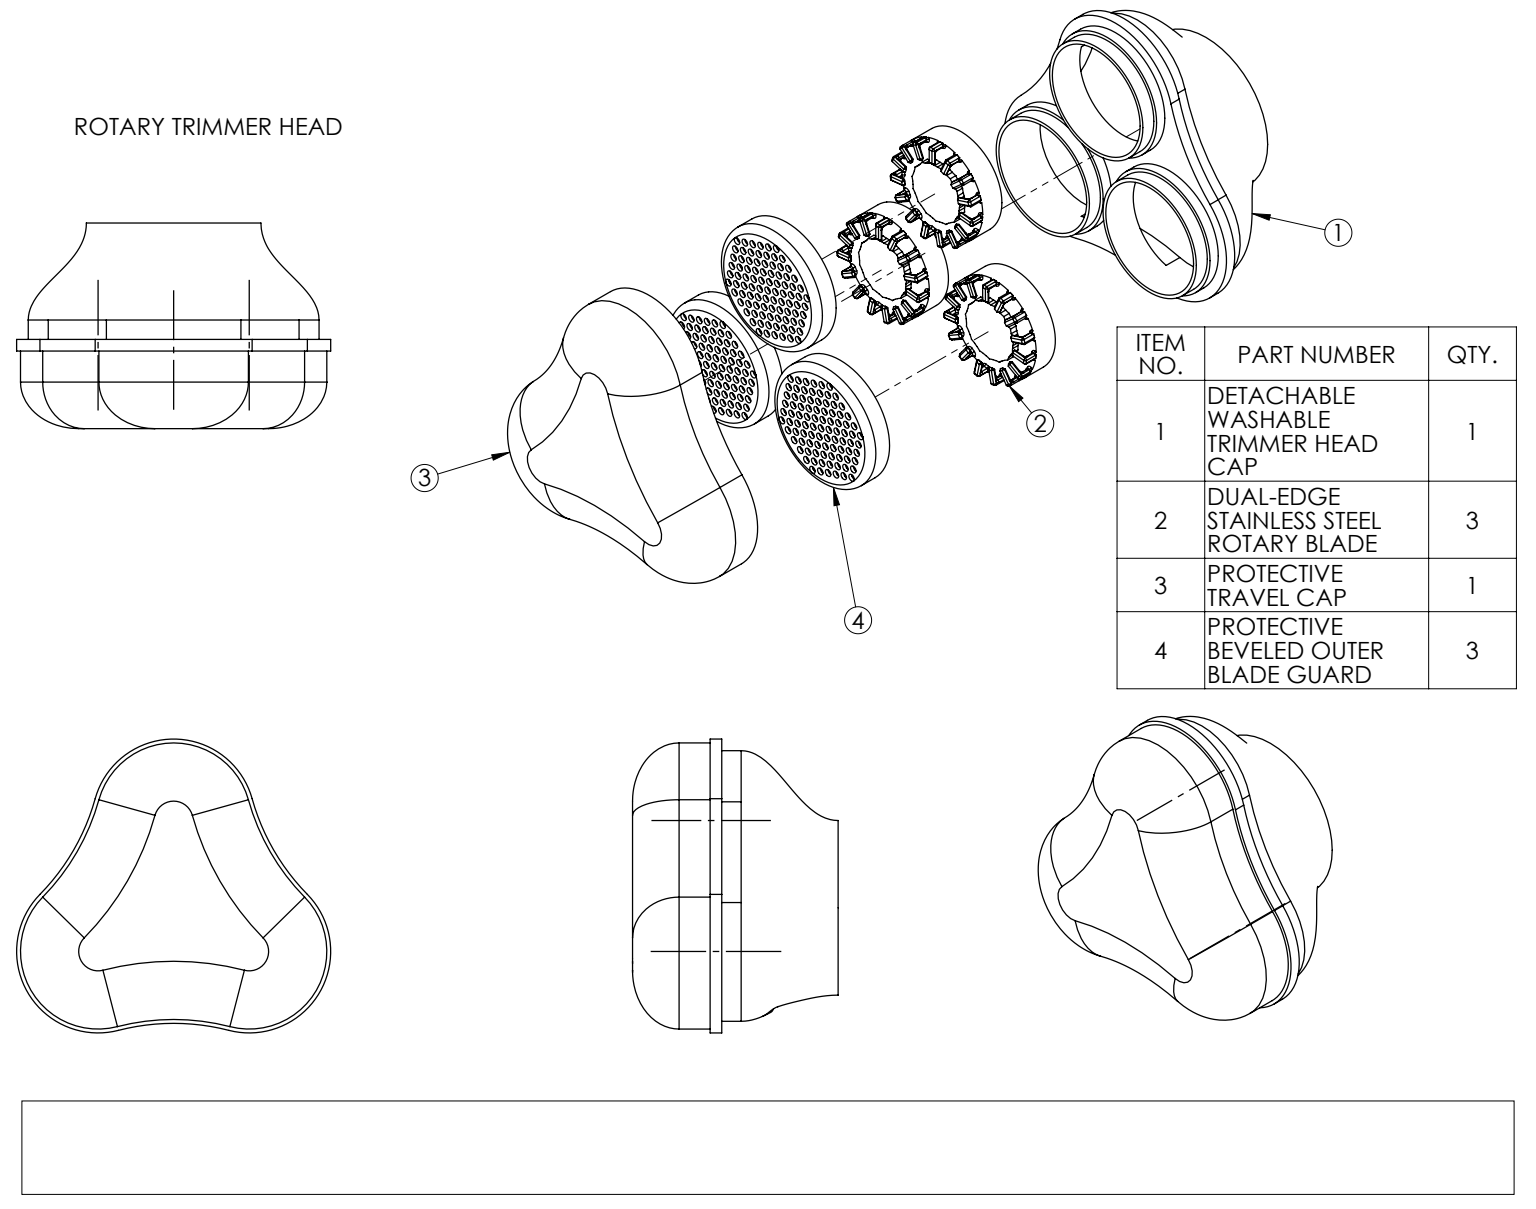
ISO-10303-21;
HEADER;
FILE_DESCRIPTION (('STEP AP214'),
    '1' );
FILE_NAME ('BR-834',
    '2026-10-04T08:29:30',
    ( '' ),
    ( '' ),
    'SwSTEP 2.0',
    'SolidWorks 2026',
    '' );
FILE_SCHEMA (( 'AUTOMOTIVE_DESIGN' ));
ENDSEC;

DATA;
#1 = DIRECTION ( 'NONE',  ( 1.000000000000000000, 0.000000000000000000, 0.000000000000000000 ) ) ;
#2 = ORIENTED_EDGE ( 'NONE', *, *, #18761, .T. ) ;
#3 = CARTESIAN_POINT ( 'NONE',  ( -6.039637753342756987, 20.17599680590523192, -26.42895019650636712 ) ) ;
#4 = DIRECTION ( 'NONE',  ( 1.000000000000000000, 0.000000000000000000, 0.000000000000000000 ) ) ;
#5 = CARTESIAN_POINT ( 'NONE',  ( 4.724371395536106633, 32.23037938972932892, 12.00000000000000000 ) ) ;
#6 = DIRECTION ( 'NONE',  ( 1.000000000000000000, 0.000000000000000000, 0.000000000000000000 ) ) ;
#7 = VERTEX_POINT ( 'NONE', #23706 ) ;
#8 = CARTESIAN_POINT ( 'NONE',  ( 30.17671132303273041, 0.02011987000799879410, -8.767782600480947153 ) ) ;
#9 = CYLINDRICAL_SURFACE ( 'NONE', #10255, 1.000000000000000000 ) ;
#10 = DIRECTION ( 'NONE',  ( 1.000000000000000000, 0.000000000000000000, 0.000000000000000000 ) ) ;
#11 = ORIENTED_EDGE ( 'NONE', *, *, #12384, .T. ) ;
#12 = CARTESIAN_POINT ( 'NONE',  ( -29.54807517884461632, 0.1037351573273601335, -10.18168607448700591 ) ) ;
#13 = DIRECTION ( 'NONE',  ( -0.2185080122244334455, 0.6724985119639524944, -0.7071067811865451302 ) ) ;
#14 = ORIENTED_EDGE ( 'NONE', *, *, #11344, .T. ) ;
#15 = CARTESIAN_POINT ( 'NONE',  ( 34.91117196809893386, -7.323106101878850360, -6.322142741489443551 ) ) ;
#16 = ORIENTED_EDGE ( 'NONE', *, *, #14456, .T. ) ;
#17 = CARTESIAN_POINT ( 'NONE',  ( 15.81286488304413318, 30.89881296429246760, 12.73282698324844375 ) ) ;
#18 = CARTESIAN_POINT ( 'NONE',  ( 18.03924190088647705, -16.85603499720526344, 20.99999999999999645 ) ) ;
#19 = FACE_OUTER_BOUND ( 'NONE', #7772, .T. ) ;
#20 = CARTESIAN_POINT ( 'NONE',  ( -6.855490822441467458, 29.74656830693323073, 20.25080042701618765 ) ) ;
#21 = CARTESIAN_POINT ( 'NONE',  ( -7.470035553104361625, 44.81454624109330354, 7.499999999999994671 ) ) ;
#22 = ORIENTED_EDGE ( 'NONE', *, *, #8423, .T. ) ;
#23 = DIRECTION ( 'NONE',  ( 0.8660254037844363761, -0.5000000000000038858, 0.000000000000000000 ) ) ;
#24 = CARTESIAN_POINT ( 'NONE',  ( 0.000000000000000000, 22.50000000000000355, 7.000000000000000000 ) ) ;
#25 = DIRECTION ( 'NONE',  ( 0.9510565162951544194, 0.3090169943749449533, -0.000000000000000000 ) ) ;
#26 = AXIS2_PLACEMENT_3D ( 'NONE', #30413, #27350, #24305 ) ;
#27 = DIRECTION ( 'NONE',  ( 0.000000000000000000, 0.000000000000000000, 1.000000000000000000 ) ) ;
#28 = CARTESIAN_POINT ( 'NONE',  ( 8.056271088701681293, 31.17318759581355536, -12.99397879114828491 ) ) ;
#29 = CARTESIAN_POINT ( 'NONE',  ( 11.44473057578109199, 31.45924896672603310, 11.00000000000000000 ) ) ;
#30 = CARTESIAN_POINT ( 'NONE',  ( 10.89305648074092225, -17.83927469781341912, -26.72577608409487127 ) ) ;
#31 = PRESENTATION_STYLE_ASSIGNMENT (( #30520 ) ) ;
#32 = PLANE ( 'NONE',  #24163 ) ;
#33 = CARTESIAN_POINT ( 'NONE',  ( -8.294006203984645609, 33.46401007850805343, 6.000000000000000000 ) ) ;
#34 = ORIENTED_EDGE ( 'NONE', *, *, #3818, .T. ) ;
#35 = CARTESIAN_POINT ( 'NONE',  ( -12.95130549116995766, 21.61585988689554227, -17.44156443216185437 ) ) ;
#36 = AXIS2_PLACEMENT_3D ( 'NONE', #271, #15908, #35000 ) ;
#37 = CARTESIAN_POINT ( 'NONE',  ( -34.17506821248604609, -14.20748230372643484, 17.42190598798392642 ) ) ;
#38 = CARTESIAN_POINT ( 'NONE',  ( 9.469227640886519026, -18.41450066817799680, -27.45857254820928262 ) ) ;
#39 = CIRCLE ( 'NONE', #2001, 1.000000000000000000 ) ;
#40 = DIRECTION ( 'NONE',  ( 1.000000000000000000, 0.000000000000000000, 0.000000000000000000 ) ) ;
#41 = EDGE_LOOP ( 'NONE', ( #16818, #38380, #12394, #9835 ) ) ;
#42 = VERTEX_POINT ( 'NONE', #38948 ) ;
#43 = CARTESIAN_POINT ( 'NONE',  ( -9.458574418659280170, 18.26235614098742843, -28.64307802517810941 ) ) ;
#44 = CARTESIAN_POINT ( 'NONE',  ( -18.65979626009148973, -26.26407584738503331, -9.537061111741776287 ) ) ;
#45 = CARTESIAN_POINT ( 'NONE',  ( 5.050662510305749642, -26.77689918168226768, 11.00000000000000178 ) ) ;
#46 = EDGE_LOOP ( 'NONE', ( #16862, #39215, #35738, #30448, #9840 ) ) ;
#47 = CARTESIAN_POINT ( 'NONE',  ( -20.13126830103601250, -6.281551959463021362, -26.35909575268052052 ) ) ;
#48 = PRODUCT_DEFINITION_CONTEXT ( 'detailed design', #8302, 'design' ) ;
#49 = CARTESIAN_POINT ( 'NONE',  ( -9.699069978481025700, -18.92072388944653127, -25.04460771491937265 ) ) ;
#50 = DIRECTION ( 'NONE',  ( 0.000000000000000000, 0.000000000000000000, 1.000000000000000000 ) ) ;
#51 = ORIENTED_EDGE ( 'NONE', *, *, #33215, .T. ) ;
#52 = CARTESIAN_POINT ( 'NONE',  ( 24.45230663209730793, 0.6563593020860170046, -18.47643289388101806 ) ) ;
#53 = DIRECTION ( 'NONE',  ( 0.000000000000000000, 0.000000000000000000, 1.000000000000000000 ) ) ;
#54 = DIRECTION ( 'NONE',  ( 0.000000000000000000, 0.000000000000000000, 1.000000000000000000 ) ) ;
#55 = VECTOR ( 'NONE', #14215, 1000.000000000000114 ) ;
#56 = ORIENTED_EDGE ( 'NONE', *, *, #7043, .F. ) ;
#57 = CARTESIAN_POINT ( 'NONE',  ( -29.40282053116814609, 0.01990383680175984021, -10.64941467521011909 ) ) ;
#58 = EDGE_LOOP ( 'NONE', ( #5255, #36161, #10685, #33701, #20952, #26926 ) ) ;
#59 = CARTESIAN_POINT ( 'NONE',  ( 25.10121631073093340, -0.7699293454477268428, -18.29635744866308400 ) ) ;
#60 = CARTESIAN_POINT ( 'NONE',  ( 8.060031444180253857, -18.86142350993543104, -30.00000000000000000 ) ) ;
#61 = CARTESIAN_POINT ( 'NONE',  ( 25.28418022016654021, -25.06680681775964104, 17.42190598798393708 ) ) ;
#62 = ADVANCED_FACE ( 'NONE', ( #11719 ), #11120, .F. ) ;
#63 = ORIENTED_EDGE ( 'NONE', *, *, #30537, .T. ) ;
#64 = CARTESIAN_POINT ( 'NONE',  ( -20.37227374329378549, 4.299522256352382499, -26.46881427764473926 ) ) ;
#65 = B_SPLINE_CURVE_WITH_KNOTS ( 'NONE', 3,
 ( #33912, #15414, #12759, #24753 ),
 .UNSPECIFIED., .F., .F.,
 ( 4, 4 ),
 ( 0.000000000000000000, 1.000000000000000000 ),
 .UNSPECIFIED. ) ;
#66 = DIRECTION ( 'NONE',  ( -0.7431448254773862505, 0.6691306063588670083, 0.000000000000000000 ) ) ;
#67 = DIRECTION ( 'NONE',  ( 0.000000000000000000, 0.000000000000000000, 1.000000000000000000 ) ) ;
#68 = AXIS2_PLACEMENT_3D ( 'NONE', #9965, #18910, #3865 ) ;
#69 = CARTESIAN_POINT ( 'NONE',  ( 13.16028273094469192, 27.30176617939681449, 7.500000000000000000 ) ) ;
#70 = EDGE_CURVE ( 'NONE', #761, #15410, #872, .T. ) ;
#71 = AXIS2_PLACEMENT_3D ( 'NONE', #37438, #19346, #24844 ) ;
#72 = DIRECTION ( 'NONE',  ( 1.000000000000000000, 0.000000000000000000, 0.000000000000000000 ) ) ;
#73 = EDGE_CURVE ( 'NONE', #19744, #23095, #8006, .T. ) ;
#74 = FACE_BOUND ( 'NONE', #6816, .T. ) ;
#75 = CARTESIAN_POINT ( 'NONE',  ( 32.33143948541893309, 1.358872982500734405, 11.55979286843934872 ) ) ;
#76 = CARTESIAN_POINT ( 'NONE',  ( -24.05674159856693706, 7.010567539539591664, -10.83448856670747062 ) ) ;
#77 = LINE ( 'NONE', #28854, #39100 ) ;
#78 = DIRECTION ( 'NONE',  ( 0.000000000000000000, 0.000000000000000000, 1.000000000000000000 ) ) ;
#79 = CARTESIAN_POINT ( 'NONE',  ( 23.11526344011869938, -26.83253816688370819, -5.449048760028999183 ) ) ;
#80 = AXIS2_PLACEMENT_3D ( 'NONE', #8723, #5868, #21115 ) ;
#81 = DIRECTION ( 'NONE',  ( 0.000000000000000000, 0.000000000000000000, 1.000000000000000000 ) ) ;
#82 = CARTESIAN_POINT ( 'NONE',  ( 11.98848786654193255, 20.09305581486839287, -20.51223356901921235 ) ) ;
#83 = ORIENTED_EDGE ( 'NONE', *, *, #31843, .F. ) ;
#84 = CARTESIAN_POINT ( 'NONE',  ( -15.67656793722190045, 23.98187497218004083, -9.264872189972811256 ) ) ;
#85 = CARTESIAN_POINT ( 'NONE',  ( -20.14416558653889666, -20.32661669692040007, 20.50957957746029336 ) ) ;
#86 = EDGE_CURVE ( 'NONE', #10650, #36352, #5018, .T. ) ;
#87 = EDGE_CURVE ( 'NONE', #32024, #8691, #8265, .T. ) ;
#88 = FACE_OUTER_BOUND ( 'NONE', #25891, .T. ) ;
#89 = CARTESIAN_POINT ( 'NONE',  ( 15.36333771843081841, 26.52970315206185958, -6.888084564221619743 ) ) ;
#90 = ORIENTED_EDGE ( 'NONE', *, *, #14466, .T. ) ;
#91 = DIRECTION ( 'NONE',  ( 1.000000000000000000, 0.000000000000000000, 0.000000000000000000 ) ) ;
#92 = EDGE_LOOP ( 'NONE', ( #13644, #34417, #27683, #7485 ) ) ;
#94 = DIRECTION ( 'NONE',  ( 1.000000000000000000, 0.000000000000000000, 0.000000000000000000 ) ) ;
#93 = CARTESIAN_POINT ( 'NONE',  ( -15.15181741199034882, 26.67644226825787612, -7.818864437366713993 ) ) ;
#95 = CARTESIAN_POINT ( 'NONE',  ( -14.89520944345796494, -25.68604227067969603, -10.17218003502877899 ) ) ;
#96 = CARTESIAN_POINT ( 'NONE',  ( -10.06946225350398194, 32.23940090176283491, 9.500000000000000000 ) ) ;
#97 = VECTOR ( 'NONE', #32100, 1000.000000000000000 ) ;
#98 = ORIENTED_EDGE ( 'NONE', *, *, #25945, .F. ) ;
#99 = CARTESIAN_POINT ( 'NONE',  ( -34.90754895111634681, -15.66705718490307753, -5.000000000000001776 ) ) ;
#100 = CARTESIAN_POINT ( 'NONE',  ( -8.710418783113659913, -18.55732502341819767, -29.36346440193179674 ) ) ;
#101 = CARTESIAN_POINT ( 'NONE',  ( -14.97283176289963968, 21.60377111278828011, 10.49999999999999645 ) ) ;
#102 = CARTESIAN_POINT ( 'NONE',  ( 14.62730537770042893, 21.61436029863431685, -14.58249002882225476 ) ) ;
#103 = ORIENTED_EDGE ( 'NONE', *, *, #28678, .T. ) ;
#104 = CARTESIAN_POINT ( 'NONE',  ( 26.12479609234808819, 4.655573347657212757, -9.320158625236146577 ) ) ;
#105 = CARTESIAN_POINT ( 'NONE',  ( 4.835130509701799362, 15.55077355964573904, 13.00000000000000178 ) ) ;
#106 = LINE ( 'NONE', #9845, #39374 ) ;
#107 = DIRECTION ( 'NONE',  ( 1.000000000000000000, 0.000000000000000000, 0.000000000000000000 ) ) ;
#108 = ORIENTED_EDGE ( 'NONE', *, *, #38694, .T. ) ;
#109 = CARTESIAN_POINT ( 'NONE',  ( -20.86432690731735562, 0.1532841330718156259, -26.77785373325384199 ) ) ;
#110 = CARTESIAN_POINT ( 'NONE',  ( 30.11859346776113000, -0.3084563647293983579, -9.685108080598787694 ) ) ;
#111 = DIRECTION ( 'NONE',  ( 0.000000000000000000, 0.000000000000000000, 1.000000000000000000 ) ) ;
#112 = CARTESIAN_POINT ( 'NONE',  ( 19.16157041420283491, -20.39791322820700259, 20.50957957746027915 ) ) ;
#113 = VERTEX_POINT ( 'NONE', #23905 ) ;
#114 = VECTOR ( 'NONE', #22519, 1000.000000000000000 ) ;
#115 = EDGE_CURVE ( 'NONE', #32074, #26123, #27464, .T. ) ;
#116 = CARTESIAN_POINT ( 'NONE',  ( 19.54664213359407654, -11.28525909758385914, -19.69475445967423610 ) ) ;
#117 = DIRECTION ( 'NONE',  ( 0.1045284632676436315, -0.9945218953682742891, 0.000000000000000000 ) ) ;
#118 = ORIENTED_EDGE ( 'NONE', *, *, #842, .F. ) ;
#119 = CARTESIAN_POINT ( 'NONE',  ( 14.09933648065468503, 26.02968990214154843, 7.500000000000000888 ) ) ;
#120 = CARTESIAN_POINT ( 'NONE',  ( -33.75875814100324135, 2.759858869446477403, 22.99999999999999645 ) ) ;
#121 = DIRECTION ( 'NONE',  ( 0.5446390350150238646, -0.8386705679454261597, 0.000000000000000000 ) ) ;
#122 = CARTESIAN_POINT ( 'NONE',  ( 0.8345715822200899803, 20.57921025466891507, -28.44513613269969099 ) ) ;
#123 = CARTESIAN_POINT ( 'NONE',  ( 0.000000000000000000, 22.50000000000000355, 6.000000000000000000 ) ) ;
#124 = DIRECTION ( 'NONE',  ( 1.000000000000000000, 3.469446951953568829E-15, 0.000000000000000000 ) ) ;
#125 = FACE_OUTER_BOUND ( 'NONE', #14098, .T. ) ;
#126 = LINE ( 'NONE', #12516, #37440 ) ;
#127 = CARTESIAN_POINT ( 'NONE',  ( 11.77212950435618488, 31.79629403205455063, 7.338691926023207301 ) ) ;
#128 = CARTESIAN_POINT ( 'NONE',  ( 14.95529536635265089, 27.95853494889172808, -6.397368112980813315 ) ) ;
#129 = CYLINDRICAL_SURFACE ( 'NONE', #3554, 0.5000000000000004441 ) ;
#130 = ORIENTED_EDGE ( 'NONE', *, *, #22039, .F. ) ;
#132 = FACE_OUTER_BOUND ( 'NONE', #27069, .T. ) ;
#131 = CARTESIAN_POINT ( 'NONE',  ( -14.93930595609077372, 14.05784520172980834, -29.41333909553293680 ) ) ;
#133 = CARTESIAN_POINT ( 'NONE',  ( 29.92393930195780527, -26.04303208588360263, 11.00000000000002132 ) ) ;
#134 = AXIS2_PLACEMENT_3D ( 'NONE', #36095, #30198, #27342 ) ;
#135 = CARTESIAN_POINT ( 'NONE',  ( 15.46971733045241670, -26.73784336799789330, -5.000000000000000000 ) ) ;
#136 = ADVANCED_FACE ( 'NONE', ( #30004 ), #2180, .T. ) ;
#137 = CARTESIAN_POINT ( 'NONE',  ( -22.79932625038946981, -26.94340799757786442, -5.449688136485410617 ) ) ;
#138 = CARTESIAN_POINT ( 'NONE',  ( 11.00941871237314906, 17.34598387146357013, -28.70709525229845838 ) ) ;
#139 = B_SPLINE_CURVE_WITH_KNOTS ( 'NONE', 3,
 ( #14310, #17577, #20620, #36259, #23258, #23855, #38896, #35449 ),
 .UNSPECIFIED., .F., .F.,
 ( 4, 2, 2, 4 ),
 ( 0.000000000000000000, 0.0004726692273637091287, 0.0007090038410455639642, 0.0009453384547274186912 ),
 .UNSPECIFIED. ) ;
#140 = CARTESIAN_POINT ( 'NONE',  ( 11.46362546061642718, 18.45517822843765643, -23.85068629872059986 ) ) ;
#141 = ORIENTED_EDGE ( 'NONE', *, *, #26869, .T. ) ;
#142 = FACE_OUTER_BOUND ( 'NONE', #24319, .T. ) ;
#143 = CARTESIAN_POINT ( 'NONE',  ( -9.432189322962019062, -18.20121415529274600, -30.00000000000000000 ) ) ;
#144 = CARTESIAN_POINT ( 'NONE',  ( -35.54328883424743424, -18.34041411986772019, 13.92931973827826297 ) ) ;
#145 = AXIS2_PLACEMENT_3D ( 'NONE', #32280, #11698, #11498 ) ;
#146 = CARTESIAN_POINT ( 'NONE',  ( -28.29430579339429386, -20.85964472249671076, -11.08156269910200109 ) ) ;
#147 = CARTESIAN_POINT ( 'NONE',  ( -0.3376553287050821917, -22.96943114444468392, -15.94602349255009521 ) ) ;
#148 = CARTESIAN_POINT ( 'NONE',  ( 12.89389314760598104, 20.70404999538203228, -18.49322484050768267 ) ) ;
#149 = CARTESIAN_POINT ( 'NONE',  ( 21.24142803452728501, 10.67320610155583971, -12.88465657304564083 ) ) ;
#150 = CARTESIAN_POINT ( 'NONE',  ( -8.927394655428429360, 11.06314620770957013, 11.00000000000000000 ) ) ;
#151 = ORIENTED_EDGE ( 'NONE', *, *, #23785, .T. ) ;
#152 = CARTESIAN_POINT ( 'NONE',  ( -34.78690698786454760, -6.577732317142261032, -5.889322506088498166 ) ) ;
#153 = CARTESIAN_POINT ( 'NONE',  ( -20.57776646309937263, 11.88057900678980872, 17.42190598798392998 ) ) ;
#154 = VECTOR ( 'NONE', #35200, 1000.000000000000000 ) ;
#155 = ORIENTED_EDGE ( 'NONE', *, *, #21487, .F. ) ;
#156 = CYLINDRICAL_SURFACE ( 'NONE', #5742, 0.5000000000000004441 ) ;
#157 = DIRECTION ( 'NONE',  ( -0.1045284632676566766, -0.9945218953682730678, 0.000000000000000000 ) ) ;
#158 = CARTESIAN_POINT ( 'NONE',  ( -22.13218141308518483, 1.022649068119683147, -22.77793944450150931 ) ) ;
#159 = EDGE_CURVE ( 'NONE', #19442, #37263, #30806, .T. ) ;
#160 = CARTESIAN_POINT ( 'NONE',  ( 20.77567436899659725, -6.972680293972757681, -24.33364738463043153 ) ) ;
#161 = CARTESIAN_POINT ( 'NONE',  ( 35.73872160561271727, -18.42674013420386459, 13.32518128616613140 ) ) ;
#162 = EDGE_CURVE ( 'NONE', #21531, #36577, #11917, .T. ) ;
#163 = VERTEX_POINT ( 'NONE', #30609 ) ;
#164 = EDGE_CURVE ( 'NONE', #16334, #15391, #9293, .T. ) ;
#165 = CARTESIAN_POINT ( 'NONE',  ( 6.654030453887980201, 35.94335816374507431, 7.500000000000000888 ) ) ;
#166 = ORIENTED_EDGE ( 'NONE', *, *, #36174, .F. ) ;
#167 = DIRECTION ( 'NONE',  ( -1.000000000000000000, 0.000000000000000000, 0.000000000000000000 ) ) ;
#168 = DIRECTION ( 'NONE',  ( 1.000000000000000000, 0.000000000000000000, 0.000000000000000000 ) ) ;
#169 = EDGE_CURVE ( 'NONE', #13627, #24692, #9468, .T. ) ;
#170 = VECTOR ( 'NONE', #21979, 1000.000000000000000 ) ;
#171 = CARTESIAN_POINT ( 'NONE',  ( 0.000000000000000000, 22.50000000000000355, 7.000000000000000000 ) ) ;
#172 = VERTEX_POINT ( 'NONE', #15755 ) ;
#173 = CARTESIAN_POINT ( 'NONE',  ( -3.068187625016429276, 38.20266742920320269, -4.999999999999997335 ) ) ;
#174 = DIRECTION ( 'NONE',  ( 0.000000000000000000, 0.000000000000000000, -1.000000000000000000 ) ) ;
#175 = DIRECTION ( 'NONE',  ( 1.000000000000000000, 0.000000000000000000, 0.000000000000000000 ) ) ;
#176 = B_SPLINE_CURVE_WITH_KNOTS ( 'NONE', 3,
 ( #11426, #39044, #29102, #33170, #14266, #32361 ),
 .UNSPECIFIED., .F., .F.,
 ( 4, 2, 4 ),
 ( 0.000000000000000000, 0.4999999999999998890, 1.000000000000000000 ),
 .UNSPECIFIED. ) ;
#177 = DIRECTION ( 'NONE',  ( 0.000000000000000000, 0.000000000000000000, -1.000000000000000000 ) ) ;
#178 = CARTESIAN_POINT ( 'NONE',  ( 14.47283171447379146, 21.48159823030311344, 7.500000000000010658 ) ) ;
#179 = CARTESIAN_POINT ( 'NONE',  ( 13.42433502267052958, 29.97960619171108476, -8.615981373113749342 ) ) ;
#180 = ORIENTED_EDGE ( 'NONE', *, *, #19438, .T. ) ;
#181 = CARTESIAN_POINT ( 'NONE',  ( -18.60936157838533589, 11.09020867803737609, -21.18208952860758387 ) ) ;
#182 = CARTESIAN_POINT ( 'NONE',  ( -2.109373541296176047, 27.06550157850341520, 23.00000000000000000 ) ) ;
#183 = CARTESIAN_POINT ( 'NONE',  ( 15.61814132907574759, -26.77569883083870650, -5.473565389543558091 ) ) ;
#184 = LINE ( 'NONE', #27415, #10010 ) ;
#185 = CARTESIAN_POINT ( 'NONE',  ( 11.02015971874664224, 17.53795386546354962, -27.44368206178839387 ) ) ;
#186 = EDGE_CURVE ( 'NONE', #15751, #12988, #40137, .T. ) ;
#187 = CARTESIAN_POINT ( 'NONE',  ( -13.28992586503615847, -18.25382200079944539, -30.00000000000000711 ) ) ;
#188 = LINE ( 'NONE', #25168, #20681 ) ;
#189 = EDGE_CURVE ( 'NONE', #7975, #16887, #8966, .T. ) ;
#190 = AXIS2_PLACEMENT_3D ( 'NONE', #26813, #7919, #22957 ) ;
#191 = CARTESIAN_POINT ( 'NONE',  ( -15.40573053741202791, 26.82015453055286969, -5.474029462766525356 ) ) ;
#192 = CARTESIAN_POINT ( 'NONE',  ( -23.94859168923916215, -23.92721191009457726, -11.16030928171529979 ) ) ;
#193 = CARTESIAN_POINT ( 'NONE',  ( 10.29923522730770280, -24.86304583090714004, -10.26489670867711546 ) ) ;
#194 = CARTESIAN_POINT ( 'NONE',  ( 11.75310639014839431, 18.84718256836299588, -22.74606834583529036 ) ) ;
#195 = CARTESIAN_POINT ( 'NONE',  ( 27.78181535516823786, -20.09500351851029265, -11.98703701457788462 ) ) ;
#196 = CIRCLE ( 'NONE', #16433, 1.000000000000000888 ) ;
#197 = CARTESIAN_POINT ( 'NONE',  ( -9.677076426724102731, 26.69573495723219736, 10.50000000000000000 ) ) ;
#198 = ORIENTED_EDGE ( 'NONE', *, *, #35032, .T. ) ;
#199 = CARTESIAN_POINT ( 'NONE',  ( -9.363295122093004963, 31.29718702830158605, -12.10286225948017602 ) ) ;
#200 = CARTESIAN_POINT ( 'NONE',  ( 19.48557158514988075, -11.24999999999998224, 6.000000000000000000 ) ) ;
#201 = CARTESIAN_POINT ( 'NONE',  ( -8.306370210276497801, 9.993911548625852959, 10.49999999999999822 ) ) ;
#202 = LINE ( 'NONE', #23984, #35140 ) ;
#203 = ORIENTED_EDGE ( 'NONE', *, *, #26918, .F. ) ;
#204 = CARTESIAN_POINT ( 'NONE',  ( 20.69210506600241217, 0.8672995041115374448, -27.44967104096003396 ) ) ;
#205 = DIRECTION ( 'NONE',  ( 0.000000000000000000, 0.000000000000000000, 1.000000000000000000 ) ) ;
#206 = DIRECTION ( 'NONE',  ( 0.000000000000000000, 0.000000000000000000, 1.000000000000000000 ) ) ;
#207 = ORIENTED_EDGE ( 'NONE', *, *, #30268, .T. ) ;
#208 = CARTESIAN_POINT ( 'NONE',  ( -20.60935208275203578, 0.8679898295200253466, -28.07838543686035493 ) ) ;
#209 = DIRECTION ( 'NONE',  ( 0.6123724356958052395, 0.3535533905932595200, -0.7071067811865454633 ) ) ;
#210 = EDGE_CURVE ( 'NONE', #22927, #29202, #39935, .T. ) ;
#211 = VECTOR ( 'NONE', #28552, 1000.000000000000000 ) ;
#212 = ORIENTED_EDGE ( 'NONE', *, *, #665, .T. ) ;
#213 = CARTESIAN_POINT ( 'NONE',  ( 21.39727014468892108, -3.719077462541732437, -24.55904260327581667 ) ) ;
#214 = AXIS2_PLACEMENT_3D ( 'NONE', #6009, #9672, #24306 ) ;
#215 = EDGE_CURVE ( 'NONE', #19575, #30083, #1517, .T. ) ;
#216 = EDGE_LOOP ( 'NONE', ( #4536, #16133, #31309, #14302 ) ) ;
#217 = CARTESIAN_POINT ( 'NONE',  ( 5.726446540400058183, 39.49945686212564055, 12.14047268033097460 ) ) ;
#218 = PLANE ( 'NONE',  #11258 ) ;
#219 = AXIS2_PLACEMENT_3D ( 'NONE', #21595, #14504, #26896 ) ;
#220 = CARTESIAN_POINT ( 'NONE',  ( 2.629601561899395534, 7.723830143584016206, 10.49999999999999822 ) ) ;
#221 = CARTESIAN_POINT ( 'NONE',  ( 10.34254640628217992, 25.37474234120047001, 19.99202127657103389 ) ) ;
#222 = STYLED_ITEM ( 'NONE', ( #29995 ), #8155 ) ;
#223 = ADVANCED_FACE ( 'NONE', ( #15359 ), #322, .F. ) ;
#224 = CARTESIAN_POINT ( 'NONE',  ( 5.288651019504051476, 36.01756689786824239, 10.83333333333333393 ) ) ;
#225 = ORIENTED_EDGE ( 'NONE', *, *, #29984, .F. ) ;
#226 = FACE_OUTER_BOUND ( 'NONE', #33759, .T. ) ;
#227 = CARTESIAN_POINT ( 'NONE',  ( -17.67638173720171935, 10.46809921990191228, -30.00000000000000355 ) ) ;
#228 =( GEOMETRIC_REPRESENTATION_CONTEXT ( 3 ) GLOBAL_UNCERTAINTY_ASSIGNED_CONTEXT ( ( #6136 ) ) GLOBAL_UNIT_ASSIGNED_CONTEXT ( ( #10558, #26390, #22941 ) ) REPRESENTATION_CONTEXT ( 'NONE', 'WORKASPACE' ) );
#229 = FACE_OUTER_BOUND ( 'NONE', #25110, .T. ) ;
#230 = DIRECTION ( 'NONE',  ( 0.000000000000000000, 0.000000000000000000, 1.000000000000000000 ) ) ;
#231 = CARTESIAN_POINT ( 'NONE',  ( 8.287352997579366942, 32.06355925594149880, -12.06759070029764480 ) ) ;
#232 = AXIS2_PLACEMENT_3D ( 'NONE', #21106, #26799, #8514 ) ;
#233 = CARTESIAN_POINT ( 'NONE',  ( 15.92400346575717762, -24.84455697418767528, -12.40895801513320507 ) ) ;
#234 = DIRECTION ( 'NONE',  ( -0.000000000000000000, -0.000000000000000000, -1.000000000000000000 ) ) ;
#235 = DIRECTION ( 'NONE',  ( 0.000000000000000000, 0.000000000000000000, 1.000000000000000000 ) ) ;
#236 = EDGE_CURVE ( 'NONE', #29069, #1872, #12116, .T. ) ;
#237 = EDGE_LOOP ( 'NONE', ( #9320, #17479 ) ) ;
#238 = CARTESIAN_POINT ( 'NONE',  ( -11.15269954372922356, 17.20160742699127709, -29.35198317640747234 ) ) ;
#239 = CIRCLE ( 'NONE', #18429, 0.5000000000000004441 ) ;
#240 = CARTESIAN_POINT ( 'NONE',  ( -22.07435099023991043, -25.45711610480719145, 17.92354375535213151 ) ) ;
#241 = CARTESIAN_POINT ( 'NONE',  ( 12.53737549699592435, -22.55629599919020123, -16.45275500735702323 ) ) ;
#242 = CARTESIAN_POINT ( 'NONE',  ( -7.559512017365658920, 19.71884705062586107, 13.00000000000000178 ) ) ;
#243 = ORIENTED_EDGE ( 'NONE', *, *, #35669, .F. ) ;
#244 = ORIENTED_EDGE ( 'NONE', *, *, #2667, .T. ) ;
#245 = CARTESIAN_POINT ( 'NONE',  ( -12.34506054626673333, 24.84528727421060523, -15.23039115023100543 ) ) ;
#246 = CARTESIAN_POINT ( 'NONE',  ( -12.69359228199308376, -19.47210042018829768, -21.37302842195050800 ) ) ;
#247 = FACE_BOUND ( 'NONE', #237, .T. ) ;
#248 = CIRCLE ( 'NONE', #15817, 0.5000000000000004441 ) ;
#249 = ORIENTED_EDGE ( 'NONE', *, *, #12112, .F. ) ;
#250 = CARTESIAN_POINT ( 'NONE',  ( -34.76827517156570480, -10.82915826946258697, -8.018781004229030174 ) ) ;
#251 = CARTESIAN_POINT ( 'NONE',  ( -10.41464456071557265, -19.61101364636477484, -22.74980965849629300 ) ) ;
#252 = DIRECTION ( 'NONE',  ( 0.9781476007338072431, 0.2079116908177519041, 0.000000000000000000 ) ) ;
#253 = VERTEX_POINT ( 'NONE', #30414 ) ;
#254 = CARTESIAN_POINT ( 'NONE',  ( 26.95107570311581213, 1.250167503761063559, -13.57310776412708897 ) ) ;
#255 = CARTESIAN_POINT ( 'NONE',  ( 5.100636323082810009, 29.29593658752792962, 6.000000000000000000 ) ) ;
#256 = DIRECTION ( 'NONE',  ( 0.000000000000000000, 0.000000000000000000, 1.000000000000000000 ) ) ;
#257 = VERTEX_POINT ( 'NONE', #18219 ) ;
#258 = CARTESIAN_POINT ( 'NONE',  ( -25.23791706649960176, 0.3308843942117839498, -17.43238208906259601 ) ) ;
#259 = ORIENTED_EDGE ( 'NONE', *, *, #8002, .F. ) ;
#260 = CARTESIAN_POINT ( 'NONE',  ( 20.49417979596975314, -0.6040919881699248206, -29.32140277093775893 ) ) ;
#261 = VECTOR ( 'NONE', #29396, 1000.000000000000000 ) ;
#262 = CARTESIAN_POINT ( 'NONE',  ( 17.66709127915118671, -10.40404091307350143, -30.00000000000003553 ) ) ;
#263 = CARTESIAN_POINT ( 'NONE',  ( 33.08368474897510225, -6.388390677200520784, 17.92354375535212085 ) ) ;
#264 = EDGE_CURVE ( 'NONE', #18645, #2968, #39539, .T. ) ;
#265 = ORIENTED_EDGE ( 'NONE', *, *, #11360, .F. ) ;
#266 = CARTESIAN_POINT ( 'NONE',  ( -26.84733007877831312, 4.410852123475765829, -6.430833405535962832 ) ) ;
#267 = DIRECTION ( 'NONE',  ( 0.7431448254773953543, 0.6691306063588571273, 0.000000000000000000 ) ) ;
#268 = CARTESIAN_POINT ( 'NONE',  ( 4.441848239913406715, 24.85865334748807953, 21.00000000000000355 ) ) ;
#269 = AXIS2_PLACEMENT_3D ( 'NONE', #36604, #30517, #27454 ) ;
#270 = DIRECTION ( 'NONE',  ( 0.000000000000000000, 0.000000000000000000, 1.000000000000000000 ) ) ;
#271 = CARTESIAN_POINT ( 'NONE',  ( -8.118377661053489902, 10.47536095541709322, 9.000000000000001776 ) ) ;
#272 = PRODUCT_DEFINITION_SHAPE ( 'NONE', 'NONE',  #1580 ) ;
#273 = VECTOR ( 'NONE', #6219, 1000.000000000000000 ) ;
#274 = FACE_BOUND ( 'NONE', #33600, .T. ) ;
#275 = CARTESIAN_POINT ( 'NONE',  ( 17.89938016353245942, 22.15910768081766946, 14.53008259252595025 ) ) ;
#276 = CARTESIAN_POINT ( 'NONE',  ( -24.00624866131704493, 7.997915524243389918, -7.901842696615398509 ) ) ;
#277 = CARTESIAN_POINT ( 'NONE',  ( 8.137585970692082782, 29.15429895402929361, 11.00000000000000000 ) ) ;
#278 = DIRECTION ( 'NONE',  ( 1.000000000000000000, 0.000000000000000000, 0.000000000000000000 ) ) ;
#279 = CARTESIAN_POINT ( 'NONE',  ( 24.11167876243596098, -26.47814462355511367, -6.319563270833929103 ) ) ;
#280 = CARTESIAN_POINT ( 'NONE',  ( -9.356056665764020508, 26.06569820189716324, 10.50000000000000533 ) ) ;
#281 = CARTESIAN_POINT ( 'NONE',  ( 15.24364315846217899, 26.94041793836633403, -6.881005480939310637 ) ) ;
#282 = ORIENTED_EDGE ( 'NONE', *, *, #11860, .T. ) ;
#283 = AXIS2_PLACEMENT_3D ( 'NONE', #15158, #26953, #5218 ) ;
#284 = CARTESIAN_POINT ( 'NONE',  ( -15.22236539853330761, 22.23089076743169912, -12.63797464781087676 ) ) ;
#285 = CARTESIAN_POINT ( 'NONE',  ( -27.67544922579230615, -7.282050787523742130, 20.50957957746029336 ) ) ;
#286 = ADVANCED_FACE ( 'NONE', ( #33861 ), #24901, .T. ) ;
#287 = LINE ( 'NONE', #25064, #8816 ) ;
#288 = CARTESIAN_POINT ( 'NONE',  ( 14.31318613898417524, 24.41519415167184803, -12.55250302939356821 ) ) ;
#289 = EDGE_LOOP ( 'NONE', ( #19488, #26739, #33941, #35393 ) ) ;
#290 = EDGE_CURVE ( 'NONE', #7488, #10226, #26444, .T. ) ;
#291 = DIRECTION ( 'NONE',  ( 0.9781476007338042455, -0.2079116908177663647, 0.000000000000000000 ) ) ;
#292 = ORIENTED_EDGE ( 'NONE', *, *, #22586, .T. ) ;
#294 = LINE ( 'NONE', #21426, #16002 ) ;
#293 = CARTESIAN_POINT ( 'NONE',  ( -10.86943063858312364, 17.38123995523577037, -29.34587341292847995 ) ) ;
#295 = CARTESIAN_POINT ( 'NONE',  ( -15.32260095203325001, -26.31805409878302271, -8.292144503809835143 ) ) ;
#296 = DIRECTION ( 'NONE',  ( 0.000000000000000000, 0.000000000000000000, 1.000000000000000000 ) ) ;
#297 = ORIENTED_EDGE ( 'NONE', *, *, #12319, .F. ) ;
#298 = CARTESIAN_POINT ( 'NONE',  ( -26.12381248617423068, -12.68530465514329997, -16.63598258512395489 ) ) ;
#299 = CARTESIAN_POINT ( 'NONE',  ( -14.44360165411499786, -26.36321174074733165, -6.890051424692051896 ) ) ;
#300 = PLANE ( 'NONE',  #32607 ) ;
#301 = CARTESIAN_POINT ( 'NONE',  ( 13.00986382136603048, 17.59953731938587040, -22.93413497736658258 ) ) ;
#302 = ORIENTED_EDGE ( 'NONE', *, *, #4167, .F. ) ;
#303 = CARTESIAN_POINT ( 'NONE',  ( 23.03828965240228754, 4.549470553047555654, -17.79268152331741604 ) ) ;
#304 = DIRECTION ( 'NONE',  ( 0.000000000000000000, 0.000000000000000000, 1.000000000000000000 ) ) ;
#305 = CARTESIAN_POINT ( 'NONE',  ( 9.541469607472739867, 17.40487552589537401, 13.00000000000000178 ) ) ;
#306 = EDGE_CURVE ( 'NONE', #11401, #17187, #24700, .T. ) ;
#307 = DIRECTION ( 'NONE',  ( 0.000000000000000000, 0.000000000000000000, -1.000000000000000000 ) ) ;
#308 = EDGE_LOOP ( 'NONE', ( #12738, #38655, #19382, #26352 ) ) ;
#309 = CARTESIAN_POINT ( 'NONE',  ( -22.83159479309421869, 0.2693187709842888578, -21.57099463304014364 ) ) ;
#310 = VECTOR ( 'NONE', #30674, 1000.000000000000114 ) ;
#311 = CARTESIAN_POINT ( 'NONE',  ( 30.96672106747950792, -0.2830252396438242557, -6.880588437363266863 ) ) ;
#312 = CARTESIAN_POINT ( 'NONE',  ( 27.76392016787571038, -12.00403709334112534, 20.69868183039782039 ) ) ;
#313 = ORIENTED_EDGE ( 'NONE', *, *, #4707, .F. ) ;
#314 = CIRCLE ( 'NONE', #1622, 1.000000000000000888 ) ;
#315 = CARTESIAN_POINT ( 'NONE',  ( -8.937590682902627037, -20.71651963383551731, -30.00000000000000000 ) ) ;
#316 = LINE ( 'NONE', #21645, #40068 ) ;
#317 = CIRCLE ( 'NONE', #3523, 1.000000000000000000 ) ;
#318 = EDGE_LOOP ( 'NONE', ( #14973, #38977, #20245, #19537 ) ) ;
#319 = ADVANCED_FACE ( 'NONE', ( #18023 ), #21649, .T. ) ;
#320 = CARTESIAN_POINT ( 'NONE',  ( -13.48130249190472796, 27.93180293473203690, 10.50000000000000533 ) ) ;
#321 = CARTESIAN_POINT ( 'NONE',  ( -19.26948696230206082, 27.85601271560033609, 11.00000000000000000 ) ) ;
#322 = CYLINDRICAL_SURFACE ( 'NONE', #16452, 1.000000000000000000 ) ;
#323 = CARTESIAN_POINT ( 'NONE',  ( 1.450876755219358882, 20.54457168034460679, -28.44848653506505443 ) ) ;
#324 = DIRECTION ( 'NONE',  ( -0.000000000000000000, -0.000000000000000000, -1.000000000000000000 ) ) ;
#325 = CARTESIAN_POINT ( 'NONE',  ( -16.00000000000000000, 22.50000000000000711, 13.00000000000000178 ) ) ;
#326 = DIRECTION ( 'NONE',  ( -0.2079116908177664480, -0.9781476007338042455, 0.000000000000000000 ) ) ;
#327 = CARTESIAN_POINT ( 'NONE',  ( 2.853166178176219425, 23.42705098312512746, 6.000000000000000000 ) ) ;
#328 = CARTESIAN_POINT ( 'NONE',  ( 12.80736835487433289, 15.68301270189216545, 9.000000000000001776 ) ) ;
#329 = DIRECTION ( 'NONE',  ( 0.000000000000000000, 0.000000000000000000, 1.000000000000000000 ) ) ;
#330 = CIRCLE ( 'NONE', #13283, 56.99999999999991473 ) ;
#331 = CARTESIAN_POINT ( 'NONE',  ( 12.99210526215103556, 23.76632269208105441, -15.34428991681221532 ) ) ;
#332 = DIRECTION ( 'NONE',  ( -0.2079116908177667256, -0.9781476007338041345, 1.734723475976808475E-15 ) ) ;
#333 = VERTEX_POINT ( 'NONE', #8869 ) ;
#335 = CARTESIAN_POINT ( 'NONE',  ( 8.593266739736579396, 16.38397459621552699, 11.00000000000000000 ) ) ;
#334 = CARTESIAN_POINT ( 'NONE',  ( -16.63603619446163862, 16.45028161191871874, -16.85965045874825563 ) ) ;
#336 = DIRECTION ( 'NONE',  ( -0.000000000000000000, -0.000000000000000000, 1.000000000000000000 ) ) ;
#337 = EDGE_CURVE ( 'NONE', #7337, #4065, #33318, .T. ) ;
#338 = CARTESIAN_POINT ( 'NONE',  ( 9.776760815194750265, -18.56791727838074380, -26.22569070247839917 ) ) ;
#339 = CARTESIAN_POINT ( 'NONE',  ( -21.82450030762573689, -25.89388939475013629, -9.434448713217458149 ) ) ;
#340 = CARTESIAN_POINT ( 'NONE',  ( 15.37031333667682098, 26.67843416892376496, -6.417118344468947910 ) ) ;
#341 = CARTESIAN_POINT ( 'NONE',  ( 14.28094865762740007, 24.49797395571547654, -12.54832579113776880 ) ) ;
#342 = VERTEX_POINT ( 'NONE', #31587 ) ;
#343 = VECTOR ( 'NONE', #22858, 1000.000000000000000 ) ;
#344 = CARTESIAN_POINT ( 'NONE',  ( 1.247466774197339978, 28.36888560440311480, 12.00000000000000000 ) ) ;
#345 = CARTESIAN_POINT ( 'NONE',  ( -12.21665226880467614, -22.02497210351782542, -17.44395964285717326 ) ) ;
#346 = CARTESIAN_POINT ( 'NONE',  ( -15.07283634910000814, -28.35394831540519789, 13.32518128616608877 ) ) ;
#347 = VECTOR ( 'NONE', #26561, 1000.000000000000000 ) ;
#348 = CIRCLE ( 'NONE', #38038, 1.000000000000000000 ) ;
#349 = CARTESIAN_POINT ( 'NONE',  ( -16.60566614357999171, -12.18170714992408499, -28.45539122509774899 ) ) ;
#350 = CARTESIAN_POINT ( 'NONE',  ( -0.2655791104724142260, -20.51720577492729092, -28.86250569332989002 ) ) ;
#351 = CARTESIAN_POINT ( 'NONE',  ( 15.20852936758548779, 24.97080914613512448, -9.721994908021176940 ) ) ;
#352 = EDGE_CURVE ( 'NONE', #2306, #34064, #29151, .T. ) ;
#353 = CARTESIAN_POINT ( 'NONE',  ( 21.80268670686854549, 10.92046029907020888, -9.886650491983484557 ) ) ;
#354 = CARTESIAN_POINT ( 'NONE',  ( -10.44103466624267185, 32.57396620494226624, 7.000000000000000000 ) ) ;
#355 = EDGE_CURVE ( 'NONE', #35064, #7027, #28384, .T. ) ;
#356 = ORIENTED_EDGE ( 'NONE', *, *, #17824, .F. ) ;
#357 = CARTESIAN_POINT ( 'NONE',  ( -22.70368315883370158, -2.084503118412175393, -22.39977614792177008 ) ) ;
#358 = CARTESIAN_POINT ( 'NONE',  ( -13.22866120779437438, 26.17694675927630499, 18.42518152272108978 ) ) ;
#359 = ORIENTED_EDGE ( 'NONE', *, *, #3116, .F. ) ;
#360 = LINE ( 'NONE', #21297, #8908 ) ;
#361 = DIRECTION ( 'NONE',  ( -0.9781476007338043566, 0.2079116908177657264, 0.000000000000000000 ) ) ;
#362 = CARTESIAN_POINT ( 'NONE',  ( -22.08665753359741402, 1.201892654560031248, -22.79865112719603459 ) ) ;
#363 = CARTESIAN_POINT ( 'NONE',  ( 35.20762394452638944, -14.18514843260475011, -5.860995113772236920 ) ) ;
#364 = CARTESIAN_POINT ( 'NONE',  ( 15.12590024503159114, -28.14827041158712717, 13.92931973827808889 ) ) ;
#365 = B_SPLINE_CURVE_WITH_KNOTS ( 'NONE', 3,
 ( #13662, #35008, #16115, #477 ),
 .UNSPECIFIED., .F., .F.,
 ( 4, 4 ),
 ( 0.0008976806579034594512, 0.0009453384547274206427 ),
 .UNSPECIFIED. ) ;
#366 = EDGE_LOOP ( 'NONE', ( #29228, #30799, #2804, #38071 ) ) ;
#367 = EDGE_CURVE ( 'NONE', #32326, #14728, #6690, .T. ) ;
#368 = DIRECTION ( 'NONE',  ( -0.000000000000000000, -0.000000000000000000, 1.000000000000000000 ) ) ;
#369 = ORIENTED_EDGE ( 'NONE', *, *, #70, .F. ) ;
#370 = EDGE_CURVE ( 'NONE', #7748, #33664, #16357, .T. ) ;
#371 = DIRECTION ( 'NONE',  ( 0.4156269377774552409, 0.5720614028176769228, 0.7071067811865524577 ) ) ;
#372 = CIRCLE ( 'NONE', #2976, 1.000000000000000000 ) ;
#373 = CARTESIAN_POINT ( 'NONE',  ( 27.36225479881369793, 10.16098284217389924, 11.00000000000000000 ) ) ;
#374 = AXIS2_PLACEMENT_3D ( 'NONE', #5565, #29757, #14717 ) ;
#375 = AXIS2_PLACEMENT_3D ( 'NONE', #24776, #21926, #21529 ) ;
#376 = FACE_OUTER_BOUND ( 'NONE', #28764, .T. ) ;
#377 = EDGE_LOOP ( 'NONE', ( #16222, #29568, #22970, #4101 ) ) ;
#378 = CARTESIAN_POINT ( 'NONE',  ( -2.141861647269084123, 26.68515866033992623, -18.63047281487552098 ) ) ;
#379 = CARTESIAN_POINT ( 'NONE',  ( -9.337241587065845394, 10.76617146908760247, 10.49999999999999822 ) ) ;
#380 = CARTESIAN_POINT ( 'NONE',  ( -9.625795778762141097, 10.95253033666833709, 10.50000000000000533 ) ) ;
#381 = DIRECTION ( 'NONE',  ( -0.000000000000000000, -0.000000000000000000, -1.000000000000000000 ) ) ;
#382 = CARTESIAN_POINT ( 'NONE',  ( -2.229437847141422679, 24.50739181907689712, 13.00000000000000178 ) ) ;
#383 = DIRECTION ( 'NONE',  ( 0.000000000000000000, 0.000000000000000000, 1.000000000000000000 ) ) ;
#384 = CARTESIAN_POINT ( 'NONE',  ( 8.496730143421112658, 19.88634191853696720, -24.66085836945053700 ) ) ;
#385 = EDGE_LOOP ( 'NONE', ( #29056, #12887, #37064, #5355 ) ) ;
#386 = CARTESIAN_POINT ( 'NONE',  ( -20.41576651639842765, 13.46337821832906201, -9.393711450338390279 ) ) ;
#387 = CARTESIAN_POINT ( 'NONE',  ( -8.437494165185018602, 40.76200631401457031, 11.00000000000000000 ) ) ;
#388 = CARTESIAN_POINT ( 'NONE',  ( 9.606819337878498288, -18.10969338424137831, -30.00000000000000000 ) ) ;
#389 = CARTESIAN_POINT ( 'NONE',  ( 4.118671991557230072, 37.17221401100731981, 13.00000000000000178 ) ) ;
#390 = CARTESIAN_POINT ( 'NONE',  ( 12.61335593425192769, 21.11317950107521568, -18.44339444917419613 ) ) ;
#391 = CARTESIAN_POINT ( 'NONE',  ( 20.90924525106827758, -8.502318254486461058, -30.00000000000001421 ) ) ;
#392 = ADVANCED_FACE ( 'NONE', ( #10459 ), #7403, .F. ) ;
#393 = FACE_OUTER_BOUND ( 'NONE', #10195, .T. ) ;
#394 = CARTESIAN_POINT ( 'NONE',  ( -27.04961384508420608, -25.34883885810744886, -5.000000000000005329 ) ) ;
#395 = CARTESIAN_POINT ( 'NONE',  ( 12.91994108110150208, -25.87706059209097731, -7.842292722746678990 ) ) ;
#396 = CARTESIAN_POINT ( 'NONE',  ( 11.37508884758295657, 17.98716365035634368, -25.02329199648203328 ) ) ;
#397 = CARTESIAN_POINT ( 'NONE',  ( 23.48339511270637914, -16.96163556805249684, -16.64869766514032889 ) ) ;
#398 = CARTESIAN_POINT ( 'NONE',  ( 14.08246327825360389, 27.69965426814068366, 10.49999999999999822 ) ) ;
#399 = DIRECTION ( 'NONE',  ( -0.000000000000000000, -0.000000000000000000, -1.000000000000000000 ) ) ;
#400 = VERTEX_POINT ( 'NONE', #31792 ) ;
#401 = CARTESIAN_POINT ( 'NONE',  ( -8.576574787394006805, 28.66784900714714723, -14.90473514947470157 ) ) ;
#402 = AXIS2_PLACEMENT_3D ( 'NONE', #36373, #21524, #8537 ) ;
#403 = CARTESIAN_POINT ( 'NONE',  ( -15.48853126089653642, -26.74269726827072446, -4.999999999999999112 ) ) ;
#404 = CARTESIAN_POINT ( 'NONE',  ( -4.458872323573595864, 26.51478363815348160, 13.00000000000000178 ) ) ;
#405 = AXIS2_PLACEMENT_3D ( 'NONE', #5623, #2190, #9079 ) ;
#406 = VECTOR ( 'NONE', #32320, 1000.000000000000000 ) ;
#407 = DIRECTION ( 'NONE',  ( 1.000000000000000000, 0.000000000000000000, 0.000000000000000000 ) ) ;
#408 = ORIENTED_EDGE ( 'NONE', *, *, #8409, .F. ) ;
#409 = CARTESIAN_POINT ( 'NONE',  ( 26.48649879351080472, 0.3041964394036508201, -15.45264338181639019 ) ) ;
#410 = CARTESIAN_POINT ( 'NONE',  ( -13.13581098909220302, 27.45627467658446008, 11.00000000000000000 ) ) ;
#411 = CIRCLE ( 'NONE', #35441, 18.00000000000000000 ) ;
#412 = DIRECTION ( 'NONE',  ( 0.000000000000000000, 0.000000000000000000, 1.000000000000000000 ) ) ;
#413 = ORIENTED_EDGE ( 'NONE', *, *, #8934, .F. ) ;
#414 = CARTESIAN_POINT ( 'NONE',  ( -21.70419570142134802, 0.7541476106288704795, -23.85713393182268049 ) ) ;
#415 = CARTESIAN_POINT ( 'NONE',  ( -20.01115660715129962, -26.54103525642217321, -8.595240659906115965 ) ) ;
#416 = ORIENTED_EDGE ( 'NONE', *, *, #27931, .F. ) ;
#417 = CARTESIAN_POINT ( 'NONE',  ( 20.40443380874665991, -3.526399787616441461, -27.86714167302821821 ) ) ;
#418 = ORIENTED_EDGE ( 'NONE', *, *, #17489, .F. ) ;
#419 = CARTESIAN_POINT ( 'NONE',  ( 14.61820604905140897, 32.41591307681830614, 13.32518128616609765 ) ) ;
#420 = DIRECTION ( 'NONE',  ( 0.000000000000000000, 0.000000000000000000, 1.000000000000000000 ) ) ;
#421 = CARTESIAN_POINT ( 'NONE',  ( -7.330077540933487512, 17.71145523154927659, 6.000000000000000000 ) ) ;
#422 = ADVANCED_FACE ( 'NONE', ( #9860 ), #3755, .F. ) ;
#423 = CARTESIAN_POINT ( 'NONE',  ( 11.83264664767333052, 25.78892025138632604, 19.27171037444156454 ) ) ;
#424 = CARTESIAN_POINT ( 'NONE',  ( -19.48557158514988785, -11.24999999999987743, 10.00000000000000000 ) ) ;
#425 = ORIENTED_EDGE ( 'NONE', *, *, #25457, .F. ) ;
#426 = CYLINDRICAL_SURFACE ( 'NONE', #11880, 1.000000000000000000 ) ;
#427 = CARTESIAN_POINT ( 'NONE',  ( -20.50991189059329400, -0.1799011681176667099, -29.99999999999999645 ) ) ;
#428 = CARTESIAN_POINT ( 'NONE',  ( 4.100636323082810009, 29.29593658752792962, 12.00000000000000000 ) ) ;
#429 = DIRECTION ( 'NONE',  ( -0.8090169943749504489, -0.5877852522924690293, 0.000000000000000000 ) ) ;
#430 = CARTESIAN_POINT ( 'NONE',  ( 16.64822277588917032, 18.43813335370595752, -13.76538777124787494 ) ) ;
#431 = CARTESIAN_POINT ( 'NONE',  ( 5.310336667938341471, 20.67330757391770035, -25.72323559496285128 ) ) ;
#432 = AXIS2_PLACEMENT_3D ( 'NONE', #3780, #28967, #7629 ) ;
#433 = AXIS2_PLACEMENT_3D ( 'NONE', #15536, #27920, #20843 ) ;
#434 = CARTESIAN_POINT ( 'NONE',  ( 15.14142468963127897, -22.46172105866550339, -16.19430842129408177 ) ) ;
#435 = CARTESIAN_POINT ( 'NONE',  ( 14.98890121934557129, -28.67928442654206833, 11.55979286843934517 ) ) ;
#436 = DIRECTION ( 'NONE',  ( 1.000000000000000000, 0.000000000000000000, 0.000000000000000000 ) ) ;
#437 = EDGE_CURVE ( 'NONE', #21611, #37532, #717, .T. ) ;
#438 = ORIENTED_EDGE ( 'NONE', *, *, #8735, .T. ) ;
#439 = CARTESIAN_POINT ( 'NONE',  ( -11.15269954372922356, 17.20160742699127709, -29.99999999999999645 ) ) ;
#440 = CARTESIAN_POINT ( 'NONE',  ( -29.75773323547239002, -22.90830468393550845, 16.87380292611442201 ) ) ;
#441 = CARTESIAN_POINT ( 'NONE',  ( 12.06224686842067406, -22.02997600949163015, -17.45733707754455821 ) ) ;
#442 = EDGE_CURVE ( 'NONE', #4338, #959, #22639, .T. ) ;
#443 = FACE_OUTER_BOUND ( 'NONE', #7900, .T. ) ;
#444 = EDGE_LOOP ( 'NONE', ( #34440, #26778, #20838, #31828 ) ) ;
#445 = VERTEX_POINT ( 'NONE', #22048 ) ;
#446 = CARTESIAN_POINT ( 'NONE',  ( -9.540218894060958021, 18.45143627731958347, -27.33005333713524720 ) ) ;
#447 = CARTESIAN_POINT ( 'NONE',  ( -11.69803459526607625, -17.05285100544052312, -27.95431881375518657 ) ) ;
#448 = CARTESIAN_POINT ( 'NONE',  ( -10.09822582592840767, -27.41751403068705883, 11.00000000001392308 ) ) ;
#449 = ORIENTED_EDGE ( 'NONE', *, *, #1153, .F. ) ;
#450 = EDGE_CURVE ( 'NONE', #13434, #36251, #32021, .T. ) ;
#451 = CARTESIAN_POINT ( 'NONE',  ( -30.99736797329587290, -9.614891179495492324, -12.97104570887609931 ) ) ;
#452 = CARTESIAN_POINT ( 'NONE',  ( -12.89014915853426224, -23.08559641726087719, -15.45851670612495887 ) ) ;
#453 = DIRECTION ( 'NONE',  ( 1.000000000000000000, 0.000000000000000000, 0.000000000000000000 ) ) ;
#454 = ORIENTED_EDGE ( 'NONE', *, *, #7492, .F. ) ;
#455 = CARTESIAN_POINT ( 'NONE',  ( 29.37184732250830521, 0.3033203897905300539, -10.18640792684451846 ) ) ;
#456 = LINE ( 'NONE', #12243, #18704 ) ;
#457 = DIRECTION ( 'NONE',  ( 0.000000000000000000, 0.000000000000000000, 1.000000000000000000 ) ) ;
#458 = EDGE_LOOP ( 'NONE', ( #11462, #15497, #1605 ) ) ;
#459 = CARTESIAN_POINT ( 'NONE',  ( -30.88976141255646368, -0.06313707789208813925, -5.945739447080108597 ) ) ;
#460 = ORIENTED_EDGE ( 'NONE', *, *, #3040, .F. ) ;
#461 = CARTESIAN_POINT ( 'NONE',  ( 20.74532546937688338, -0.6322448352572834773, -27.35194312868669186 ) ) ;
#462 = AXIS2_PLACEMENT_3D ( 'NONE', #19631, #7640, #26540 ) ;
#463 = CARTESIAN_POINT ( 'NONE',  ( -5.359815401306925686, -19.79953048918116565, -30.00000000000000000 ) ) ;
#464 = CARTESIAN_POINT ( 'NONE',  ( 32.73576105632422184, -2.961849131989182204, 16.87380292611480215 ) ) ;
#465 = ORIENTED_EDGE ( 'NONE', *, *, #21335, .F. ) ;
#466 = EDGE_CURVE ( 'NONE', #7227, #12151, #39815, .T. ) ;
#467 = CARTESIAN_POINT ( 'NONE',  ( -14.63635198741550347, 25.78286467897752487, 7.000000000000000000 ) ) ;
#468 = EDGE_CURVE ( 'NONE', #11093, #7792, #39183, .T. ) ;
#469 = CARTESIAN_POINT ( 'NONE',  ( -4.672335726382759624, 24.36080358023105674, 20.99999999999999645 ) ) ;
#470 = VECTOR ( 'NONE', #7205, 1000.000000000000000 ) ;
#471 = LINE ( 'NONE', #3906, #36294 ) ;
#472 = CYLINDRICAL_SURFACE ( 'NONE', #19490, 1.000000000000000888 ) ;
#473 = FACE_BOUND ( 'NONE', #25651, .T. ) ;
#474 = DIRECTION ( 'NONE',  ( 1.000000000000000000, 0.000000000000000000, 0.000000000000000000 ) ) ;
#475 = CARTESIAN_POINT ( 'NONE',  ( -19.72218505466810967, 7.980765556227030544, -23.29036116115986133 ) ) ;
#476 = CARTESIAN_POINT ( 'NONE',  ( 22.61779009251464956, -26.31551665274535523, -8.089115201911514674 ) ) ;
#477 = CARTESIAN_POINT ( 'NONE',  ( -14.44277748876676881, 26.55045409923033972, 7.499999999999993783 ) ) ;
#478 = ADVANCED_FACE ( 'NONE', ( #13295 ), #25691, .F. ) ;
#479 = CARTESIAN_POINT ( 'NONE',  ( 10.88003517233900297, 17.37455259072008573, -30.00000000000000000 ) ) ;
#480 = VECTOR ( 'NONE', #651, 1000.000000000000114 ) ;
#481 = VERTEX_POINT ( 'NONE', #34449 ) ;
#483 = AXIS2_PLACEMENT_3D ( 'NONE', #20290, #35930, #32279 ) ;
#482 = CARTESIAN_POINT ( 'NONE',  ( -14.02863424743453891, 20.80391705836231608, -16.56546359749882669 ) ) ;
#484 = CARTESIAN_POINT ( 'NONE',  ( -26.84751477640364214, -17.98144108585655232, 20.25080042701566896 ) ) ;
#485 = EDGE_CURVE ( 'NONE', #2217, #31250, #21009, .T. ) ;
#486 = CARTESIAN_POINT ( 'NONE',  ( 10.51560177358059534, 33.07492339674065818, 10.49999999999999822 ) ) ;
#487 = CARTESIAN_POINT ( 'NONE',  ( 11.04029860655090012, 17.32608448718281480, -28.70838011759155961 ) ) ;
#488 = VERTEX_POINT ( 'NONE', #16768 ) ;
#489 = DIRECTION ( 'NONE',  ( 0.000000000000000000, 0.000000000000000000, 1.000000000000000000 ) ) ;
#490 = VERTEX_POINT ( 'NONE', #28941 ) ;
#491 = VECTOR ( 'NONE', #25478, 1000.000000000000000 ) ;
#493 = DIRECTION ( 'NONE',  ( 0.7431448254773954654, 0.6691306063588569053, -0.000000000000000000 ) ) ;
#492 = CARTESIAN_POINT ( 'NONE',  ( -11.33960866872714135, 18.56140262423198450, -23.83101412075703252 ) ) ;
#494 = CARTESIAN_POINT ( 'NONE',  ( -14.24405758500416930, -24.64403535565174508, -12.53474328698910334 ) ) ;
#495 = DIRECTION ( 'NONE',  ( 0.000000000000000000, 0.000000000000000000, 1.000000000000000000 ) ) ;
#496 = AXIS2_PLACEMENT_3D ( 'NONE', #14949, #12490, #18205 ) ;
#497 = ORIENTED_EDGE ( 'NONE', *, *, #4457, .F. ) ;
#498 = CARTESIAN_POINT ( 'NONE',  ( -33.71791919605428944, -15.10493296938091845, -8.852922798908716473 ) ) ;
#499 = CARTESIAN_POINT ( 'NONE',  ( -9.692485564073882287, -19.34668444509729568, -23.91709408057471364 ) ) ;
#500 = DIRECTION ( 'NONE',  ( 0.000000000000000000, 0.000000000000000000, 1.000000000000000000 ) ) ;
#501 = CARTESIAN_POINT ( 'NONE',  ( 13.86637344848912257, 19.30070053511032668, -18.64709189320727489 ) ) ;
#502 = ORIENTED_EDGE ( 'NONE', *, *, #14245, .T. ) ;
#503 = CARTESIAN_POINT ( 'NONE',  ( 26.00311425638208362, 4.651086067102406574, -9.804938788202040456 ) ) ;
#504 = CARTESIAN_POINT ( 'NONE',  ( -3.597409820281606940, 14.42008525284352594, 9.000000000000001776 ) ) ;
#505 = DIRECTION ( 'NONE',  ( -0.5877852522924796874, -0.8090169943749425663, 0.000000000000000000 ) ) ;
#506 = CARTESIAN_POINT ( 'NONE',  ( -9.221287281574667816, 10.65863771052209863, 7.000000000000000000 ) ) ;
#507 = ORIENTED_EDGE ( 'NONE', *, *, #21085, .T. ) ;
#508 = CARTESIAN_POINT ( 'NONE',  ( -22.38012257604306399, -0.01397392160533758761, -22.64776935873009123 ) ) ;
#509 = CARTESIAN_POINT ( 'NONE',  ( 21.73684131651624796, 0.5819632018348794844, -23.83618332979514776 ) ) ;
#510 = CARTESIAN_POINT ( 'NONE',  ( 26.56332897235214574, -4.302820985782148000, 20.25080042701566541 ) ) ;
#511 = ORIENTED_EDGE ( 'NONE', *, *, #1102, .F. ) ;
#512 = VECTOR ( 'NONE', #22352, 1000.000000000000000 ) ;
#513 = CARTESIAN_POINT ( 'NONE',  ( 12.33616729053617966, -27.99489201236593416, -13.58461195433497437 ) ) ;
#514 = CARTESIAN_POINT ( 'NONE',  ( 14.36830325120613594, 20.48707633493483371, 9.000000000000001776 ) ) ;
#515 = AXIS2_PLACEMENT_3D ( 'NONE', #19842, #29379, #10491 ) ;
#516 = ORIENTED_EDGE ( 'NONE', *, *, #20080, .F. ) ;
#517 = ADVANCED_FACE ( 'NONE', ( #1121 ), #13502, .T. ) ;
#518 = CARTESIAN_POINT ( 'NONE',  ( 14.52509594610761923, 21.97885917798724975, 7.500000000000010658 ) ) ;
#519 = VECTOR ( 'NONE', #30356, 999.9999999999998863 ) ;
#520 = CARTESIAN_POINT ( 'NONE',  ( -11.61146752755215417, 31.78078372435996002, 10.49999999999999822 ) ) ;
#521 = DIRECTION ( 'NONE',  ( -0.000000000000000000, -0.000000000000000000, -1.000000000000000000 ) ) ;
#522 = CARTESIAN_POINT ( 'NONE',  ( 2.722378455267432606, 20.72894175598409205, -26.99545394230949924 ) ) ;
#523 = LINE ( 'NONE', #12905, #3587 ) ;
#524 = CARTESIAN_POINT ( 'NONE',  ( 14.55889214498799689, 20.02072497456981282, 10.49999999999999822 ) ) ;
#525 = DIRECTION ( 'NONE',  ( 1.000000000000000000, 0.000000000000000000, 0.000000000000000000 ) ) ;
#526 = CARTESIAN_POINT ( 'NONE',  ( -14.81329996725647469, 19.93755115561707569, 11.00000000000000000 ) ) ;
#527 = CARTESIAN_POINT ( 'NONE',  ( -14.25384497784211923, 25.55416164399415280, 7.000000000000000000 ) ) ;
#528 = CARTESIAN_POINT ( 'NONE',  ( -6.688306800005769048, 28.52217545723006609, 12.00000000000000000 ) ) ;
#529 = CARTESIAN_POINT ( 'NONE',  ( 14.90937338384046207, 27.40770937021949294, -7.795567658461852290 ) ) ;
#530 = DIRECTION ( 'NONE',  ( 0.000000000000000000, 0.000000000000000000, -1.000000000000000000 ) ) ;
#531 = ORIENTED_EDGE ( 'NONE', *, *, #18718, .T. ) ;
#533 = CARTESIAN_POINT ( 'NONE',  ( 2.046188276595768407, 8.063706679521116527, 10.49999999999999822 ) ) ;
#532 = CARTESIAN_POINT ( 'NONE',  ( -17.91418368663225635, 16.64594202802076595, -12.82604463341725598 ) ) ;
#534 = DIRECTION ( 'NONE',  ( -0.000000000000000000, -0.000000000000000000, -1.000000000000000000 ) ) ;
#535 = CARTESIAN_POINT ( 'NONE',  ( 11.53193418976769102, -20.97837345754841820, -19.49836150433041837 ) ) ;
#536 = CYLINDRICAL_SURFACE ( 'NONE', #23712, 1.000000000000000888 ) ;
#537 = CARTESIAN_POINT ( 'NONE',  ( 15.17870064116790374, 26.26746426438345594, -8.297842380696128117 ) ) ;
#538 = CARTESIAN_POINT ( 'NONE',  ( 14.73308801456976980, 25.40969082412797420, -10.65228738806455766 ) ) ;
#539 = ORIENTED_EDGE ( 'NONE', *, *, #1715, .F. ) ;
#540 = DIRECTION ( 'NONE',  ( -0.000000000000000000, -0.000000000000000000, -1.000000000000000000 ) ) ;
#541 = CARTESIAN_POINT ( 'NONE',  ( -9.556882383769263356, -18.37204861498985053, -27.45237673257718924 ) ) ;
#542 = CARTESIAN_POINT ( 'NONE',  ( -37.14493776307941175, -9.008680429016052926, 12.73282698324853079 ) ) ;
#543 = AXIS2_PLACEMENT_3D ( 'NONE', #36741, #6444, #8906 ) ;
#544 = TOROIDAL_SURFACE ( 'NONE', #21940, 1.000000000000000000, 0.5000000000000000000 ) ;
#545 = CARTESIAN_POINT ( 'NONE',  ( -26.76216378966945086, -19.72671915244844953, -12.90723624995964691 ) ) ;
#546 = CARTESIAN_POINT ( 'NONE',  ( -4.347975343347115995, -23.51214084136499594, -13.86639182548506533 ) ) ;
#547 = CARTESIAN_POINT ( 'NONE',  ( 15.43728935786161216, 25.42686383105192860, -8.304351359789887255 ) ) ;
#548 = ORIENTED_EDGE ( 'NONE', *, *, #9154, .F. ) ;
#549 = CARTESIAN_POINT ( 'NONE',  ( 21.75928845812402557, 9.796106908765645827, -12.87849264206665190 ) ) ;
#550 = CARTESIAN_POINT ( 'NONE',  ( 5.767236651883445475, 13.71142893291679243, 10.50000000000000000 ) ) ;
#551 = CARTESIAN_POINT ( 'NONE',  ( 9.401525468405049324, 34.87112330957724282, 16.87380292611441490 ) ) ;
#552 = AXIS2_PLACEMENT_3D ( 'NONE', #26299, #39088, #32608 ) ;
#553 = ORIENTED_EDGE ( 'NONE', *, *, #25998, .T. ) ;
#554 = CARTESIAN_POINT ( 'NONE',  ( -32.67788646804365271, -3.365289809214419670, -8.615938099305980202 ) ) ;
#555 = AXIS2_PLACEMENT_3D ( 'NONE', #755, #4607, #4402 ) ;
#556 = CARTESIAN_POINT ( 'NONE',  ( -26.46356280842828212, 3.031871643958657714, 17.42190598798967827 ) ) ;
#557 = ORIENTED_EDGE ( 'NONE', *, *, #30997, .F. ) ;
#558 = CARTESIAN_POINT ( 'NONE',  ( 21.42047163595253778, -15.86044052053649978, 20.99999999999999645 ) ) ;
#559 = CARTESIAN_POINT ( 'NONE',  ( 14.81329996725643738, 19.93755115561686964, 11.00000000000000000 ) ) ;
#560 = CARTESIAN_POINT ( 'NONE',  ( -29.88325193432147842, 0.8555504981620180027, -6.890743476730220252 ) ) ;
#561 = CARTESIAN_POINT ( 'NONE',  ( 29.51672614961463736, -12.91057139293011602, -13.82673195968690649 ) ) ;
#562 = CARTESIAN_POINT ( 'NONE',  ( 34.54872031832756818, -1.828101745486344187, 13.32518128616626640 ) ) ;
#563 = ADVANCED_FACE ( 'NONE', ( #26303 ), #20819, .T. ) ;
#564 = ORIENTED_EDGE ( 'NONE', *, *, #28279, .T. ) ;
#565 = ORIENTED_EDGE ( 'NONE', *, *, #1592, .F. ) ;
#566 = DIRECTION ( 'NONE',  ( 1.000000000000000000, 0.000000000000000000, 0.000000000000000000 ) ) ;
#567 = DIRECTION ( 'NONE',  ( 0.000000000000000000, 0.000000000000000000, 1.000000000000000000 ) ) ;
#568 = AXIS2_PLACEMENT_3D ( 'NONE', #19540, #31929, #16503 ) ;
#569 = CYLINDRICAL_SURFACE ( 'NONE', #4551, 1.000000000000000000 ) ;
#570 = ORIENTED_EDGE ( 'NONE', *, *, #16751, .F. ) ;
#571 = EDGE_CURVE ( 'NONE', #36570, #10398, #25541, .T. ) ;
#572 = CARTESIAN_POINT ( 'NONE',  ( -1.887696780556682219, 23.64799547898650189, -21.85798975256318855 ) ) ;
#573 = CARTESIAN_POINT ( 'NONE',  ( -35.07906678349440455, -7.111640533861553592, -4.999999999999999112 ) ) ;
#574 = CARTESIAN_POINT ( 'NONE',  ( -15.00000000000000000, 22.50000000000000355, 0.000000000000000000 ) ) ;
#575 = EDGE_CURVE ( 'NONE', #17675, #5736, #23614, .T. ) ;
#576 = AXIS2_PLACEMENT_3D ( 'NONE', #4517, #7758, #23405 ) ;
#577 = LINE ( 'NONE', #40192, #36421 ) ;
#578 = CARTESIAN_POINT ( 'NONE',  ( 7.282669157963869822, 29.73016112791698262, 10.75000000000000000 ) ) ;
#579 = CARTESIAN_POINT ( 'NONE',  ( 4.100636323082810009, 29.29593658752792962, 12.00000000000000000 ) ) ;
#580 = CARTESIAN_POINT ( 'NONE',  ( 13.04798778810585347, 29.04188371427077087, -10.44273296311215304 ) ) ;
#581 = EDGE_LOOP ( 'NONE', ( #27282, #21112 ) ) ;
#582 = CARTESIAN_POINT ( 'NONE',  ( -21.00653608580854481, 12.56855149973239172, -8.901572196327759201 ) ) ;
#583 = DIRECTION ( 'NONE',  ( 0.000000000000000000, 0.000000000000000000, 1.000000000000000000 ) ) ;
#584 = CARTESIAN_POINT ( 'NONE',  ( 10.31172964540912673, -19.13411530003786964, -23.84291266785244545 ) ) ;
#585 = PLANE ( 'NONE',  #20443 ) ;
#586 = CARTESIAN_POINT ( 'NONE',  ( 15.26830110528803530, 26.60668572641256802, -7.355644065423295075 ) ) ;
#587 = CARTESIAN_POINT ( 'NONE',  ( 37.62663912510992503, -8.659558992827971480, -14.26382729546509687 ) ) ;
#588 = PLANE ( 'NONE',  #3155 ) ;
#589 = CARTESIAN_POINT ( 'NONE',  ( -25.85745970633643864, -25.73337701278340006, -6.737025561790457751 ) ) ;
#590 = CARTESIAN_POINT ( 'NONE',  ( 8.302662708387121171, -24.93668839658822023, -8.846291834586214264 ) ) ;
#591 = CARTESIAN_POINT ( 'NONE',  ( 15.08502492231579595, 25.75735284694121319, -9.240969017626685655 ) ) ;
#592 = CARTESIAN_POINT ( 'NONE',  ( 18.23446778745489638, -12.32129691478622213, -24.23299356642612423 ) ) ;
#593 = EDGE_CURVE ( 'NONE', #38427, #25178, #1550, .T. ) ;
#594 = CARTESIAN_POINT ( 'NONE',  ( 13.72389693702425184, 27.48489553602867019, 10.99387789255783687 ) ) ;
#595 = DIRECTION ( 'NONE',  ( -0.000000000000000000, -0.000000000000000000, 1.000000000000000000 ) ) ;
#596 = ADVANCED_FACE ( 'NONE', ( #10870 ), #32410, .F. ) ;
#597 = ORIENTED_EDGE ( 'NONE', *, *, #23075, .F. ) ;
#598 = CARTESIAN_POINT ( 'NONE',  ( -8.428619364643951783, 35.98800784865809277, -6.299206775149388982 ) ) ;
#599 = CARTESIAN_POINT ( 'NONE',  ( 2.256323172317815207, 14.28970123917151192, 9.000000000000001776 ) ) ;
#600 = VECTOR ( 'NONE', #21084, 1000.000000000000000 ) ;
#601 = CIRCLE ( 'NONE', #23310, 1.000000000000000888 ) ;
#602 = FACE_OUTER_BOUND ( 'NONE', #27008, .T. ) ;
#603 = EDGE_LOOP ( 'NONE', ( #23347, #6480, #32826, #34211 ) ) ;
#604 = CARTESIAN_POINT ( 'NONE',  ( 28.92463652500844162, 0.06159917911152616721, -11.59545931083614079 ) ) ;
#605 = DIRECTION ( 'NONE',  ( 0.000000000000000000, 0.000000000000000000, 1.000000000000000000 ) ) ;
#606 = FACE_OUTER_BOUND ( 'NONE', #33987, .T. ) ;
#607 = CIRCLE ( 'NONE', #22659, 16.00000000000000000 ) ;
#608 = B_SPLINE_SURFACE_WITH_KNOTS ( 'NONE', 1, 3, ( 
 ( #8281, #20688, #33083, #17647, #29414, #30019, #1791, #10525, #2195, #7469 ),
 ( #32265, #16834, #29215, #30431, #11932, #11734, #27366, #2393, #27566, #11535 ) ),
 .UNSPECIFIED., .F., .F., .F.,
 ( 2, 2 ),
 ( 4, 2, 2, 2, 4 ),
 ( 0.000000000000000000, 1.000000000000000000 ),
 ( -1.344962617103292679, -0.9522635354045664302, -0.5595644537058401813, -0.1668653720071138769, 0.2258337096916124276 ),
 .UNSPECIFIED. ) ;
#609 = ORIENTED_EDGE ( 'NONE', *, *, #7426, .F. ) ;
#610 = CARTESIAN_POINT ( 'NONE',  ( -30.44556900789973852, 0.02942595176201418319, -7.828065574714944574 ) ) ;
#611 = DIRECTION ( 'NONE',  ( 0.000000000000000000, -0.000000000000000000, -1.000000000000000000 ) ) ;
#612 = ORIENTED_EDGE ( 'NONE', *, *, #30344, .T. ) ;
#613 = CARTESIAN_POINT ( 'NONE',  ( 31.36889017270395286, -5.558195913421866585, -12.17070191464305751 ) ) ;
#614 = VERTEX_POINT ( 'NONE', #20214 ) ;
#615 = CARTESIAN_POINT ( 'NONE',  ( -7.591957726968746378, 38.93640765974107154, 10.99999999999981526 ) ) ;
#616 = CARTESIAN_POINT ( 'NONE',  ( -13.94482798346716201, 26.50521816028930999, 7.000000000000000000 ) ) ;
#617 = CARTESIAN_POINT ( 'NONE',  ( 5.947717410344609767, 34.62949535663720013, 7.000000000000000000 ) ) ;
#618 = EDGE_CURVE ( 'NONE', #36861, #8408, #24252, .T. ) ;
#619 = CARTESIAN_POINT ( 'NONE',  ( 4.864422697791962236, 33.03032433378086807, 19.66345542862529427 ) ) ;
#620 = DIRECTION ( 'NONE',  ( 0.000000000000000000, 0.000000000000000000, 1.000000000000000000 ) ) ;
#621 = EDGE_LOOP ( 'NONE', ( #17162, #4935, #36145, #2379, #27346, #12203, #28190 ) ) ;
#622 = DIRECTION ( 'NONE',  ( 0.000000000000000000, 0.000000000000000000, 1.000000000000000000 ) ) ;
#623 = CARTESIAN_POINT ( 'NONE',  ( -13.94509305167025204, 15.04106830562277253, -30.00000000000002132 ) ) ;
#624 = DIRECTION ( 'NONE',  ( 1.000000000000000000, 0.000000000000000000, 0.000000000000000000 ) ) ;
#625 = CARTESIAN_POINT ( 'NONE',  ( 8.577540944421576441, 33.15743037285414374, 6.000000000000000000 ) ) ;
#626 = CARTESIAN_POINT ( 'NONE',  ( 14.98739814520312130, 15.86604096426238364, -22.05070079658612059 ) ) ;
#628 = AXIS2_PLACEMENT_3D ( 'NONE', #36059, #24064, #26910 ) ;
#627 = CARTESIAN_POINT ( 'NONE',  ( 4.580011667354150440, 20.37550453228363878, -27.05156434026686441 ) ) ;
#629 = ORIENTED_EDGE ( 'NONE', *, *, #20742, .F. ) ;
#630 = CARTESIAN_POINT ( 'NONE',  ( 10.08241157172804670, -17.84938614438609505, -30.00000000000000000 ) ) ;
#631 = DIRECTION ( 'NONE',  ( 0.000000000000000000, 0.000000000000000000, -1.000000000000000000 ) ) ;
#632 = VECTOR ( 'NONE', #12558, 1000.000000000000000 ) ;
#633 = DIRECTION ( 'NONE',  ( 0.000000000000000000, 0.000000000000000000, 1.000000000000000000 ) ) ;
#634 = VERTEX_POINT ( 'NONE', #17175 ) ;
#635 = CARTESIAN_POINT ( 'NONE',  ( -11.01210778500241361, 17.34425618060466689, -28.70720727591743682 ) ) ;
#636 = CARTESIAN_POINT ( 'NONE',  ( -32.97049335004036408, -4.716631976066113729, 17.42190598798392998 ) ) ;
#637 = CARTESIAN_POINT ( 'NONE',  ( 9.889788205164110835, -18.84469253480084205, -25.02328945438690866 ) ) ;
#638 = DIRECTION ( 'NONE',  ( 0.000000000000000000, 0.000000000000000000, 1.000000000000000000 ) ) ;
#639 = EDGE_CURVE ( 'NONE', #11613, #16948, #14507, .T. ) ;
#640 = ORIENTED_EDGE ( 'NONE', *, *, #14841, .F. ) ;
#641 = ORIENTED_EDGE ( 'NONE', *, *, #9085, .F. ) ;
#642 = CARTESIAN_POINT ( 'NONE',  ( -8.669908543505703946, 19.79285976321129681, -24.67981830963679357 ) ) ;
#643 = DIRECTION ( 'NONE',  ( 0.3090169943749573322, 0.9510565162951504226, -0.000000000000000000 ) ) ;
#644 = FACE_BOUND ( 'NONE', #39612, .T. ) ;
#645 = CARTESIAN_POINT ( 'NONE',  ( -35.42614648568259383, -9.922089300916915988, -5.873467316378663483 ) ) ;
#646 = CARTESIAN_POINT ( 'NONE',  ( -13.57768790248920254, -24.10155420078447719, -13.51926864417577079 ) ) ;
#647 = FACE_OUTER_BOUND ( 'NONE', #36295, .T. ) ;
#648 = VERTEX_POINT ( 'NONE', #32814 ) ;
#649 = CARTESIAN_POINT ( 'NONE',  ( 24.49786104224794769, 0.5606131564536942502, -18.46619948923875754 ) ) ;
#650 = CARTESIAN_POINT ( 'NONE',  ( 5.064564986133971658, 13.54338174056915456, 6.000000000000000000 ) ) ;
#651 = DIRECTION ( 'NONE',  ( -0.3535533905932792820, -0.6123724356957955806, -0.7071067811865437980 ) ) ;
#652 = ORIENTED_EDGE ( 'NONE', *, *, #37876, .T. ) ;
#653 = CARTESIAN_POINT ( 'NONE',  ( -30.66481745429630834, -0.06869490606624445439, -7.356079483744078829 ) ) ;
#654 = ORIENTED_EDGE ( 'NONE', *, *, #20863, .T. ) ;
#655 = CARTESIAN_POINT ( 'NONE',  ( 31.43862993417205587, -1.740267522059486760, -9.139700976824004286 ) ) ;
#656 = AXIS2_PLACEMENT_3D ( 'NONE', #39004, #20734, #38601 ) ;
#657 = CYLINDRICAL_SURFACE ( 'NONE', #27165, 1.000000000000000888 ) ;
#658 = CARTESIAN_POINT ( 'NONE',  ( 28.76760616113913827, -24.40467509901337451, 16.30093088680155233 ) ) ;
#659 = VERTEX_POINT ( 'NONE', #11273 ) ;
#660 = AXIS2_PLACEMENT_3D ( 'NONE', #1120, #13501, #15263 ) ;
#661 = DIRECTION ( 'NONE',  ( -0.000000000000000000, -0.000000000000000000, -1.000000000000000000 ) ) ;
#662 = EDGE_CURVE ( 'NONE', #39411, #25405, #239, .T. ) ;
#663 = CARTESIAN_POINT ( 'NONE',  ( 0.6269669233416744758, 28.28960257232503395, 20.99999999999998934 ) ) ;
#664 = CARTESIAN_POINT ( 'NONE',  ( 5.706335727061685681, 24.35410196624994583, 13.00000000000000178 ) ) ;
#665 = EDGE_CURVE ( 'NONE', #36376, #19095, #908, .T. ) ;
#666 = FACE_OUTER_BOUND ( 'NONE', #37210, .T. ) ;
#667 = VECTOR ( 'NONE', #4209, 1000.000000000000000 ) ;
#668 = EDGE_CURVE ( 'NONE', #29140, #10198, #27105, .T. ) ;
#669 = LINE ( 'NONE', #26655, #35272 ) ;
#670 = CARTESIAN_POINT ( 'NONE',  ( 28.79337657215373980, 4.963436916934907295, 11.55979286843148302 ) ) ;
#671 = CARTESIAN_POINT ( 'NONE',  ( -22.79758257504442653, 9.829873109737514270, -7.912986613509453981 ) ) ;
#672 = CARTESIAN_POINT ( 'NONE',  ( 24.21359695930263101, -26.57684320323437532, -5.000000000000000888 ) ) ;
#673 = CARTESIAN_POINT ( 'NONE',  ( -0.01803903918367114056, 14.62372257652092422, 6.000000000000000000 ) ) ;
#674 = CARTESIAN_POINT ( 'NONE',  ( 14.20562871930490978, 24.69601559057154816, -12.53150451778845564 ) ) ;
#675 = ORIENTED_EDGE ( 'NONE', *, *, #10855, .T. ) ;
#676 = CARTESIAN_POINT ( 'NONE',  ( -13.79767463674636296, 21.20177806324913306, -16.53259672287590831 ) ) ;
#677 = CARTESIAN_POINT ( 'NONE',  ( -23.91569629078610149, -19.26019901638321130, 20.50957957746006954 ) ) ;
#678 = CARTESIAN_POINT ( 'NONE',  ( 10.50986403156584714, 32.63594044384544901, 10.99387789255782977 ) ) ;
#679 = CARTESIAN_POINT ( 'NONE',  ( 11.91825936693510535, 19.35450465693568844, -21.62159660657380300 ) ) ;
#680 = ORIENTED_EDGE ( 'NONE', *, *, #28784, .T. ) ;
#681 = CARTESIAN_POINT ( 'NONE',  ( 18.51255757462615037, -10.21466864353301141, -26.25688464355175711 ) ) ;
#682 = CYLINDRICAL_SURFACE ( 'NONE', #22242, 1.000000000000000000 ) ;
#683 = EDGE_CURVE ( 'NONE', #5931, #35634, #37212, .T. ) ;
#684 = CIRCLE ( 'NONE', #18216, 1.000000000000000000 ) ;
#685 = EDGE_LOOP ( 'NONE', ( #29987, #10385, #3731, #31281 ) ) ;
#687 = CARTESIAN_POINT ( 'NONE',  ( -14.73239529508891188, 21.45431699865994446, 10.94611345180490680 ) ) ;
#686 = CARTESIAN_POINT ( 'NONE',  ( -15.13223720903381420, 26.73911770198351334, -7.816828578819325024 ) ) ;
#688 = EDGE_CURVE ( 'NONE', #13732, #13187, #35450, .T. ) ;
#689 = CARTESIAN_POINT ( 'NONE',  ( -11.68873037371707646, -20.37810347578055215, -20.47508729926761006 ) ) ;
#690 = CARTESIAN_POINT ( 'NONE',  ( 12.69365875748871808, 14.48606190191208043, 10.49999999999999822 ) ) ;
#691 = EDGE_CURVE ( 'NONE', #38413, #8131, #33021, .T. ) ;
#692 = ORIENTED_EDGE ( 'NONE', *, *, #14157, .F. ) ;
#693 = CARTESIAN_POINT ( 'NONE',  ( -34.20107842149033672, -15.32937321432364541, -7.980157440187811702 ) ) ;
#694 = CARTESIAN_POINT ( 'NONE',  ( -14.38923059561778750, -26.28103352123245884, -7.361378720437378398 ) ) ;
#695 = CARTESIAN_POINT ( 'NONE',  ( -3.458872323573595864, 26.51478363815348160, 13.00000000000000178 ) ) ;
#696 = CARTESIAN_POINT ( 'NONE',  ( 13.27244829273280580, 17.32419186230290364, -22.96854396723484371 ) ) ;
#697 = VERTEX_POINT ( 'NONE', #5170 ) ;
#698 = CARTESIAN_POINT ( 'NONE',  ( 25.23600728880220601, 5.524756554899235006, -10.31010501861125483 ) ) ;
#699 = CARTESIAN_POINT ( 'NONE',  ( 6.064564986133971658, 13.54338174056915456, 6.000000000000000000 ) ) ;
#700 = CARTESIAN_POINT ( 'NONE',  ( -13.30736791469135483, 15.68301270237671474, 10.49999999999999822 ) ) ;
#701 = CARTESIAN_POINT ( 'NONE',  ( -10.26940745284057321, 33.04623494220486890, 10.49999999999999822 ) ) ;
#702 = ORIENTED_EDGE ( 'NONE', *, *, #1930, .F. ) ;
#703 = CARTESIAN_POINT ( 'NONE',  ( -26.28050422335599734, -0.3854494769453477576, -16.35547130288665585 ) ) ;
#704 = CARTESIAN_POINT ( 'NONE',  ( 29.81715026116830813, -0.1969218862350708976, -10.16156011328718733 ) ) ;
#705 = AXIS2_PLACEMENT_3D ( 'NONE', #15865, #25, #24803 ) ;
#706 = CARTESIAN_POINT ( 'NONE',  ( 23.63966112704433087, -21.14828014214163687, 19.99202127657103034 ) ) ;
#707 = AXIS2_PLACEMENT_3D ( 'NONE', #29205, #32465, #35505 ) ;
#708 = VERTEX_POINT ( 'NONE', #2331 ) ;
#709 = CARTESIAN_POINT ( 'NONE',  ( 8.937590682902566641, -20.71651963383554218, -30.00000000000000000 ) ) ;
#710 = EDGE_CURVE ( 'NONE', #32625, #13649, #10400, .T. ) ;
#711 = CARTESIAN_POINT ( 'NONE',  ( -3.118678732975735279, 7.827785988993307242, 13.00000000000000178 ) ) ;
#712 = EDGE_CURVE ( 'NONE', #7720, #4426, #23259, .T. ) ;
#713 = ORIENTED_EDGE ( 'NONE', *, *, #38236, .T. ) ;
#714 = AXIS2_PLACEMENT_3D ( 'NONE', #38345, #10515, #35300 ) ;
#715 = DIRECTION ( 'NONE',  ( -0.6691306063588706721, -0.7431448254773830309, -6.938893903907237844E-15 ) ) ;
#716 = CARTESIAN_POINT ( 'NONE',  ( -11.48173768534022976, 32.16538668264431777, 10.49999999999999645 ) ) ;
#717 = LINE ( 'NONE', #3561, #16478 ) ;
#718 = CARTESIAN_POINT ( 'NONE',  ( 2.668841116913946987, 20.33496311051875693, -29.22043024060798544 ) ) ;
#719 = LINE ( 'NONE', #37295, #34101 ) ;
#720 = ORIENTED_EDGE ( 'NONE', *, *, #23187, .T. ) ;
#721 = CARTESIAN_POINT ( 'NONE',  ( -6.431109915229962226, 35.71521269883987770, 10.96580508970282253 ) ) ;
#722 = DIRECTION ( 'NONE',  ( -0.1045284632676566766, -0.9945218953682730678, 0.000000000000000000 ) ) ;
#723 = CARTESIAN_POINT ( 'NONE',  ( 29.12711452743133123, -22.43287856296975136, -8.860495667039732126 ) ) ;
#724 = LINE ( 'NONE', #28551, #470 ) ;
#725 = DIRECTION ( 'NONE',  ( 1.000000000000000000, 1.224646799147351235E-16, -0.000000000000000000 ) ) ;
#726 = LINE ( 'NONE', #37894, #21676 ) ;
#727 = CARTESIAN_POINT ( 'NONE',  ( 10.90121339050992688, 18.34931554698703238, -24.95865895646690902 ) ) ;
#728 = DIRECTION ( 'NONE',  ( 1.000000000000000000, 0.000000000000000000, 0.000000000000000000 ) ) ;
#729 = ORIENTED_EDGE ( 'NONE', *, *, #21810, .F. ) ;
#730 = AXIS2_PLACEMENT_3D ( 'NONE', #39640, #18124, #33167 ) ;
#732 = DIRECTION ( 'NONE',  ( 1.000000000000000000, 0.000000000000000000, 0.000000000000000000 ) ) ;
#731 = CARTESIAN_POINT ( 'NONE',  ( -17.41140981635742691, 20.80174530708337244, -5.476551464811988623 ) ) ;
#733 = CARTESIAN_POINT ( 'NONE',  ( 13.28731253932047807, 15.83618351361437959, 10.49999999999999822 ) ) ;
#734 = CIRCLE ( 'NONE', #27335, 0.5000000000000007772 ) ;
#735 = CARTESIAN_POINT ( 'NONE',  ( 10.20950366300454171, -19.16978685508543023, -23.85584966388176298 ) ) ;
#736 = DIRECTION ( 'NONE',  ( 1.000000000000000000, 0.000000000000000000, 0.000000000000000000 ) ) ;
#737 = CARTESIAN_POINT ( 'NONE',  ( 10.99090272494190224, 17.30462611091308034, -29.34849402232231697 ) ) ;
#738 = ORIENTED_EDGE ( 'NONE', *, *, #6248, .T. ) ;
#739 = CARTESIAN_POINT ( 'NONE',  ( 15.22950456640031014, 26.41560797655204240, -7.827722518576876176 ) ) ;
#740 = ORIENTED_EDGE ( 'NONE', *, *, #36204, .T. ) ;
#741 = CARTESIAN_POINT ( 'NONE',  ( 0.5000000000000005551, 32.50000000000000000, 10.49999999999999645 ) ) ;
#742 = CARTESIAN_POINT ( 'NONE',  ( -9.628986672078191589, -18.46998302835118011, -26.83562301995240773 ) ) ;
#743 = CARTESIAN_POINT ( 'NONE',  ( -37.00900745416922177, -9.025932648522855928, 13.32518128616608699 ) ) ;
#744 = CARTESIAN_POINT ( 'NONE',  ( -31.54076586169206919, -21.75719626739306634, -5.857273151554024615 ) ) ;
#745 = CARTESIAN_POINT ( 'NONE',  ( -4.676031460464607825, -24.51955512654058467, -9.374897136078594428 ) ) ;
#746 = CARTESIAN_POINT ( 'NONE',  ( 11.42286652154374416, 17.26241004482871588, -27.47436460497770838 ) ) ;
#747 = VERTEX_POINT ( 'NONE', #23050 ) ;
#748 = CARTESIAN_POINT ( 'NONE',  ( 18.42271044342168551, 9.437130544017666267, -26.61798538005301751 ) ) ;
#749 = CARTESIAN_POINT ( 'NONE',  ( -8.843266739736657556, 16.81698729810786830, 10.50000000000000000 ) ) ;
#750 = CARTESIAN_POINT ( 'NONE',  ( -3.366772934462026523, 37.76190412503627414, 16.87380292611445043 ) ) ;
#751 = VERTEX_POINT ( 'NONE', #4970 ) ;
#752 = CARTESIAN_POINT ( 'NONE',  ( -33.32611593189657384, -4.382374629824890455, -8.137203135799296660 ) ) ;
#753 = CARTESIAN_POINT ( 'NONE',  ( -23.79662817865075652, 0.8209266586187062842, 19.66345542862912765 ) ) ;
#754 = ORIENTED_EDGE ( 'NONE', *, *, #2123, .T. ) ;
#755 = CARTESIAN_POINT ( 'NONE',  ( -14.26585111513660031, 17.86474508437623143, 13.00000000000000178 ) ) ;
#756 = CARTESIAN_POINT ( 'NONE',  ( 23.05386822411318803, -7.747535282638377652, 23.00000000000000000 ) ) ;
#757 = CARTESIAN_POINT ( 'NONE',  ( -24.93452846701059045, 1.910380023892134904, -16.57983970799203988 ) ) ;
#758 = CARTESIAN_POINT ( 'NONE',  ( 33.76608682364540925, -14.77791854593863441, -8.856012205662965542 ) ) ;
#759 = CARTESIAN_POINT ( 'NONE',  ( 35.99085602461089195, -18.53811353976012555, 12.14047268033102611 ) ) ;
#760 = CIRCLE ( 'NONE', #6572, 1.000000000000007772 ) ;
#761 = VERTEX_POINT ( 'NONE', #35848 ) ;
#762 = ORIENTED_EDGE ( 'NONE', *, *, #20179, .T. ) ;
#763 = DIRECTION ( 'NONE',  ( -1.224646799147353947E-16, 1.000000000000000000, 0.000000000000000000 ) ) ;
#764 = LINE ( 'NONE', #29397, #38958 ) ;
#765 = CARTESIAN_POINT ( 'NONE',  ( 5.440908595777819379, 35.94977745735560859, 11.00000000000000000 ) ) ;
#766 = ORIENTED_EDGE ( 'NONE', *, *, #9500, .T. ) ;
#767 = CARTESIAN_POINT ( 'NONE',  ( -0.5252917279287608876, 26.85053590416535485, -18.61061436390101420 ) ) ;
#768 = CARTESIAN_POINT ( 'NONE',  ( -14.06524961900331760, 27.71236540882611621, 7.499999999999993783 ) ) ;
#769 = CARTESIAN_POINT ( 'NONE',  ( -10.54700836463453584, 22.39697303105802462, 11.00000000000000000 ) ) ;
#770 = AXIS2_PLACEMENT_3D ( 'NONE', #10146, #34727, #6484 ) ;
#771 = FACE_OUTER_BOUND ( 'NONE', #385, .T. ) ;
#772 = DIRECTION ( 'NONE',  ( 1.000000000000000000, 0.000000000000000000, 0.000000000000000000 ) ) ;
#773 = DIRECTION ( 'NONE',  ( -0.07391278520356947546, -0.7032331762534066444, -0.7071067811865447972 ) ) ;
#774 = CARTESIAN_POINT ( 'NONE',  ( 14.48331725184759478, 29.32085274443433676, -5.463096073128409280 ) ) ;
#775 = DIRECTION ( 'NONE',  ( 0.000000000000000000, 0.000000000000000000, 1.000000000000000000 ) ) ;
#776 = ORIENTED_EDGE ( 'NONE', *, *, #24265, .T. ) ;
#778 = DIRECTION ( 'NONE',  ( -0.8660254037844432595, -0.4999999999999920064, 0.000000000000000000 ) ) ;
#777 = CARTESIAN_POINT ( 'NONE',  ( -20.20127174136113979, 10.94879929003026575, -15.94514669860665812 ) ) ;
#779 = CARTESIAN_POINT ( 'NONE',  ( 7.766013557953382218, 28.81973365084987293, 10.00000000000000000 ) ) ;
#780 = CARTESIAN_POINT ( 'NONE',  ( 9.559327499438646569, -18.18575031750659576, -28.70543891380848933 ) ) ;
#781 = CARTESIAN_POINT ( 'NONE',  ( -11.44473057578096764, 31.45924896672619298, 7.500000000000004441 ) ) ;
#782 = CARTESIAN_POINT ( 'NONE',  ( 11.84840861761741770, 19.42896758927500755, -21.60864054467572970 ) ) ;
#783 = CARTESIAN_POINT ( 'NONE',  ( -6.023418944065151770, 39.81932404830322270, -14.45070082761206365 ) ) ;
#784 = FACE_OUTER_BOUND ( 'NONE', #14646, .T. ) ;
#785 = CARTESIAN_POINT ( 'NONE',  ( -25.61532841618020129, -25.51455009192830659, -7.602007375326987670 ) ) ;
#786 = CARTESIAN_POINT ( 'NONE',  ( 6.254033923143232698, -25.07628688208260215, -5.959964782852217979 ) ) ;
#787 = CARTESIAN_POINT ( 'NONE',  ( 12.02371930289417712, 19.24250431711205422, -21.63974928700125844 ) ) ;
#788 = CARTESIAN_POINT ( 'NONE',  ( 28.51898608182493433, -20.62815466463653635, -11.07930801063890591 ) ) ;
#789 = EDGE_CURVE ( 'NONE', #38536, #6543, #27496, .T. ) ;
#790 = CARTESIAN_POINT ( 'NONE',  ( 14.11133924723983490, 27.61078317377175395, 10.49999999999999112 ) ) ;
#791 = CARTESIAN_POINT ( 'NONE',  ( -0.9999999999999997780, 36.00000000000000711, 10.50000000000000000 ) ) ;
#792 = ORIENTED_EDGE ( 'NONE', *, *, #25775, .F. ) ;
#793 = CARTESIAN_POINT ( 'NONE',  ( -5.299830568715972134, 19.88204471691616249, -28.50950821733531271 ) ) ;
#794 = CARTESIAN_POINT ( 'NONE',  ( 14.47283171447379146, 21.48159823030311344, 11.00000000000000000 ) ) ;
#795 = ORIENTED_EDGE ( 'NONE', *, *, #33606, .T. ) ;
#796 = CARTESIAN_POINT ( 'NONE',  ( 20.97107657471919140, 0.7936463442397385659, -26.22365389466587970 ) ) ;
#797 = EDGE_CURVE ( 'NONE', #24743, #614, #12560, .T. ) ;
#798 = CYLINDRICAL_SURFACE ( 'NONE', #21949, 0.4999999999999981681 ) ;
#799 = AXIS2_PLACEMENT_3D ( 'NONE', #36695, #5807, #18404 ) ;
#800 = CARTESIAN_POINT ( 'NONE',  ( -10.33795143809923545, 20.40792924032147226, 10.49999999999999467 ) ) ;
#801 = ADVANCED_FACE ( 'NONE', ( #34005 ), #24850, .F. ) ;
#802 = VERTEX_POINT ( 'NONE', #27695 ) ;
#803 = CARTESIAN_POINT ( 'NONE',  ( -29.22185649745145852, 0.2267782905184046460, -10.65771505781855844 ) ) ;
#804 = CARTESIAN_POINT ( 'NONE',  ( -20.43668243666616391, -27.04690956338842867, -6.800953625924956114 ) ) ;
#805 = ORIENTED_EDGE ( 'NONE', *, *, #87, .F. ) ;
#806 = CARTESIAN_POINT ( 'NONE',  ( 30.02603344819934961, -7.132601230694261218, -13.96448966489334254 ) ) ;
#807 = AXIS2_PLACEMENT_3D ( 'NONE', #26934, #39521, #39719 ) ;
#808 = AXIS2_PLACEMENT_3D ( 'NONE', #20811, #5557, #5361 ) ;
#809 = ORIENTED_EDGE ( 'NONE', *, *, #16122, .T. ) ;
#810 = SHAPE_DEFINITION_REPRESENTATION ( #13590, #33787 ) ;
#811 = CARTESIAN_POINT ( 'NONE',  ( -13.75539757512625272, 34.17605197834731712, 12.14047268033125171 ) ) ;
#812 = DIRECTION ( 'NONE',  ( 0.000000000000000000, 0.000000000000000000, 1.000000000000000000 ) ) ;
#813 = LINE ( 'NONE', #34149, #15004 ) ;
#814 = CARTESIAN_POINT ( 'NONE',  ( 7.971538940948045493, 30.92644086612910570, 19.66345542862527651 ) ) ;
#815 = DIRECTION ( 'NONE',  ( 0.000000000000000000, 0.000000000000000000, -1.000000000000000000 ) ) ;
#816 = ORIENTED_EDGE ( 'NONE', *, *, #29193, .T. ) ;
#817 = AXIS2_PLACEMENT_3D ( 'NONE', #2928, #34208, #30371 ) ;
#818 =( NAMED_UNIT ( * ) SI_UNIT ( $, .STERADIAN. ) SOLID_ANGLE_UNIT ( ) );
#819 = CARTESIAN_POINT ( 'NONE',  ( 8.691530736372195420, 18.57012985596350774, -29.99999999999999645 ) ) ;
#820 = DIRECTION ( 'NONE',  ( 0.000000000000000000, 0.000000000000000000, 1.000000000000000000 ) ) ;
#821 = EDGE_CURVE ( 'NONE', #30083, #13640, #37873, .T. ) ;
#822 = CARTESIAN_POINT ( 'NONE',  ( 12.05736835487432579, 14.38397459621550567, 10.49999999999999822 ) ) ;
#823 = CARTESIAN_POINT ( 'NONE',  ( 18.08305879496937507, 18.91083807987443777, -6.919464382693917059 ) ) ;
#824 = VECTOR ( 'NONE', #14516, 1000.000000000000114 ) ;
#825 = CARTESIAN_POINT ( 'NONE',  ( 9.988892050414650114, 34.83439005035236846, -6.311689768854881422 ) ) ;
#826 = ORIENTED_EDGE ( 'NONE', *, *, #18908, .F. ) ;
#827 = CIRCLE ( 'NONE', #29361, 1.000000000000000000 ) ;
#828 = CARTESIAN_POINT ( 'NONE',  ( 15.07574506840335182, -25.19415529391676145, -11.54849945562353675 ) ) ;
#829 = CARTESIAN_POINT ( 'NONE',  ( 8.293999462566144842, 11.53598992149257008, 12.00000000000000000 ) ) ;
#830 = CARTESIAN_POINT ( 'NONE',  ( 3.784364466546041417, 47.62563423532509432, 7.000000000000000000 ) ) ;
#831 = ORIENTED_EDGE ( 'NONE', *, *, #16332, .F. ) ;
#832 = CARTESIAN_POINT ( 'NONE',  ( -15.41919230091076187, 26.77186013819068577, -5.000000000000001776 ) ) ;
#833 = AXIS2_PLACEMENT_3D ( 'NONE', #38271, #31970, #16136 ) ;
#834 = CARTESIAN_POINT ( 'NONE',  ( -35.08888820711664636, -5.671254737730515139, 15.72805884748985861 ) ) ;
#835 = CARTESIAN_POINT ( 'NONE',  ( 9.471631541704100599, -18.70210992107973880, -26.25392865717030233 ) ) ;
#836 = CARTESIAN_POINT ( 'NONE',  ( 0.000000000000000000, 22.50000000000000355, 7.000000000000000000 ) ) ;
#837 = ORIENTED_EDGE ( 'NONE', *, *, #21012, .F. ) ;
#838 = B_SPLINE_CURVE_WITH_KNOTS ( 'NONE', 3,
 ( #28197, #3416, #573, #3223, #34107, #28798 ),
 .UNSPECIFIED., .F., .F.,
 ( 4, 2, 4 ),
 ( 0.7014326802556738460, 0.8507163401278369230, 1.000000000000000000 ),
 .UNSPECIFIED. ) ;
#839 = VERTEX_POINT ( 'NONE', #14916 ) ;
#840 = CARTESIAN_POINT ( 'NONE',  ( -12.69759596664596479, 27.62578264501285474, -12.31174057995972859 ) ) ;
#841 = CARTESIAN_POINT ( 'NONE',  ( -18.07439754813544042, -24.11643431014769234, -13.20271803398926735 ) ) ;
#842 = EDGE_CURVE ( 'NONE', #17938, #4137, #39467, .T. ) ;
#843 = AXIS2_PLACEMENT_3D ( 'NONE', #11726, #1991, #14371 ) ;
#844 = FACE_BOUND ( 'NONE', #6698, .T. ) ;
#845 = CARTESIAN_POINT ( 'NONE',  ( -20.56951523689105343, -4.408057065260900131, -26.45586068485761189 ) ) ;
#846 = DIRECTION ( 'NONE',  ( -0.4156269377774569063, -0.5720614028176815857, -0.7071067811865476838 ) ) ;
#847 = EDGE_LOOP ( 'NONE', ( #36208, #23534, #21814, #12695 ) ) ;
#848 = CARTESIAN_POINT ( 'NONE',  ( 23.25665023848704749, 0.7203469195909389944, -20.56232886303743257 ) ) ;
#849 = CARTESIAN_POINT ( 'NONE',  ( 11.47989394321261258, 18.44111858363577383, -23.85327844017400523 ) ) ;
#850 = DIRECTION ( 'NONE',  ( 0.1045284632676569680, 0.9945218953682729568, -0.000000000000000000 ) ) ;
#851 = EDGE_CURVE ( 'NONE', #39696, #20959, #15707, .T. ) ;
#852 = EDGE_LOOP ( 'NONE', ( #11085, #1876, #20436, #35870 ) ) ;
#853 = CARTESIAN_POINT ( 'NONE',  ( -29.63796514091300338, 0.003639834609975854327, -10.17682443054809838 ) ) ;
#854 = CARTESIAN_POINT ( 'NONE',  ( -17.47510495690846355, -31.20661830902342615, 11.00000000000000000 ) ) ;
#855 = VERTEX_POINT ( 'NONE', #24451 ) ;
#856 = CARTESIAN_POINT ( 'NONE',  ( 30.99264825080417651, -2.094996292503707558, -10.50450261084496262 ) ) ;
#857 = AXIS2_PLACEMENT_3D ( 'NONE', #18083, #5474, #30473 ) ;
#858 = DIRECTION ( 'NONE',  ( 0.000000000000000000, 0.000000000000000000, 1.000000000000000000 ) ) ;
#859 = CARTESIAN_POINT ( 'NONE',  ( 35.14638740386845939, -7.516303343517492408, 16.30093088680192892 ) ) ;
#860 = VERTEX_POINT ( 'NONE', #18763 ) ;
#861 = VECTOR ( 'NONE', #15724, 1000.000000000000000 ) ;
#862 = CARTESIAN_POINT ( 'NONE',  ( -14.95773623274140895, 28.45553334944834489, 16.30093088680134983 ) ) ;
#863 = FACE_OUTER_BOUND ( 'NONE', #16552, .T. ) ;
#864 = CARTESIAN_POINT ( 'NONE',  ( -3.456468065140321233, 26.15323006594350019, 20.99999999999998934 ) ) ;
#865 = AXIS2_PLACEMENT_3D ( 'NONE', #33227, #35660, #17588 ) ;
#866 = DIRECTION ( 'NONE',  ( 0.9135454576426004225, -0.4067366430758009854, 0.000000000000000000 ) ) ;
#867 = EDGE_CURVE ( 'NONE', #37025, #33408, #28133, .T. ) ;
#868 = FACE_OUTER_BOUND ( 'NONE', #1524, .T. ) ;
#869 = ADVANCED_FACE ( 'NONE', ( #39494, #24256, #11671, #27502, #8821, #24652, #5564, #24058, #21208, #2722, #33618, #9020, #5768, #21014, #33423, #12264, #33812, #5960, #30362, #2529, #74, #27898, #21601, #27305, #30562, #37046, #18364, #30759, #15112, #39885, #12458, #12062, #2921, #9216, #15309, #30951, #3119, #15516, #34795, #25845, #35195, #3910, #6749, #25251, #38246, #22595, #6945, #10414, #9622, #31749, #22796, #38041, #9816, #28297, #13251, #25642, #37837, #3515, #7353, #22002, #19757, #32155, #34401, #28693, #13048, #25438, #4315, #28094, #28899, #473, #15912, #871, #31545, #274, #19352, #22392, #16310, #12659, #25051, #35004, #12856, #37646, #37445, #7153, #10210, #6552 ), #19551, .F. ) ;
#870 = VECTOR ( 'NONE', #18177, 1000.000000000000114 ) ;
#871 = FACE_BOUND ( 'NONE', #16938, .T. ) ;
#872 = CIRCLE ( 'NONE', #33967, 1.000000000000000000 ) ;
#873 = CARTESIAN_POINT ( 'NONE',  ( 14.67741354573947810, 20.96472719003773477, 18.42518152271840037 ) ) ;
#874 = CARTESIAN_POINT ( 'NONE',  ( -19.24333380943624050, 7.104126583969421205, -29.42120498672176154 ) ) ;
#875 = CARTESIAN_POINT ( 'NONE',  ( 19.08127237847830315, -22.31786008396426624, -14.97965334449903629 ) ) ;
#876 = DIRECTION ( 'NONE',  ( 0.000000000000000000, 0.000000000000000000, -1.000000000000000000 ) ) ;
#877 = ORIENTED_EDGE ( 'NONE', *, *, #27021, .F. ) ;
#878 = CARTESIAN_POINT ( 'NONE',  ( 15.36998952511977912, 26.94570423236723755, -5.000000000000000888 ) ) ;
#879 = VECTOR ( 'NONE', #28401, 1000.000000000000000 ) ;
#880 = VERTEX_POINT ( 'NONE', #4109 ) ;
#881 = CARTESIAN_POINT ( 'NONE',  ( -15.13444618763030469, 24.74347023186265204, -10.19675551309649997 ) ) ;
#882 = CARTESIAN_POINT ( 'NONE',  ( -29.20803623499946511, -13.20745421916120499, 20.25080042701566541 ) ) ;
#883 = CARTESIAN_POINT ( 'NONE',  ( -2.229437847141422679, 24.50739181907689712, 12.00000000000000000 ) ) ;
#884 = CARTESIAN_POINT ( 'NONE',  ( 11.21793679047693892, 17.73202320564904966, -26.22846769416230472 ) ) ;
#885 = ORIENTED_EDGE ( 'NONE', *, *, #33735, .F. ) ;
#886 = CARTESIAN_POINT ( 'NONE',  ( 29.77249239352657284, -15.24433919496233258, -12.89210252282047797 ) ) ;
#887 = DIRECTION ( 'NONE',  ( 1.000000000000000000, 0.000000000000000000, 0.000000000000000000 ) ) ;
#888 = VERTEX_POINT ( 'NONE', #16516 ) ;
#890 = CARTESIAN_POINT ( 'NONE',  ( -2.211402178667006169, 32.38366924255629442, 6.000000000000000000 ) ) ;
#889 = CARTESIAN_POINT ( 'NONE',  ( -15.23011890149219738, 27.15271631207409797, -6.409557253276911837 ) ) ;
#891 = CARTESIAN_POINT ( 'NONE',  ( -9.617847002920147048, -18.10379274102027836, -29.34587326035947541 ) ) ;
#892 = EDGE_CURVE ( 'NONE', #1059, #25293, #22193, .T. ) ;
#893 = CYLINDRICAL_SURFACE ( 'NONE', #39346, 1.000000000000000888 ) ;
#894 = CIRCLE ( 'NONE', #2839, 1.000000000000000000 ) ;
#895 = ORIENTED_EDGE ( 'NONE', *, *, #15860, .F. ) ;
#896 = CARTESIAN_POINT ( 'NONE',  ( -35.24776836081323239, -13.33918002079275844, -6.287261223954184075 ) ) ;
#897 = CARTESIAN_POINT ( 'NONE',  ( -8.710418783113659913, -18.55732502341819767, -29.99999999999999645 ) ) ;
#898 = CARTESIAN_POINT ( 'NONE',  ( 0.5000000000000000000, 37.00000000000000711, 7.000000000000000000 ) ) ;
#899 = CARTESIAN_POINT ( 'NONE',  ( 15.07270250660410227, 20.73502926711271854, -14.63261333351891480 ) ) ;
#900 = ORIENTED_EDGE ( 'NONE', *, *, #18324, .F. ) ;
#901 = CARTESIAN_POINT ( 'NONE',  ( 26.80184643760344798, 3.774889638419365312, -9.304333590497897433 ) ) ;
#902 = CARTESIAN_POINT ( 'NONE',  ( 13.30736791475921699, 15.68301270237638967, 10.49999999999999822 ) ) ;
#903 = CARTESIAN_POINT ( 'NONE',  ( -24.37759566069532724, -10.08322588119026797, 23.00000000000000000 ) ) ;
#904 = ORIENTED_EDGE ( 'NONE', *, *, #35439, .F. ) ;
#905 = EDGE_CURVE ( 'NONE', #13411, #2697, #37018, .T. ) ;
#906 = CARTESIAN_POINT ( 'NONE',  ( -20.62742209940435600, 0.5119082021479205435, -28.06054629692573243 ) ) ;
#907 = CARTESIAN_POINT ( 'NONE',  ( 30.31228144303179661, -0.3231585995110547449, -9.216521076407452995 ) ) ;
#908 = CIRCLE ( 'NONE', #24889, 1.000000000000000000 ) ;
#909 = CARTESIAN_POINT ( 'NONE',  ( 30.28108141855193480, -11.05112898844763514, 19.99202127657103034 ) ) ;
#910 = ORIENTED_EDGE ( 'NONE', *, *, #29653, .F. ) ;
#911 = CARTESIAN_POINT ( 'NONE',  ( -20.55563217186184133, -29.52600041847739476, -4.999999999999992006 ) ) ;
#912 = CIRCLE ( 'NONE', #27540, 1.000000000000000888 ) ;
#913 = CARTESIAN_POINT ( 'NONE',  ( 5.400683141673458643, 15.91724817395916070, 9.000000000000001776 ) ) ;
#914 = ORIENTED_EDGE ( 'NONE', *, *, #26901, .F. ) ;
#915 = DIRECTION ( 'NONE',  ( -0.6691306063588671194, -0.7431448254773861395, -0.000000000000000000 ) ) ;
#916 = EDGE_CURVE ( 'NONE', #33995, #4123, #669, .T. ) ;
#917 = VECTOR ( 'NONE', #27944, 1000.000000000000114 ) ;
#918 = FACE_OUTER_BOUND ( 'NONE', #33899, .T. ) ;
#919 = DIRECTION ( 'NONE',  ( 0.000000000000000000, 0.000000000000000000, 1.000000000000000000 ) ) ;
#920 = CARTESIAN_POINT ( 'NONE',  ( -2.036571916123810055, 8.108948098542073879, 7.499999999999997335 ) ) ;
#921 = EDGE_LOOP ( 'NONE', ( #7988, #20870 ) ) ;
#922 = CARTESIAN_POINT ( 'NONE',  ( 5.724371395536106633, 32.23037938972932892, 13.00000000000000178 ) ) ;
#923 = DIRECTION ( 'NONE',  ( 1.000000000000000000, 0.000000000000000000, 0.000000000000000000 ) ) ;
#924 = CARTESIAN_POINT ( 'NONE',  ( 16.57621650368579935, -13.52450271667361648, -25.63860445636134244 ) ) ;
#925 = DIRECTION ( 'NONE',  ( 1.000000000000000000, 0.000000000000000000, 0.000000000000000000 ) ) ;
#926 = CARTESIAN_POINT ( 'NONE',  ( 14.44277748876681855, 26.55045409923015853, 7.000000000000000000 ) ) ;
#927 = CARTESIAN_POINT ( 'NONE',  ( 10.41696638283783471, 17.65700839937217381, -30.00000000000000355 ) ) ;
#928 = CARTESIAN_POINT ( 'NONE',  ( 13.19674782540804792, 16.00858767546125350, 10.49999999999999822 ) ) ;
#929 = ORIENTED_EDGE ( 'NONE', *, *, #21435, .F. ) ;
#931 = CARTESIAN_POINT ( 'NONE',  ( 8.927394655428274817, 11.06314620770945112, 9.500000000000000000 ) ) ;
#930 = CARTESIAN_POINT ( 'NONE',  ( -16.52919907445785697, 19.39618867232801591, -12.74319168300435123 ) ) ;
#932 = AXIS2_PLACEMENT_3D ( 'NONE', #35100, #7255, #38346 ) ;
#933 = CARTESIAN_POINT ( 'NONE',  ( -13.36146265112639675, 15.68301270189280672, 7.445905703748357141 ) ) ;
#934 = CARTESIAN_POINT ( 'NONE',  ( 12.62357604078584572, -22.55721479133982044, -16.44622715326968532 ) ) ;
#935 = DIRECTION ( 'NONE',  ( -0.000000000000000000, -0.000000000000000000, -1.000000000000000000 ) ) ;
#936 = CARTESIAN_POINT ( 'NONE',  ( 14.93762947894291493, 25.79075299017892320, -9.709418743867059831 ) ) ;
#937 = ORIENTED_EDGE ( 'NONE', *, *, #26202, .T. ) ;
#938 = CARTESIAN_POINT ( 'NONE',  ( 15.41558956916364664, 26.78481017491955285, -5.474206059968303784 ) ) ;
#939 = PRODUCT ( 'BR-834', 'BR-834', '', ( #29440 ) ) ;
#940 = ORIENTED_EDGE ( 'NONE', *, *, #29925, .F. ) ;
#942 = DIRECTION ( 'NONE',  ( 0.9510565162951504226, -0.3090169943749573322, 0.000000000000000000 ) ) ;
#941 = CARTESIAN_POINT ( 'NONE',  ( -11.26290815293687686, 18.07476739303793067, -25.00808982776462841 ) ) ;
#943 = CARTESIAN_POINT ( 'NONE',  ( -14.82428456515288673, -25.82275059238470760, -9.709745829346953627 ) ) ;
#944 = EDGE_CURVE ( 'NONE', #35769, #14313, #38446, .T. ) ;
#945 = CARTESIAN_POINT ( 'NONE',  ( -37.38745755834736428, -10.91949489986329347, 12.73282698324913831 ) ) ;
#946 = CARTESIAN_POINT ( 'NONE',  ( -19.10838325939929661, -14.03250534646638137, -21.87301868147889650 ) ) ;
#947 = CARTESIAN_POINT ( 'NONE',  ( -7.052297394767913730, -25.17996142191265463, -5.478637597918203817 ) ) ;
#948 = CARTESIAN_POINT ( 'NONE',  ( 15.36816765326552314, 25.28887897332994328, -8.776245744413783356 ) ) ;
#950 = EDGE_CURVE ( 'NONE', #4321, #28310, #29705, .T. ) ;
#949 = ORIENTED_EDGE ( 'NONE', *, *, #13774, .F. ) ;
#951 = CARTESIAN_POINT ( 'NONE',  ( 20.10518103393213352, 8.324311984002667586, -21.14455001357749708 ) ) ;
#952 = CARTESIAN_POINT ( 'NONE',  ( -15.33540831873584587, 35.51988610398909429, 10.99999999999999822 ) ) ;
#953 = CARTESIAN_POINT ( 'NONE',  ( -7.449887436100933513, 34.87105630051663496, 17.92354375535170874 ) ) ;
#954 = ORIENTED_EDGE ( 'NONE', *, *, #24516, .T. ) ;
#955 = CARTESIAN_POINT ( 'NONE',  ( -33.52901403654990276, -3.501605748354566394, -5.457694923509727403 ) ) ;
#956 = VECTOR ( 'NONE', #36154, 1000.000000000000000 ) ;
#957 = EDGE_CURVE ( 'NONE', #26836, #32713, #21640, .T. ) ;
#958 = CARTESIAN_POINT ( 'NONE',  ( -14.79097147050020311, 14.99953367534935822, 19.66345542862526585 ) ) ;
#959 = VERTEX_POINT ( 'NONE', #13657 ) ;
#960 = CARTESIAN_POINT ( 'NONE',  ( 20.92112759555554291, -16.07000418475260162, 20.99999999999999645 ) ) ;
#961 = DIRECTION ( 'NONE',  ( 0.000000000000000000, 0.000000000000000000, 1.000000000000000000 ) ) ;
#962 = CARTESIAN_POINT ( 'NONE',  ( 34.52637764006742316, -16.38715731849997681, -6.278547096120509430 ) ) ;
#963 = CARTESIAN_POINT ( 'NONE',  ( 37.52525227335095082, -10.91693234368658061, 12.14047268033090532 ) ) ;
#964 = EDGE_LOOP ( 'NONE', ( #31219, #25857, #1045, #21630 ) ) ;
#965 = ORIENTED_EDGE ( 'NONE', *, *, #34679, .F. ) ;
#966 = DIRECTION ( 'NONE',  ( -0.5000000000000038858, -0.8660254037844364872, 0.000000000000000000 ) ) ;
#967 = CARTESIAN_POINT ( 'NONE',  ( -20.20214925928707572, 14.56229221429976128, -5.000000000000000000 ) ) ;
#968 = EDGE_CURVE ( 'NONE', #18645, #35629, #176, .T. ) ;
#969 = EDGE_CURVE ( 'NONE', #18974, #18778, #38852, .T. ) ;
#970 = VECTOR ( 'NONE', #2003, 1000.000000000000114 ) ;
#971 = CARTESIAN_POINT ( 'NONE',  ( -10.44103466624267185, 32.57396620494226624, 7.000000000000000000 ) ) ;
#972 = ORIENTED_EDGE ( 'NONE', *, *, #34521, .F. ) ;
#973 = CARTESIAN_POINT ( 'NONE',  ( -1.088922936409942421, 21.99923614848890097, -24.22294042631511246 ) ) ;
#974 = CARTESIAN_POINT ( 'NONE',  ( -15.21736038221435727, 17.55712500267617315, 13.00000000000000178 ) ) ;
#975 = FACE_OUTER_BOUND ( 'NONE', #36778, .T. ) ;
#976 = STYLED_ITEM ( 'NONE', ( #32825 ), #34952 ) ;
#977 = CARTESIAN_POINT ( 'NONE',  ( 13.03640989728592459, 29.14264673470096767, 13.00000000000000178 ) ) ;
#978 = FACE_OUTER_BOUND ( 'NONE', #35617, .T. ) ;
#979 = FACE_OUTER_BOUND ( 'NONE', #25316, .T. ) ;
#980 = CARTESIAN_POINT ( 'NONE',  ( 14.23920029309381974, 28.74314447264790928, -8.209473521281651642 ) ) ;
#982 = VECTOR ( 'NONE', #8472, 1000.000000000000000 ) ;
#981 = DIRECTION ( 'NONE',  ( 0.8090169943749504489, 0.5877852522924689183, 0.000000000000000000 ) ) ;
#983 = ORIENTED_EDGE ( 'NONE', *, *, #3827, .F. ) ;
#985 = LINE ( 'NONE', #10523, #15475 ) ;
#984 = CARTESIAN_POINT ( 'NONE',  ( -20.28121371388173344, 13.36466378765053165, -10.38440001512937627 ) ) ;
#986 = DIRECTION ( 'NONE',  ( 0.000000000000000000, 0.000000000000000000, 1.000000000000000000 ) ) ;
#987 = CARTESIAN_POINT ( 'NONE',  ( 12.33240784613131602, -22.02210067590966958, -17.43238452351191370 ) ) ;
#988 = LINE ( 'NONE', #13370, #29539 ) ;
#989 = CARTESIAN_POINT ( 'NONE',  ( 15.38567911973872171, 26.79894733746586510, -5.945569934900782449 ) ) ;
#990 = CARTESIAN_POINT ( 'NONE',  ( 3.091399026088761826, 22.35909668862748489, -19.80438750953543803 ) ) ;
#991 = LINE ( 'NONE', #7683, #5762 ) ;
#992 = EDGE_CURVE ( 'NONE', #16279, #36570, #31383, .T. ) ;
#993 = CARTESIAN_POINT ( 'NONE',  ( -14.07208788724811477, -14.92005942896404669, -29.25347274896327932 ) ) ;
#994 = CARTESIAN_POINT ( 'NONE',  ( 5.770784699189574596, -20.01892754147923270, -26.51040416381328058 ) ) ;
#995 = CARTESIAN_POINT ( 'NONE',  ( 14.80735206003844340, 25.19352138484959980, -10.65771637371773117 ) ) ;
#996 = EDGE_CURVE ( 'NONE', #36577, #34828, #35607, .T. ) ;
#997 = CARTESIAN_POINT ( 'NONE',  ( 26.16185303258038886, -18.91739542788047501, -13.82176542154406818 ) ) ;
#998 = CARTESIAN_POINT ( 'NONE',  ( -19.48557158514998022, -11.24999999999982414, -5.000000000000000000 ) ) ;
#999 = DIRECTION ( 'NONE',  ( 0.000000000000000000, 0.000000000000000000, 1.000000000000000000 ) ) ;
#1000 = ORIENTED_EDGE ( 'NONE', *, *, #15480, .F. ) ;
#1001 = CARTESIAN_POINT ( 'NONE',  ( -6.470191821340285365, 24.31185124780299844, -19.83456026983462905 ) ) ;
#1002 = CIRCLE ( 'NONE', #26954, 0.5000000000000004441 ) ;
#1003 = DIRECTION ( 'NONE',  ( -0.07391278520356937831, -0.7032331762534056452, 0.7071067811865457964 ) ) ;
#1004 = ORIENTED_EDGE ( 'NONE', *, *, #36950, .F. ) ;
#1005 = CARTESIAN_POINT ( 'NONE',  ( 30.88264071866746008, -0.05584998072600699803, -5.946076430058510276 ) ) ;
#1006 = DIRECTION ( 'NONE',  ( 1.000000000000000000, 0.000000000000000000, 0.000000000000000000 ) ) ;
#1007 = CARTESIAN_POINT ( 'NONE',  ( -29.28423149095162259, -1.632116715639065463, 18.42518152272108978 ) ) ;
#1008 = ORIENTED_EDGE ( 'NONE', *, *, #2242, .F. ) ;
#1009 = CIRCLE ( 'NONE', #38616, 16.00000000000000000 ) ;
#1010 = CARTESIAN_POINT ( 'NONE',  ( -26.44429670257990495, 0.3694839107847344151, -15.45773263958803945 ) ) ;
#1011 = CARTESIAN_POINT ( 'NONE',  ( 8.410254037844358876, 17.06698729810774395, 10.49999999999999822 ) ) ;
#1012 = ORIENTED_EDGE ( 'NONE', *, *, #30842, .F. ) ;
#1013 = CARTESIAN_POINT ( 'NONE',  ( 33.18948647224070214, -7.908499970437028459, -10.28410421794941776 ) ) ;
#1014 = CIRCLE ( 'NONE', #6200, 1.000000000000000000 ) ;
#1015 = AXIS2_PLACEMENT_3D ( 'NONE', #7326, #10794, #26626 ) ;
#1016 = ORIENTED_EDGE ( 'NONE', *, *, #29221, .F. ) ;
#1017 = PRODUCT_CONTEXT ( 'NONE', #21521, 'mechanical' ) ;
#1018 = DIRECTION ( 'NONE',  ( 0.000000000000000000, 0.000000000000000000, 1.000000000000000000 ) ) ;
#1019 = LINE ( 'NONE', #9364, #17089 ) ;
#1020 = CARTESIAN_POINT ( 'NONE',  ( -8.401171878996500197, 21.11424711454089476, 9.000000000000001776 ) ) ;
#1021 = CARTESIAN_POINT ( 'NONE',  ( -6.977707682421693924, 31.68171018602201983, 19.66345542862527651 ) ) ;
#1022 = LINE ( 'NONE', #19908, #16824 ) ;
#1023 = ORIENTED_EDGE ( 'NONE', *, *, #968, .T. ) ;
#1024 = CARTESIAN_POINT ( 'NONE',  ( -12.43436401264212954, 16.30149266761548787, -29.99999999999998579 ) ) ;
#1025 = PLANE ( 'NONE',  #27349 ) ;
#1026 = EDGE_CURVE ( 'NONE', #1570, #35419, #19056, .T. ) ;
#1027 = FACE_OUTER_BOUND ( 'NONE', #29182, .T. ) ;
#1028 = CARTESIAN_POINT ( 'NONE',  ( 16.44760013473877791, 18.13359219541155909, -14.76563877920854573 ) ) ;
#1029 = CARTESIAN_POINT ( 'NONE',  ( 8.055990078716707359, 27.84801368489809192, -15.86024324141795105 ) ) ;
#1030 = ORIENTED_EDGE ( 'NONE', *, *, #916, .T. ) ;
#1031 = DIRECTION ( 'NONE',  ( 0.000000000000000000, 0.000000000000000000, 1.000000000000000000 ) ) ;
#1032 = CARTESIAN_POINT ( 'NONE',  ( 0.000000000000000000, 22.50000000000000355, 7.000000000000000000 ) ) ;
#1033 = CARTESIAN_POINT ( 'NONE',  ( 10.44076220327837135, -18.61599742478032127, -24.95863081061211020 ) ) ;
#1034 = CARTESIAN_POINT ( 'NONE',  ( 2.594149110900750621, 26.80855565015184894, 20.99999999999999289 ) ) ;
#1035 = DIRECTION ( 'NONE',  ( -1.000000000000000000, 0.000000000000000000, 0.000000000000000000 ) ) ;
#1036 = ORIENTED_EDGE ( 'NONE', *, *, #9740, .F. ) ;
#1037 = AXIS2_PLACEMENT_3D ( 'NONE', #25052, #28298, #18959 ) ;
#1038 = CARTESIAN_POINT ( 'NONE',  ( -11.08838803815796048, 17.49214405190394217, -27.44899145124595918 ) ) ;
#1039 = CIRCLE ( 'NONE', #14000, 1.000000000000000000 ) ;
#1040 = CARTESIAN_POINT ( 'NONE',  ( -35.58257249438602798, -10.95300747732907354, 16.30093088680272118 ) ) ;
#1041 = CARTESIAN_POINT ( 'NONE',  ( 14.97886844088684200, -26.54010076781190364, -6.417509905602858389 ) ) ;
#1042 = AXIS2_PLACEMENT_3D ( 'NONE', #7873, #10730, #26571 ) ;
#1043 = DIRECTION ( 'NONE',  ( 0.9781476007338070211, 0.2079116908177532919, 0.000000000000000000 ) ) ;
#1044 = ORIENTED_EDGE ( 'NONE', *, *, #7401, .F. ) ;
#1045 = ORIENTED_EDGE ( 'NONE', *, *, #14187, .F. ) ;
#1046 = CARTESIAN_POINT ( 'NONE',  ( -11.80691721808442018, 25.54223282131769324, -15.16446032101342034 ) ) ;
#1047 = DIRECTION ( 'NONE',  ( 0.000000000000000000, 0.000000000000000000, 1.000000000000000000 ) ) ;
#1048 = CARTESIAN_POINT ( 'NONE',  ( -12.60100158617414934, 14.64745807297398983, 10.87262190629281378 ) ) ;
#1049 = CARTESIAN_POINT ( 'NONE',  ( -20.04600691274970714, -4.289688609580842638, -29.25985845626247084 ) ) ;
#1050 = PLANE ( 'NONE',  #22867 ) ;
#1051 = ORIENTED_EDGE ( 'NONE', *, *, #1452, .F. ) ;
#1052 = CARTESIAN_POINT ( 'NONE',  ( 27.05411555961266856, 0.3588468966283088202, -14.48483347321499259 ) ) ;
#1053 = CYLINDRICAL_SURFACE ( 'NONE', #33678, 1.000000000000000000 ) ;
#1054 = CARTESIAN_POINT ( 'NONE',  ( -4.835137251120299240, 29.44922644035488446, 12.00000000000000000 ) ) ;
#1055 = EDGE_CURVE ( 'NONE', #39013, #24143, #4522, .T. ) ;
#1056 = ORIENTED_EDGE ( 'NONE', *, *, #19803, .T. ) ;
#1057 = CARTESIAN_POINT ( 'NONE',  ( -27.75511952204637112, 0.1671360698226562469, -13.51159890575608458 ) ) ;
#1058 = LINE ( 'NONE', #30989, #24781 ) ;
#1059 = VERTEX_POINT ( 'NONE', #26046 ) ;
#1060 = CARTESIAN_POINT ( 'NONE',  ( 20.88781296840016566, -0.9792067608458780992, -26.69013418581465658 ) ) ;
#1061 = CARTESIAN_POINT ( 'NONE',  ( 16.08977793723792615, 12.77418664379545277, -30.00000000000000000 ) ) ;
#1062 = CARTESIAN_POINT ( 'NONE',  ( 35.36447994912680315, -9.234655410422998756, 16.30093088680190760 ) ) ;
#1063 = ORIENTED_EDGE ( 'NONE', *, *, #14261, .T. ) ;
#1064 = CARTESIAN_POINT ( 'NONE',  ( -3.569741787452771042, 38.68155838841067151, 15.72805884748945715 ) ) ;
#1065 = VECTOR ( 'NONE', #39012, 1000.000000000000000 ) ;
#1066 = CARTESIAN_POINT ( 'NONE',  ( -5.706342468480190000, 20.64589803375067945, 6.000000000000000000 ) ) ;
#1067 = CARTESIAN_POINT ( 'NONE',  ( -1.596172877504954402, 27.23837864096127959, 20.99999999999999645 ) ) ;
#1068 = AXIS2_PLACEMENT_3D ( 'NONE', #29176, #32221, #13524 ) ;
#1069 = DIRECTION ( 'NONE',  ( 0.000000000000000000, 0.000000000000000000, 1.000000000000000000 ) ) ;
#1070 = AXIS2_PLACEMENT_3D ( 'NONE', #25458, #22617, #31769 ) ;
#1071 = EDGE_CURVE ( 'NONE', #7930, #30348, #29905, .T. ) ;
#1072 = DIRECTION ( 'NONE',  ( 1.000000000000000000, 0.000000000000000000, 0.000000000000000000 ) ) ;
#1073 = B_SPLINE_CURVE_WITH_KNOTS ( 'NONE', 3,
 ( #35093, #37939, #19246, #4618, #7247, #765 ),
 .UNSPECIFIED., .F., .F.,
 ( 4, 2, 4 ),
 ( 0.000000000000000000, 0.5000000000000000000, 1.000000000000000000 ),
 .UNSPECIFIED. ) ;
#1074 = EDGE_CURVE ( 'NONE', #24243, #2749, #16921, .T. ) ;
#1075 = CARTESIAN_POINT ( 'NONE',  ( -11.48173768534022976, 32.16538668264431777, 10.63089969389957012 ) ) ;
#1076 = ADVANCED_FACE ( 'NONE', ( #32767 ), #16717, .F. ) ;
#1077 = CARTESIAN_POINT ( 'NONE',  ( 17.25967040852637169, 21.92197836105680864, 15.72805884747922889 ) ) ;
#1078 = CARTESIAN_POINT ( 'NONE',  ( -22.43125282700144396, 9.709888685033304156, -10.37626387228879921 ) ) ;
#1079 = ADVANCED_FACE ( 'NONE', ( #23613 ), #35403, .F. ) ;
#1080 = CARTESIAN_POINT ( 'NONE',  ( 13.53326846751017776, -16.93861287502592461, -24.59972970754256139 ) ) ;
#1081 = CARTESIAN_POINT ( 'NONE',  ( 3.100636323082810009, 29.29593658752792962, 12.00000000000000000 ) ) ;
#1082 = VERTEX_POINT ( 'NONE', #1477 ) ;
#1083 = CARTESIAN_POINT ( 'NONE',  ( 13.39395081145689126, 23.01331212264283010, -15.42805658671999147 ) ) ;
#1084 = VERTEX_POINT ( 'NONE', #23210 ) ;
#1085 = CARTESIAN_POINT ( 'NONE',  ( -15.32210889896768080, 24.20449498080214568, -10.20718785661471273 ) ) ;
#1086 = CARTESIAN_POINT ( 'NONE',  ( -22.56822310031916956, -21.59793901597470978, 19.99202127657132522 ) ) ;
#1087 = DIRECTION ( 'NONE',  ( -0.000000000000000000, -0.000000000000000000, -1.000000000000000000 ) ) ;
#1088 = CARTESIAN_POINT ( 'NONE',  ( 15.43057444885795526, 26.63884252548692899, -5.946095807145699297 ) ) ;
#1089 = VERTEX_POINT ( 'NONE', #32564 ) ;
#1090 = CARTESIAN_POINT ( 'NONE',  ( 23.49686793660233164, -12.95939375123112924, -18.61325731074879641 ) ) ;
#1091 = CARTESIAN_POINT ( 'NONE',  ( -3.211402178667006169, 32.38366924255629442, 13.00000000000000178 ) ) ;
#1092 = ORIENTED_EDGE ( 'NONE', *, *, #36685, .T. ) ;
#1094 = CARTESIAN_POINT ( 'NONE',  ( -8.160254037844437036, 16.63397459621563712, 10.49999999999999822 ) ) ;
#1093 = CARTESIAN_POINT ( 'NONE',  ( -11.97960752203429635, 20.10336228911335610, -20.51048379201368732 ) ) ;
#1095 = CARTESIAN_POINT ( 'NONE',  ( -15.17654956054996340, -24.76925620166926834, -12.46321089911742419 ) ) ;
#1096 = CARTESIAN_POINT ( 'NONE',  ( 0.000000000000000000, 22.50000000000000355, 0.000000000000000000 ) ) ;
#1097 = ORIENTED_EDGE ( 'NONE', *, *, #1427, .T. ) ;
#1098 = CARTESIAN_POINT ( 'NONE',  ( -29.69559183934828184, -12.23830469681641198, -13.83596335006340361 ) ) ;
#1099 = CARTESIAN_POINT ( 'NONE',  ( -13.96032889325439896, -26.00713114000728154, -8.307085670361487928 ) ) ;
#1100 = DIRECTION ( 'NONE',  ( 1.000000000000000000, 0.000000000000000000, 0.000000000000000000 ) ) ;
#1101 = CARTESIAN_POINT ( 'NONE',  ( 16.44978060298200262, 23.23702767493066901, -6.423945567198219742 ) ) ;
#1102 = EDGE_CURVE ( 'NONE', #6805, #11440, #7390, .T. ) ;
#1103 = ORIENTED_EDGE ( 'NONE', *, *, #25798, .F. ) ;
#1104 = CARTESIAN_POINT ( 'NONE',  ( 20.14573521205405626, 4.508281606648074202, -27.63363721710107157 ) ) ;
#1105 = DIRECTION ( 'NONE',  ( 1.000000000000000000, 0.000000000000000000, 0.000000000000000000 ) ) ;
#1106 = EDGE_CURVE ( 'NONE', #5248, #38699, #11028, .T. ) ;
#1107 = CARTESIAN_POINT ( 'NONE',  ( 0.3582258883630317636, 11.68927977431952137, 13.00000000000000178 ) ) ;
#1108 = EDGE_CURVE ( 'NONE', #22676, #5593, #20373, .T. ) ;
#1109 = ORIENTED_EDGE ( 'NONE', *, *, #6611, .F. ) ;
#1110 = CARTESIAN_POINT ( 'NONE',  ( -22.28238350020720304, 0.4113152637605046458, -22.70236739277193294 ) ) ;
#1111 = CARTESIAN_POINT ( 'NONE',  ( 20.62616697249115560, 0.5412120207698293273, -28.06201873610561748 ) ) ;
#1112 = CARTESIAN_POINT ( 'NONE',  ( 17.92913371968424840, -21.93458435334546408, 19.99202127657079942 ) ) ;
#1113 = ORIENTED_EDGE ( 'NONE', *, *, #23489, .F. ) ;
#1114 = CARTESIAN_POINT ( 'NONE',  ( -16.77267017469753085, -29.13948811618693924, -13.79123840944732748 ) ) ;
#1115 = CARTESIAN_POINT ( 'NONE',  ( -13.99633081586299532, 26.34670874090678439, 10.83333333333333570 ) ) ;
#1116 = DIRECTION ( 'NONE',  ( 0.000000000000000000, 0.000000000000000000, 1.000000000000000000 ) ) ;
#1117 = CYLINDRICAL_SURFACE ( 'NONE', #37924, 1.000000000000000000 ) ;
#1118 = EDGE_CURVE ( 'NONE', #7593, #21179, #16509, .T. ) ;
#1119 = CONICAL_SURFACE ( 'NONE', #1797, 1.000000000000002665, 0.7853981633974509435 ) ;
#1120 = CARTESIAN_POINT ( 'NONE',  ( 23.80624316739448787, 27.22568555153026537, 7.000000000000000000 ) ) ;
#1121 = FACE_OUTER_BOUND ( 'NONE', #18738, .T. ) ;
#1122 = CARTESIAN_POINT ( 'NONE',  ( 12.80736835487432934, 15.68301270189215835, 11.00000000000000000 ) ) ;
#1123 = ORIENTED_EDGE ( 'NONE', *, *, #27299, .F. ) ;
#1124 = DIRECTION ( 'NONE',  ( 1.000000000000000000, 0.000000000000000000, 0.000000000000000000 ) ) ;
#1125 = CARTESIAN_POINT ( 'NONE',  ( 0.9819609608163288872, 14.62372257652092422, 12.00000000000000000 ) ) ;
#1126 = CARTESIAN_POINT ( 'NONE',  ( 15.78360135397623232, -13.68898427767162218, -27.02986149001527849 ) ) ;
#1127 = CIRCLE ( 'NONE', #32283, 1.000000000000000000 ) ;
#1128 = PLANE ( 'NONE',  #15137 ) ;
#1129 = DIRECTION ( 'NONE',  ( 1.224646799147351235E-16, -1.000000000000000000, 0.000000000000000000 ) ) ;
#1130 = CARTESIAN_POINT ( 'NONE',  ( 11.52463565043312776, 19.76527168737703732, -21.54802219502610683 ) ) ;
#1131 = AXIS2_PLACEMENT_3D ( 'NONE', #23713, #26563, #39745 ) ;
#1132 = CARTESIAN_POINT ( 'NONE',  ( 35.48557158514975640, -11.24999999999998046, 10.00000000000000000 ) ) ;
#1133 = ORIENTED_EDGE ( 'NONE', *, *, #27197, .F. ) ;
#1134 = CARTESIAN_POINT ( 'NONE',  ( -17.46789482202738242, 19.19107468640789449, -9.821805770008548819 ) ) ;
#1135 = CARTESIAN_POINT ( 'NONE',  ( -21.72603204741356109, -16.58852365944958862, 20.99999999999999645 ) ) ;
#1136 = CARTESIAN_POINT ( 'NONE',  ( 9.612089455291110696, -18.34516641601810960, -27.44844517416429852 ) ) ;
#1137 = DIRECTION ( 'NONE',  ( -0.3090169943749450643, 0.9510565162951544194, -0.000000000000000000 ) ) ;
#1138 = CARTESIAN_POINT ( 'NONE',  ( 15.42600414702388001, 26.74738280129588475, -5.474195457183328450 ) ) ;
#1139 = VERTEX_POINT ( 'NONE', #39839 ) ;
#1140 = CARTESIAN_POINT ( 'NONE',  ( 15.29107182738991355, 26.52751320015934056, -7.357832120508806639 ) ) ;
#1141 = ORIENTED_EDGE ( 'NONE', *, *, #7030, .T. ) ;
#1143 = LINE ( 'NONE', #31610, #30909 ) ;
#1142 = CARTESIAN_POINT ( 'NONE',  ( -11.85453240479826498, 19.42245932160622601, -21.60981001402871016 ) ) ;
#1144 = CARTESIAN_POINT ( 'NONE',  ( -15.16455904780920605, -26.28013905145489559, -8.298198564278338907 ) ) ;
#1145 = CARTESIAN_POINT ( 'NONE',  ( -35.38210723591855356, -3.548218742175161200, 13.32518128616608877 ) ) ;
#1146 = CARTESIAN_POINT ( 'NONE',  ( -31.16588773407646684, -20.14524002064360886, -8.845864470397883039 ) ) ;
#1147 = CARTESIAN_POINT ( 'NONE',  ( -3.789163634868768504, -21.80995766230909183, -20.07097836427437443 ) ) ;
#1148 = CARTESIAN_POINT ( 'NONE',  ( 11.49276420112067676, 17.21302641401697642, -27.47950092418111012 ) ) ;
#1149 = ORIENTED_EDGE ( 'NONE', *, *, #8604, .F. ) ;
#1150 = CARTESIAN_POINT ( 'NONE',  ( 20.19436507835331440, 7.509872463613282534, -22.18560086142950993 ) ) ;
#1151 = CARTESIAN_POINT ( 'NONE',  ( -5.473344025737326923, 14.11593743010433499, 10.00000000000000000 ) ) ;
#1152 = CARTESIAN_POINT ( 'NONE',  ( -12.63195416618315825, 14.41050271297376462, 7.485646746502369275 ) ) ;
#1153 = EDGE_CURVE ( 'NONE', #21780, #5670, #17808, .T. ) ;
#1154 = CARTESIAN_POINT ( 'NONE',  ( -10.35750558342918737, 33.44896173339029133, 17.42190598798475065 ) ) ;
#1155 = ORIENTED_EDGE ( 'NONE', *, *, #7543, .F. ) ;
#1156 = CARTESIAN_POINT ( 'NONE',  ( -32.75383215441653562, -2.524879539945301232, -6.828243879031231423 ) ) ;
#1157 = VECTOR ( 'NONE', #7333, 1000.000000000000000 ) ;
#1158 = VECTOR ( 'NONE', #19430, 1000.000000000000000 ) ;
#1159 = CARTESIAN_POINT ( 'NONE',  ( -9.534329713701904296, 19.05805734593735679, 20.69868183039760368 ) ) ;
#1160 = EDGE_LOOP ( 'NONE', ( #5743, #16893, #6841, #25465 ) ) ;
#1161 = DIRECTION ( 'NONE',  ( -0.000000000000000000, -0.000000000000000000, -1.000000000000000000 ) ) ;
#1162 = CYLINDRICAL_SURFACE ( 'NONE', #25192, 0.4999999999999999445 ) ;
#1163 = CARTESIAN_POINT ( 'NONE',  ( 32.91113856765019108, -15.59652155672033125, -9.731851003150181256 ) ) ;
#1164 = CARTESIAN_POINT ( 'NONE',  ( 37.45384686740442248, -12.88771083438643927, 12.14047268033111671 ) ) ;
#1165 = ORIENTED_EDGE ( 'NONE', *, *, #15702, .F. ) ;
#1166 = ORIENTED_EDGE ( 'NONE', *, *, #37930, .F. ) ;
#1167 = DIRECTION ( 'NONE',  ( 0.3706816908110067699, -0.7275037805840999239, 0.5773502691896271743 ) ) ;
#1168 = CARTESIAN_POINT ( 'NONE',  ( -15.49888991410544392, 26.48751662061146916, -5.000000000000000000 ) ) ;
#1169 = ADVANCED_FACE ( 'NONE', ( #6654 ), #30108, .T. ) ;
#1170 = CARTESIAN_POINT ( 'NONE',  ( 13.14827996435953139, 25.72067290776661608, 10.00000000000000000 ) ) ;
#1171 = ORIENTED_EDGE ( 'NONE', *, *, #36222, .T. ) ;
#1172 = EDGE_CURVE ( 'NONE', #37413, #7627, #15815, .T. ) ;
#1173 = CARTESIAN_POINT ( 'NONE',  ( -1.884094491940191407, 37.39490938450266100, -8.406240364095751261 ) ) ;
#1174 = DIRECTION ( 'NONE',  ( 1.000000000000000000, 0.000000000000000000, 0.000000000000000000 ) ) ;
#1175 = DIRECTION ( 'NONE',  ( 0.000000000000000000, 0.000000000000000000, 1.000000000000000000 ) ) ;
#1176 = FACE_OUTER_BOUND ( 'NONE', #21976, .T. ) ;
#1177 = PLANE ( 'NONE',  #27529 ) ;
#1178 = DIRECTION ( 'NONE',  ( 0.000000000000000000, 0.000000000000000000, 1.000000000000000000 ) ) ;
#1179 = CARTESIAN_POINT ( 'NONE',  ( 10.37878353480403071, 20.06555603763842655, -22.52087948115185156 ) ) ;
#1180 = DIRECTION ( 'NONE',  ( 0.000000000000000000, 0.000000000000000000, 1.000000000000000000 ) ) ;
#1181 = AXIS2_PLACEMENT_3D ( 'NONE', #12643, #53, #25031 ) ;
#1182 = ORIENTED_EDGE ( 'NONE', *, *, #28357, .T. ) ;
#1183 = EDGE_CURVE ( 'NONE', #36822, #20981, #34308, .T. ) ;
#1185 = CARTESIAN_POINT ( 'NONE',  ( 3.503793317224327186, 8.420815634768674229, 7.000000000000000000 ) ) ;
#1184 = CARTESIAN_POINT ( 'NONE',  ( -16.84542159628621860, 11.77608213748940358, -28.29354725645489665 ) ) ;
#1186 = DIRECTION ( 'NONE',  ( -0.000000000000000000, -0.000000000000000000, -1.000000000000000000 ) ) ;
#1187 = CARTESIAN_POINT ( 'NONE',  ( 15.31617560365994812, -26.41030191234985125, -7.825682279171108924 ) ) ;
#1188 = CARTESIAN_POINT ( 'NONE',  ( -2.525645716490711123, 8.212903943950955465, 11.00000000000000000 ) ) ;
#1189 = CARTESIAN_POINT ( 'NONE',  ( 11.09563071542133450, 17.63336311864914663, -26.82764557179471510 ) ) ;
#1190 = AXIS2_PLACEMENT_3D ( 'NONE', #27894, #67, #9614 ) ;
#1191 = CARTESIAN_POINT ( 'NONE',  ( -19.69645987729884595, 11.37175641224115097, -29.99999999999998934 ) ) ;
#1192 = DIRECTION ( 'NONE',  ( 0.000000000000000000, 0.000000000000000000, 1.000000000000000000 ) ) ;
#1193 = AXIS2_PLACEMENT_3D ( 'NONE', #14848, #27235, #11798 ) ;
#1194 = CARTESIAN_POINT ( 'NONE',  ( -29.02322137993849438, -24.14915179229603837, -5.000000000000007994 ) ) ;
#1195 = CARTESIAN_POINT ( 'NONE',  ( 5.647652911981364099, -19.78961436050011713, -28.81940954220644713 ) ) ;
#1196 = CARTESIAN_POINT ( 'NONE',  ( 14.38725729136163345, 24.22873298939326148, -12.55976455580122675 ) ) ;
#1197 = CARTESIAN_POINT ( 'NONE',  ( 17.17189741702122063, 11.35564286007100065, -27.73265135103572376 ) ) ;
#1198 = DIRECTION ( 'NONE',  ( 1.000000000000000000, 0.000000000000000000, 0.000000000000000000 ) ) ;
#1199 = CARTESIAN_POINT ( 'NONE',  ( 11.94134295108989896, 16.18301270189217433, 10.00000000000000000 ) ) ;
#1201 = ORIENTED_EDGE ( 'NONE', *, *, #17627, .T. ) ;
#1200 = EDGE_CURVE ( 'NONE', #11801, #6957, #37554, .T. ) ;
#1202 = CARTESIAN_POINT ( 'NONE',  ( -6.727062190665558106, 25.26119790492828088, -18.80720107704606647 ) ) ;
#1203 = EDGE_CURVE ( 'NONE', #36455, #445, #34657, .T. ) ;
#1204 = EDGE_LOOP ( 'NONE', ( #35292, #7584, #15851, #28195 ) ) ;
#1205 = EDGE_CURVE ( 'NONE', #3451, #1436, #12018, .T. ) ;
#1206 = LINE ( 'NONE', #13990, #38384 ) ;
#1207 = ORIENTED_EDGE ( 'NONE', *, *, #7249, .F. ) ;
#1208 = CARTESIAN_POINT ( 'NONE',  ( 29.82425386686576019, 0.01900928345093852792, -9.708684470575656533 ) ) ;
#1209 = DIRECTION ( 'NONE',  ( 0.000000000000000000, 0.000000000000000000, 1.000000000000000000 ) ) ;
#1210 = CARTESIAN_POINT ( 'NONE',  ( -32.09165771328038375, 1.123514972298483405, 13.32518128616608344 ) ) ;
#1211 = ORIENTED_EDGE ( 'NONE', *, *, #23289, .F. ) ;
#1212 = CARTESIAN_POINT ( 'NONE',  ( -29.89861541276895451, 0.1309397030943943996, -9.240080585033846106 ) ) ;
#1213 = EDGE_LOOP ( 'NONE', ( #29735, #21723 ) ) ;
#1214 = CARTESIAN_POINT ( 'NONE',  ( 30.12854829685219826, -8.081545850541484555, -13.92922311047432693 ) ) ;
#1215 = CONICAL_SURFACE ( 'NONE', #13527, 1.000000000000002665, 0.7853981633974547183 ) ;
#1216 = AXIS2_PLACEMENT_3D ( 'NONE', #39023, #17309, #17711 ) ;
#1217 = ORIENTED_EDGE ( 'NONE', *, *, #3052, .T. ) ;
#1218 = CARTESIAN_POINT ( 'NONE',  ( 0.000000000000000000, 0.000000000000000000, 0.000000000000000000 ) ) ;
#1219 = CARTESIAN_POINT ( 'NONE',  ( 2.672146553953313131, 12.33340603770390764, 10.50000000000000000 ) ) ;
#1220 = CIRCLE ( 'NONE', #11606, 1.000000000000000000 ) ;
#1221 = DIRECTION ( 'NONE',  ( 0.000000000000000000, 0.000000000000000000, -1.000000000000000000 ) ) ;
#1222 = CARTESIAN_POINT ( 'NONE',  ( 8.910254037844365982, 17.93301270189218855, 10.50000000000000000 ) ) ;
#1223 = EDGE_CURVE ( 'NONE', #12698, #32913, #15840, .T. ) ;
#1224 = CARTESIAN_POINT ( 'NONE',  ( -7.430899969937648564, 32.27804933232874873, 19.27171037444156099 ) ) ;
#1225 = CARTESIAN_POINT ( 'NONE',  ( 0.5000000000000000000, 37.50000000000000711, 10.49999999999999822 ) ) ;
#1226 = EDGE_LOOP ( 'NONE', ( #7696, #31771 ) ) ;
#1227 = EDGE_CURVE ( 'NONE', #29281, #13694, #28202, .T. ) ;
#1228 = DIRECTION ( 'NONE',  ( 0.000000000000000000, 0.000000000000000000, 1.000000000000000000 ) ) ;
#1229 = FACE_OUTER_BOUND ( 'NONE', #33630, .T. ) ;
#1230 = CARTESIAN_POINT ( 'NONE',  ( 13.63581098909226874, 27.45627467658428955, 7.000000000000000000 ) ) ;
#1231 = CARTESIAN_POINT ( 'NONE',  ( 14.37745063133728962, 14.88579328056754392, -27.07234760961560838 ) ) ;
#1232 = CARTESIAN_POINT ( 'NONE',  ( 10.87246471302026585, 34.12433032489231977, -6.319560934679609332 ) ) ;
#1233 = ORIENTED_EDGE ( 'NONE', *, *, #26995, .F. ) ;
#1234 = CARTESIAN_POINT ( 'NONE',  ( 1.494936919103933226, 34.23777120880591696, 6.000000000000000000 ) ) ;
#1235 = LINE ( 'NONE', #22751, #18810 ) ;
#1236 = CARTESIAN_POINT ( 'NONE',  ( 11.20115890257327429, -19.37169324739840803, -22.64800607319368098 ) ) ;
#1237 = DIRECTION ( 'NONE',  ( 0.000000000000000000, 0.000000000000000000, 1.000000000000000000 ) ) ;
#1238 = DIRECTION ( 'NONE',  ( 0.9781476007338041345, -0.2079116908177664202, 0.000000000000000000 ) ) ;
#1239 = VECTOR ( 'NONE', #27661, 1000.000000000000000 ) ;
#1240 = ORIENTED_EDGE ( 'NONE', *, *, #8680, .T. ) ;
#1242 = VECTOR ( 'NONE', #27565, 1000.000000000000000 ) ;
#1241 = CARTESIAN_POINT ( 'NONE',  ( -12.14073867079856228, 19.91215881038760216, -20.54295507933877829 ) ) ;
#1243 = CARTESIAN_POINT ( 'NONE',  ( -20.67781403882173663, -27.68125770801090013, 15.72805884748939498 ) ) ;
#1244 = CARTESIAN_POINT ( 'NONE',  ( 10.56033047147009363, -20.05577440089765773, -21.65083658459305838 ) ) ;
#1245 = FACE_OUTER_BOUND ( 'NONE', #6644, .T. ) ;
#1246 = ORIENTED_EDGE ( 'NONE', *, *, #32743, .T. ) ;
#1247 = ORIENTED_EDGE ( 'NONE', *, *, #950, .T. ) ;
#1248 = AXIS2_PLACEMENT_3D ( 'NONE', #664, #24648, #15512 ) ;
#1249 = CARTESIAN_POINT ( 'NONE',  ( -12.16410700443224435, 28.43824891296100787, -12.25767132112050284 ) ) ;
#1250 = DIRECTION ( 'NONE',  ( -0.7032331762534058672, -0.07391278520355742954, -0.7071067811865467956 ) ) ;
#1251 = DIRECTION ( 'NONE',  ( 0.000000000000000000, 0.000000000000000000, 1.000000000000000000 ) ) ;
#1252 = CARTESIAN_POINT ( 'NONE',  ( -34.40806036129627898, -8.519187409710106351, -8.488083742945722321 ) ) ;
#1253 = LINE ( 'NONE', #10392, #32639 ) ;
#1254 = ORIENTED_EDGE ( 'NONE', *, *, #37582, .T. ) ;
#1255 = CARTESIAN_POINT ( 'NONE',  ( 30.57967879765778108, 0.1203670305863910467, -6.888307866855733153 ) ) ;
#1256 = CARTESIAN_POINT ( 'NONE',  ( 14.42035624161478857, 26.65972665747660031, 10.49999999999999822 ) ) ;
#1257 = DIRECTION ( 'NONE',  ( -0.1045284632676570929, -0.9945218953682730678, 0.000000000000000000 ) ) ;
#1258 = VERTEX_POINT ( 'NONE', #22299 ) ;
#1259 = CARTESIAN_POINT ( 'NONE',  ( -20.81612948364115567, 0.8239250655022540837, -26.83009370459933152 ) ) ;
#1260 = CARTESIAN_POINT ( 'NONE',  ( -30.53342463661827821, -27.99077457432856875, 11.00000000000000178 ) ) ;
#1261 = VERTEX_POINT ( 'NONE', #5321 ) ;
#1262 = CARTESIAN_POINT ( 'NONE',  ( 33.89061681622978028, -4.196143601155450931, -5.455404339117079004 ) ) ;
#1263 = DIRECTION ( 'NONE',  ( 0.1045284632676437842, -0.9945218953682742891, 0.000000000000000000 ) ) ;
#1264 = CARTESIAN_POINT ( 'NONE',  ( 32.49165476041698497, -0.9821698610445067645, 15.72805884749123351 ) ) ;
#1265 = ORIENTED_EDGE ( 'NONE', *, *, #18694, .F. ) ;
#1266 = CARTESIAN_POINT ( 'NONE',  ( -13.24632657851083550, 31.48533120267438079, 16.30093088680190050 ) ) ;
#1267 = CARTESIAN_POINT ( 'NONE',  ( -5.218261001347021200, -24.78318996519343997, 16.30093088680190760 ) ) ;
#1268 = DIRECTION ( 'NONE',  ( -1.000000000000000000, -1.224646799147351235E-16, 0.000000000000000000 ) ) ;
#1269 = CARTESIAN_POINT ( 'NONE',  ( 5.067518982750386591, 26.80212859219470189, 20.94377226548378346 ) ) ;
#1270 = AXIS2_PLACEMENT_3D ( 'NONE', #37696, #19009, #9864 ) ;
#1271 = DIRECTION ( 'NONE',  ( -1.000000000000000000, 0.000000000000000000, 0.000000000000000000 ) ) ;
#1272 = LINE ( 'NONE', #13655, #19517 ) ;
#1273 = CIRCLE ( 'NONE', #40184, 21.00000000000002842 ) ;
#1274 = PRODUCT_DEFINITION_SHAPE ( 'NONE', 'NONE',  #3314 ) ;
#1275 = DIRECTION ( 'NONE',  ( 0.000000000000000000, 0.000000000000000000, 1.000000000000000000 ) ) ;
#1276 = CARTESIAN_POINT ( 'NONE',  ( 19.49168883800135532, 11.25353179758032063, 18.42518152272108978 ) ) ;
#1277 = CARTESIAN_POINT ( 'NONE',  ( -23.34228009291333805, 8.898789006328664541, -8.395681560599031812 ) ) ;
#1278 = CARTESIAN_POINT ( 'NONE',  ( 12.77972917816506104, -16.04224856310990432, -29.99999999999998224 ) ) ;
#1279 = CARTESIAN_POINT ( 'NONE',  ( -13.29616015536805662, -18.15165799370312882, -30.00000000000000711 ) ) ;
#1280 = ORIENTED_EDGE ( 'NONE', *, *, #14981, .F. ) ;
#1281 = CARTESIAN_POINT ( 'NONE',  ( 12.04731220300567962, 20.02368371182513229, -20.52401430719184816 ) ) ;
#1282 = ORIENTED_EDGE ( 'NONE', *, *, #10347, .F. ) ;
#1283 = CARTESIAN_POINT ( 'NONE',  ( -14.05791702678590482, 21.72486893603357316, -15.52982955538085363 ) ) ;
#1284 = CARTESIAN_POINT ( 'NONE',  ( -29.14609120334281300, -6.569533100116839108, 19.99202127657103389 ) ) ;
#1285 = CARTESIAN_POINT ( 'NONE',  ( 10.44103466624280507, 32.57396620494213124, 10.99999999999999645 ) ) ;
#1286 = CARTESIAN_POINT ( 'NONE',  ( 12.44038979486233742, 20.42548900545279977, -19.50506954796185610 ) ) ;
#1287 = ORIENTED_EDGE ( 'NONE', *, *, #18070, .T. ) ;
#1288 = CARTESIAN_POINT ( 'NONE',  ( 17.94885553750267349, -9.904091770223047320, -29.21232500953899347 ) ) ;
#1289 = DIRECTION ( 'NONE',  ( 1.000000000000000000, 0.000000000000000000, 0.000000000000000000 ) ) ;
#1290 = VERTEX_POINT ( 'NONE', #17733 ) ;
#1292 = CARTESIAN_POINT ( 'NONE',  ( -11.11016527260153630, 31.83082137946488643, 7.000000000000000000 ) ) ;
#1291 = CARTESIAN_POINT ( 'NONE',  ( -13.60097212438034653, 23.76709706593192095, -14.43766431921598681 ) ) ;
#1293 = CARTESIAN_POINT ( 'NONE',  ( -9.617847002920147048, -18.10379274102027836, -30.00000000000000000 ) ) ;
#1294 = DIRECTION ( 'NONE',  ( -1.000000000000000000, 0.000000000000000000, 0.000000000000000000 ) ) ;
#1295 = VECTOR ( 'NONE', #26003, 1000.000000000000000 ) ;
#1296 = ORIENTED_EDGE ( 'NONE', *, *, #28654, .F. ) ;
#1297 = CARTESIAN_POINT ( 'NONE',  ( -19.30384401185921917, -8.002489564330206306, -26.99704546719047471 ) ) ;
#1298 = CARTESIAN_POINT ( 'NONE',  ( -9.169462346764058580, -18.33493501355543742, -30.00000000000000000 ) ) ;
#1299 = CARTESIAN_POINT ( 'NONE',  ( -22.37674264578614469, 24.85189042352228839, 7.000000000000000000 ) ) ;
#1300 = CARTESIAN_POINT ( 'NONE',  ( 14.17125917010577574, 17.46214553589771157, -20.85956934933411233 ) ) ;
#1301 = ORIENTED_EDGE ( 'NONE', *, *, #22155, .F. ) ;
#1302 = CARTESIAN_POINT ( 'NONE',  ( 27.36042259163830082, 3.779474170926635512, -6.428186719520351922 ) ) ;
#1303 = EDGE_CURVE ( 'NONE', #21971, #24685, #2677, .T. ) ;
#1304 = CARTESIAN_POINT ( 'NONE',  ( 5.187504188494417079, 36.60991850771481637, 11.00000000000000000 ) ) ;
#1305 = CARTESIAN_POINT ( 'NONE',  ( -33.75875814100331951, 2.759858869446532470, 23.00000000000000000 ) ) ;
#1306 = CONICAL_SURFACE ( 'NONE', #24006, 0.9999999999999970024, 0.7853981633974552734 ) ;
#1307 = ORIENTED_EDGE ( 'NONE', *, *, #32309, .T. ) ;
#1308 = CARTESIAN_POINT ( 'NONE',  ( -30.66527662088913075, -0.2016734898252389718, -7.819459957311872600 ) ) ;
#1309 = CARTESIAN_POINT ( 'NONE',  ( 31.16058696847114362, -0.7566004393934862016, -7.796922074218358922 ) ) ;
#1310 = ADVANCED_FACE ( 'NONE', ( #21162 ), #12761, .F. ) ;
#1311 = CARTESIAN_POINT ( 'NONE',  ( 28.87886971313727003, -7.891952902956772320, 20.25080042701540251 ) ) ;
#1312 = ORIENTED_EDGE ( 'NONE', *, *, #25393, .F. ) ;
#1313 = EDGE_CURVE ( 'NONE', #6680, #2398, #15203, .T. ) ;
#1314 = CARTESIAN_POINT ( 'NONE',  ( -11.10756861982300947, 19.59949212537556562, -29.99999999999999645 ) ) ;
#1315 = DIRECTION ( 'NONE',  ( 0.000000000000000000, 0.000000000000000000, 1.000000000000000000 ) ) ;
#1316 = CARTESIAN_POINT ( 'NONE',  ( 9.840690490415068936, 20.46019347195515792, 10.50000000000000533 ) ) ;
#1317 = CARTESIAN_POINT ( 'NONE',  ( 5.458865582155095986, 18.48521636184714012, 12.00000000000000000 ) ) ;
#1318 = CARTESIAN_POINT ( 'NONE',  ( -11.54426395383663539, 32.09594422634664568, 10.49999999999999822 ) ) ;
#1319 = CARTESIAN_POINT ( 'NONE',  ( 30.90412082983250741, -0.04211290444289944590, -5.000000000000000000 ) ) ;
#1320 = CARTESIAN_POINT ( 'NONE',  ( -0.9999999999999993339, 33.00000000000000000, 10.50000000000000178 ) ) ;
#1321 = ORIENTED_EDGE ( 'NONE', *, *, #36254, .F. ) ;
#1322 = ADVANCED_FACE ( 'NONE', ( #5718 ), #8061, .T. ) ;
#1323 = CARTESIAN_POINT ( 'NONE',  ( -6.546529844544896726, 35.97445010452243963, 10.68306085400114469 ) ) ;
#1324 = EDGE_CURVE ( 'NONE', #26783, #13841, #26857, .T. ) ;
#1325 = LINE ( 'NONE', #26511, #14257 ) ;
#1326 = CARTESIAN_POINT ( 'NONE',  ( 15.49469401537697877, -13.43643885346290645, -30.00000000000000000 ) ) ;
#1327 = PLANE ( 'NONE',  #6311 ) ;
#1328 = LINE ( 'NONE', #7615, #10590 ) ;
#1329 = CARTESIAN_POINT ( 'NONE',  ( 13.75857034051007588, 24.56595210210346636, -13.45474119376723188 ) ) ;
#1330 = DIRECTION ( 'NONE',  ( -1.000000000000000000, 0.000000000000000000, 0.000000000000000000 ) ) ;
#1331 = ORIENTED_EDGE ( 'NONE', *, *, #20700, .T. ) ;
#1332 = CARTESIAN_POINT ( 'NONE',  ( -14.93930595609077372, 14.05784520172980834, -30.00000000000002132 ) ) ;
#1333 = CARTESIAN_POINT ( 'NONE',  ( -24.38721429972438770, -12.23686305972948318, 20.99999999999999645 ) ) ;
#1334 = CARTESIAN_POINT ( 'NONE',  ( 9.515264969114221927, -18.30106724108619787, -28.08047306799037202 ) ) ;
#1335 = CARTESIAN_POINT ( 'NONE',  ( -19.48557158514998022, -11.24999999999982414, 23.00000000000000000 ) ) ;
#1336 = CARTESIAN_POINT ( 'NONE',  ( 15.02664410326935851, 25.94178776440897494, -9.238651380280199277 ) ) ;
#1337 = ORIENTED_EDGE ( 'NONE', *, *, #16216, .F. ) ;
#1338 = CARTESIAN_POINT ( 'NONE',  ( 15.09864989872857244, 26.14700263954316029, -8.767557201553991320 ) ) ;
#1339 = ORIENTED_EDGE ( 'NONE', *, *, #20945, .T. ) ;
#1341 = CARTESIAN_POINT ( 'NONE',  ( 14.31632963181209917, 26.62592636301939919, 10.82238861112333694 ) ) ;
#1340 = CARTESIAN_POINT ( 'NONE',  ( -14.70308516012370248, 25.50042804345432756, -10.64636925701135617 ) ) ;
#1342 = CARTESIAN_POINT ( 'NONE',  ( -14.31400716352764668, -25.06285765673995769, -11.60025332831071054 ) ) ;
#1343 = CARTESIAN_POINT ( 'NONE',  ( -16.87498849720621763, -29.16588574430760517, 11.55979286843870035 ) ) ;
#1344 = VECTOR ( 'NONE', #28491, 1000.000000000000000 ) ;
#1345 = CARTESIAN_POINT ( 'NONE',  ( -31.84658246857330965, -19.23773494732160572, -8.842712113036586885 ) ) ;
#1346 = CARTESIAN_POINT ( 'NONE',  ( -2.475031807174856713, -24.15412266750587023, -10.88196088067523881 ) ) ;
#1347 = CARTESIAN_POINT ( 'NONE',  ( 11.56847964180033728, 16.97430105090107233, -28.72963091288654169 ) ) ;
#1348 = ORIENTED_EDGE ( 'NONE', *, *, #957, .T. ) ;
#1349 = CARTESIAN_POINT ( 'NONE',  ( 22.28759716408703895, 8.923642387558418321, -12.86559102559659351 ) ) ;
#1350 = CIRCLE ( 'NONE', #6519, 1.000000000000000888 ) ;
#1351 = CARTESIAN_POINT ( 'NONE',  ( -37.48557158514991272, -11.24999999999982414, 23.00000000000000000 ) ) ;
#1352 = CARTESIAN_POINT ( 'NONE',  ( -10.15119711060580343, -25.59814205317665881, -4.999999999999997335 ) ) ;
#1353 = CARTESIAN_POINT ( 'NONE',  ( -1.621626408466260161, 37.48425883190013508, 17.42190598798392642 ) ) ;
#1354 = ORIENTED_EDGE ( 'NONE', *, *, #29827, .T. ) ;
#1355 = CARTESIAN_POINT ( 'NONE',  ( -20.87597923362057983, -1.832164627360789666, -26.62503287721647993 ) ) ;
#1356 = ADVANCED_FACE ( 'NONE', ( #5514 ), #24009, .F. ) ;
#1357 = CARTESIAN_POINT ( 'NONE',  ( -8.768078002824983841, 24.93711404285093991, 20.50957957746029336 ) ) ;
#1358 = EDGE_LOOP ( 'NONE', ( #33756, #22693 ) ) ;
#1359 = CARTESIAN_POINT ( 'NONE',  ( 24.08646667827959220, -13.28101593840520600, 20.99999999999999645 ) ) ;
#1360 = FACE_OUTER_BOUND ( 'NONE', #19909, .T. ) ;
#1361 = AXIS2_PLACEMENT_3D ( 'NONE', #24804, #28254, #12412 ) ;
#1362 = CARTESIAN_POINT ( 'NONE',  ( 1.485571585149874529, -11.25000000000009415, 3.000000000000000000 ) ) ;
#1363 = CARTESIAN_POINT ( 'NONE',  ( 21.69165369200475624, -9.527500816022886454, -21.87585738750458475 ) ) ;
#1364 = CARTESIAN_POINT ( 'NONE',  ( 32.80061120326785584, -23.42582577749432104, 12.14047268033107407 ) ) ;
#1365 = VERTEX_POINT ( 'NONE', #36801 ) ;
#1366 = CARTESIAN_POINT ( 'NONE',  ( -18.00000000000000000, 22.50000000000000355, 6.000000000000000000 ) ) ;
#1367 = LINE ( 'NONE', #10306, #8481 ) ;
#1368 = CIRCLE ( 'NONE', #31840, 0.5000000000000004441 ) ;
#1369 = DIRECTION ( 'NONE',  ( 0.5446390350150349668, 0.8386705679454188322, -7.903458058585596061E-16 ) ) ;
#1370 = ORIENTED_EDGE ( 'NONE', *, *, #15507, .T. ) ;
#1371 = CARTESIAN_POINT ( 'NONE',  ( -0.7505169017605982651, 38.27747495725317606, -6.696244658323041499 ) ) ;
#1372 = VECTOR ( 'NONE', #34789, 1000.000000000000114 ) ;
#1373 = CARTESIAN_POINT ( 'NONE',  ( -14.97840499040354878, 21.69233280637162053, 7.455539900862802050 ) ) ;
#1374 = ADVANCED_FACE ( 'NONE', ( #22106 ), #9347, .T. ) ;
#1375 = CARTESIAN_POINT ( 'NONE',  ( 17.34253826607195847, 27.32041144403996569, 11.55979286843935405 ) ) ;
#1376 = EDGE_CURVE ( 'NONE', #18785, #40077, #26215, .T. ) ;
#1377 = LINE ( 'NONE', #35710, #25357 ) ;
#1378 = CARTESIAN_POINT ( 'NONE',  ( -14.47283171447380390, 21.48159823030330529, 11.00000000000000000 ) ) ;
#1379 = CYLINDRICAL_SURFACE ( 'NONE', #11271, 0.4999999999999999445 ) ;
#1380 = CARTESIAN_POINT ( 'NONE',  ( 11.86081488739372958, 24.33169448125006795, -16.19729836796659939 ) ) ;
#1381 = CARTESIAN_POINT ( 'NONE',  ( 10.10646936306337729, 32.94553861768082470, 9.500000000000000000 ) ) ;
#1382 = EDGE_LOOP ( 'NONE', ( #25850, #30866, #28267, #16850 ) ) ;
#1384 = CARTESIAN_POINT ( 'NONE',  ( -4.118678732975735279, 7.827785988993307242, 6.000000000000000000 ) ) ;
#1383 = CARTESIAN_POINT ( 'NONE',  ( -17.39430208471609163, 11.24351447107411772, -26.62001118384078779 ) ) ;
#1385 = CARTESIAN_POINT ( 'NONE',  ( -0.5934445985556291436, 37.50000000000000711, 10.49999999999999822 ) ) ;
#1386 = CARTESIAN_POINT ( 'NONE',  ( 9.770751854196934261, -18.40326536504920796, -26.82356556862325547 ) ) ;
#1387 = AXIS2_PLACEMENT_3D ( 'NONE', #12365, #28398, #31452 ) ;
#1388 = CARTESIAN_POINT ( 'NONE',  ( 15.32336983265158281, 26.66990810724929872, -6.886851398718627948 ) ) ;
#1389 = CARTESIAN_POINT ( 'NONE',  ( 4.336808689942017736E-15, 40.84107189184581443, -5.000000000000008882 ) ) ;
#1390 = CARTESIAN_POINT ( 'NONE',  ( -4.987329993433320396E-14, 13.65543219052647927, 7.000000000000000000 ) ) ;
#1391 = CARTESIAN_POINT ( 'NONE',  ( -16.43502440684527599, -14.51438213871383454, -24.33132401675261747 ) ) ;
#1392 = CARTESIAN_POINT ( 'NONE',  ( 5.635282026549600864, -19.76630616200782242, -29.40695735224786844 ) ) ;
#1393 = CARTESIAN_POINT ( 'NONE',  ( 15.52561063650128759, 26.30458316266247110, -5.946179686823199972 ) ) ;
#1394 = CARTESIAN_POINT ( 'NONE',  ( 18.66890321014120246, 12.51461972714008652, -18.00895683570465522 ) ) ;
#1395 = CARTESIAN_POINT ( 'NONE',  ( 4.727507481117209309, 31.88885898370940453, 10.00000000000000000 ) ) ;
#1396 = CYLINDRICAL_SURFACE ( 'NONE', #2758, 1.000000000000000000 ) ;
#1397 = ORIENTED_EDGE ( 'NONE', *, *, #13984, .F. ) ;
#1398 = CARTESIAN_POINT ( 'NONE',  ( -8.453943144716905778, 36.13191751627968529, -5.000000000000000888 ) ) ;
#1399 = ORIENTED_EDGE ( 'NONE', *, *, #30628, .F. ) ;
#1400 = ADVANCED_FACE ( 'NONE', ( #16413 ), #35301, .F. ) ;
#1401 = CARTESIAN_POINT ( 'NONE',  ( -11.40809387606930336, -20.99419242044788803, -19.51149134545002184 ) ) ;
#1402 = AXIS2_PLACEMENT_3D ( 'NONE', #9572, #21954, #28251 ) ;
#1403 = DIRECTION ( 'NONE',  ( -0.000000000000000000, -0.000000000000000000, -1.000000000000000000 ) ) ;
#1404 = VERTEX_POINT ( 'NONE', #3817 ) ;
#1405 = VECTOR ( 'NONE', #33314, 1000.000000000000000 ) ;
#1406 = DIRECTION ( 'NONE',  ( 1.000000000000000000, 0.000000000000000000, 0.000000000000000000 ) ) ;
#1407 = EDGE_CURVE ( 'NONE', #37972, #16754, #31408, .T. ) ;
#1408 = CARTESIAN_POINT ( 'NONE',  ( -32.28722999652026004, 1.315479119632481098, 12.14047268033097637 ) ) ;
#1409 = ORIENTED_EDGE ( 'NONE', *, *, #22300, .F. ) ;
#1410 = CARTESIAN_POINT ( 'NONE',  ( -30.38029091318623642, 0.09813233376897281812, -7.828559720627486840 ) ) ;
#1411 = ORIENTED_EDGE ( 'NONE', *, *, #18184, .T. ) ;
#1412 = CARTESIAN_POINT ( 'NONE',  ( 34.90301088146017605, -9.422820822732527191, -7.602032696592240235 ) ) ;
#1413 = EDGE_CURVE ( 'NONE', #14680, #20195, #33151, .T. ) ;
#1414 = ORIENTED_EDGE ( 'NONE', *, *, #34847, .F. ) ;
#1415 = DIRECTION ( 'NONE',  ( 1.000000000000000000, 0.000000000000000000, 0.000000000000000000 ) ) ;
#1416 = AXIS2_PLACEMENT_3D ( 'NONE', #32542, #2255, #4697 ) ;
#1417 = CARTESIAN_POINT ( 'NONE',  ( -1.947644445291408566, 40.50000000000003553, 10.99999999999999822 ) ) ;
#1418 = LINE ( 'NONE', #29444, #27453 ) ;
#1419 = CARTESIAN_POINT ( 'NONE',  ( 11.14716901145161643, 12.46304090461738667, 12.00000000000000000 ) ) ;
#1420 = CARTESIAN_POINT ( 'NONE',  ( 13.22866120778972210, 26.17694675929306314, 18.42518152272108622 ) ) ;
#1421 = PLANE ( 'NONE',  #23980 ) ;
#1422 = ORIENTED_EDGE ( 'NONE', *, *, #35439, .T. ) ;
#1423 = LINE ( 'NONE', #23757, #26238 ) ;
#1424 = CARTESIAN_POINT ( 'NONE',  ( -2.629601561899595374, 7.723830143584053509, 10.49999999999999822 ) ) ;
#1425 = EDGE_CURVE ( 'NONE', #29377, #5003, #4219, .T. ) ;
#1426 = LINE ( 'NONE', #13808, #32490 ) ;
#1427 = EDGE_CURVE ( 'NONE', #25178, #38914, #38549, .T. ) ;
#1428 = CARTESIAN_POINT ( 'NONE',  ( 17.57999905932629048, 16.66487347840518041, -13.82914334805849421 ) ) ;
#1429 = CARTESIAN_POINT ( 'NONE',  ( 10.76909278579559981, 33.72652210473967926, -7.628981730212053947 ) ) ;
#1430 = ORIENTED_EDGE ( 'NONE', *, *, #13824, .F. ) ;
#1431 = CARTESIAN_POINT ( 'NONE',  ( 6.354454053420414361, 35.54304081427980577, 7.000000000000000000 ) ) ;
#1432 = CARTESIAN_POINT ( 'NONE',  ( -2.063787492809998625, 7.980908877017413694, 10.49999999999999645 ) ) ;
#1433 = CARTESIAN_POINT ( 'NONE',  ( 16.42748648437301640, -26.82053992255703889, -6.866534988705063292 ) ) ;
#1434 = FACE_BOUND ( 'NONE', #30961, .T. ) ;
#1435 = DIRECTION ( 'NONE',  ( 1.000000000000000000, 0.000000000000000000, 0.000000000000000000 ) ) ;
#1436 = VERTEX_POINT ( 'NONE', #32050 ) ;
#1437 = CARTESIAN_POINT ( 'NONE',  ( -10.98473797697927701, 17.30853926952405075, -29.34836101394438401 ) ) ;
#1438 = CARTESIAN_POINT ( 'NONE',  ( -18.89970378041276788, -27.81027634888826938, 15.72805884748982130 ) ) ;
#1439 = CARTESIAN_POINT ( 'NONE',  ( 14.86825508979877064, -26.56089389575996407, -5.946233135902982525 ) ) ;
#1440 = DIRECTION ( 'NONE',  ( -0.000000000000000000, -0.000000000000000000, -1.000000000000000000 ) ) ;
#1441 = ORIENTED_EDGE ( 'NONE', *, *, #32902, .F. ) ;
#1442 = ORIENTED_EDGE ( 'NONE', *, *, #468, .T. ) ;
#1443 = CARTESIAN_POINT ( 'NONE',  ( -13.13940279579264825, 30.96237069512062590, -7.695636096163062767 ) ) ;
#1444 = DIRECTION ( 'NONE',  ( 0.000000000000000000, 0.000000000000000000, 1.000000000000000000 ) ) ;
#1445 = EDGE_CURVE ( 'NONE', #11176, #10038, #11957, .T. ) ;
#1446 = CARTESIAN_POINT ( 'NONE',  ( -12.74038105676665111, 14.56698729810790027, 10.49999999999999822 ) ) ;
#1447 = CIRCLE ( 'NONE', #22192, 0.4999999999999997780 ) ;
#1448 = CARTESIAN_POINT ( 'NONE',  ( -33.37315695507471958, -7.245599113437738659, -9.850161829985118800 ) ) ;
#1449 = LINE ( 'NONE', #8349, #28663 ) ;
#1450 = VERTEX_POINT ( 'NONE', #28600 ) ;
#1451 = CARTESIAN_POINT ( 'NONE',  ( 27.60362641570377207, 0.3697951749082440953, -13.52364084678252887 ) ) ;
#1452 = EDGE_CURVE ( 'NONE', #21094, #16360, #1581, .T. ) ;
#1453 = DIRECTION ( 'NONE',  ( 0.000000000000000000, 0.000000000000000000, 1.000000000000000000 ) ) ;
#1454 = CARTESIAN_POINT ( 'NONE',  ( 4.724371395536106633, 32.23037938972932892, 6.000000000000000000 ) ) ;
#1455 = LINE ( 'NONE', #16903, #16082 ) ;
#1456 = ORIENTED_EDGE ( 'NONE', *, *, #37296, .T. ) ;
#1457 = CARTESIAN_POINT ( 'NONE',  ( -28.35170116396216144, 0.1243089573432585720, -12.54891019634939298 ) ) ;
#1458 = DIRECTION ( 'NONE',  ( 0.9781476007338072431, 0.2079116908177516265, 0.000000000000000000 ) ) ;
#1459 = ORIENTED_EDGE ( 'NONE', *, *, #16258, .F. ) ;
#1460 = CARTESIAN_POINT ( 'NONE',  ( 23.33064708864463555, -1.963756010919469830, -21.28980525675968849 ) ) ;
#1461 = EDGE_CURVE ( 'NONE', #11801, #13694, #16826, .T. ) ;
#1462 = CARTESIAN_POINT ( 'NONE',  ( 12.92776996871492479, 15.91343586356105533, -30.00000000000001421 ) ) ;
#1463 = AXIS2_PLACEMENT_3D ( 'NONE', #33377, #21369, #3079 ) ;
#1464 = CARTESIAN_POINT ( 'NONE',  ( 29.26100170765755948, -25.10377279866101929, 15.13084544680181942 ) ) ;
#1465 = EDGE_LOOP ( 'NONE', ( #32543, #28517, #29952, #26022 ) ) ;
#1466 = CARTESIAN_POINT ( 'NONE',  ( 6.948689594652316615, 37.54332414141804719, 15.72805884748934169 ) ) ;
#1467 = CARTESIAN_POINT ( 'NONE',  ( 4.318754312355916755E-14, -23.13411080437162326, 17.92354375535250810 ) ) ;
#1468 = CARTESIAN_POINT ( 'NONE',  ( 16.00000000000000000, 22.50000000000000355, 12.00000000000000000 ) ) ;
#1469 = CARTESIAN_POINT ( 'NONE',  ( 8.768078002822827344, 24.93711404285870614, 20.50957957746029692 ) ) ;
#1470 = PLANE ( 'NONE',  #5767 ) ;
#1471 = AXIS2_PLACEMENT_3D ( 'NONE', #39229, #2264, #14653 ) ;
#1472 = CARTESIAN_POINT ( 'NONE',  ( 7.312035131040564906, 19.41226734497195849, 6.000000000000000000 ) ) ;
#1473 = ADVANCED_FACE ( 'NONE', ( #4012 ), #1177, .T. ) ;
#1474 = ADVANCED_FACE ( 'NONE', ( #4625 ), #17026, .F. ) ;
#1475 = CARTESIAN_POINT ( 'NONE',  ( 4.832435196289363688, 29.43795123185613249, -15.73446877130611377 ) ) ;
#1476 = CIRCLE ( 'NONE', #24180, 1.000000000000000888 ) ;
#1477 = CARTESIAN_POINT ( 'NONE',  ( -10.36702044712415116, 31.16169077310601310, 7.000000000000000000 ) ) ;
#1478 = CARTESIAN_POINT ( 'NONE',  ( 24.95394407858722374, 1.780357051442290839, 18.87996532026972218 ) ) ;
#1479 = CARTESIAN_POINT ( 'NONE',  ( -20.87744296876565286, 11.29336303379088235, -12.88788702006255349 ) ) ;
#1480 = CARTESIAN_POINT ( 'NONE',  ( 18.22149445818437385, -22.61346887214493862, -15.02646902325029643 ) ) ;
#1481 = LINE ( 'NONE', #13868, #13224 ) ;
#1482 = CARTESIAN_POINT ( 'NONE',  ( -33.63536641588170539, -18.98279099655679758, -4.999999999999999112 ) ) ;
#1483 = CARTESIAN_POINT ( 'NONE',  ( 15.38842093998857230, 26.88136989284191003, -5.000000000000000000 ) ) ;
#1484 = EDGE_LOOP ( 'NONE', ( #15281, #34654, #5534 ) ) ;
#1485 = CARTESIAN_POINT ( 'NONE',  ( -12.44742484898385904, 17.58201857736815299, -23.99274416867952553 ) ) ;
#1486 = CARTESIAN_POINT ( 'NONE',  ( -31.78757023779102298, -12.37085478034622810, 19.27171037444157875 ) ) ;
#1487 = LINE ( 'NONE', #23625, #21790 ) ;
#1488 = CARTESIAN_POINT ( 'NONE',  ( 11.16523723692197478, 17.58493466368048530, -26.83415995730371506 ) ) ;
#1489 = VERTEX_POINT ( 'NONE', #28801 ) ;
#1490 = CARTESIAN_POINT ( 'NONE',  ( 32.80703094730063185, -16.80140863343335766, -9.283588785457341785 ) ) ;
#1491 = ORIENTED_EDGE ( 'NONE', *, *, #37103, .T. ) ;
#1493 = DIRECTION ( 'NONE',  ( 1.000000000000000000, 0.000000000000000000, 0.000000000000000000 ) ) ;
#1492 = CARTESIAN_POINT ( 'NONE',  ( -12.24516985351738718, 20.68376759742653093, -19.46578503039011210 ) ) ;
#1494 = CARTESIAN_POINT ( 'NONE',  ( -16.22334360803714404, -26.92298677526160233, -5.000000000000000888 ) ) ;
#1495 = DIRECTION ( 'NONE',  ( 0.000000000000000000, 0.000000000000000000, 1.000000000000000000 ) ) ;
#1496 = VECTOR ( 'NONE', #9423, 1000.000000000000114 ) ;
#1497 = ORIENTED_EDGE ( 'NONE', *, *, #11640, .F. ) ;
#1498 = CARTESIAN_POINT ( 'NONE',  ( -26.43177126521426956, -11.85372628369261250, -16.64861771188786221 ) ) ;
#1499 = CARTESIAN_POINT ( 'NONE',  ( -11.10430509875484084, -21.03298634457605232, -19.54320612427354931 ) ) ;
#1500 = CARTESIAN_POINT ( 'NONE',  ( 34.33271597229073535, -24.82403720151181759, 23.00000000000093792 ) ) ;
#1501 = CARTESIAN_POINT ( 'NONE',  ( 17.03376377104290640, 20.70341664989160435, -8.831506936632600002 ) ) ;
#1502 = ORIENTED_EDGE ( 'NONE', *, *, #26343, .T. ) ;
#1503 = CARTESIAN_POINT ( 'NONE',  ( 20.24413271415620841, 3.804288779818567612, -28.19920182012378973 ) ) ;
#1504 = ADVANCED_FACE ( 'NONE', ( #978 ), #10721, .F. ) ;
#1505 = CARTESIAN_POINT ( 'NONE',  ( 11.44134295108988830, 15.31698729810772974, 7.000000000000000000 ) ) ;
#1506 = LINE ( 'NONE', #19583, #6950 ) ;
#1507 = EDGE_LOOP ( 'NONE', ( #5685, #4941, #29383, #39119 ) ) ;
#1508 = CARTESIAN_POINT ( 'NONE',  ( -29.12724189388964291, -0.1775561609936863183, -11.57335334406140426 ) ) ;
#1509 = CARTESIAN_POINT ( 'NONE',  ( 30.44880780573000933, -0.6958124801958616157, -9.659808045383314834 ) ) ;
#1510 = CIRCLE ( 'NONE', #865, 0.9999999999999974465 ) ;
#1511 = CARTESIAN_POINT ( 'NONE',  ( 32.25947621352486294, -13.82181017473358331, 18.87996532025784546 ) ) ;
#1512 = ORIENTED_EDGE ( 'NONE', *, *, #23760, .T. ) ;
#1513 = CARTESIAN_POINT ( 'NONE',  ( -28.42036332966587509, 2.623993810986071651, -5.474604813331526820 ) ) ;
#1514 = CARTESIAN_POINT ( 'NONE',  ( 11.31392148919589680, 36.91540483778863546, -14.26382729546508088 ) ) ;
#1515 = AXIS2_PLACEMENT_3D ( 'NONE', #23057, #32207, #34854 ) ;
#1516 = CARTESIAN_POINT ( 'NONE',  ( 0.8712018466506370462, 31.30332840660451765, 12.00000000000000000 ) ) ;
#1517 = CIRCLE ( 'NONE', #10593, 0.4999999999999995559 ) ;
#1518 = CARTESIAN_POINT ( 'NONE',  ( -7.688306800005769048, 28.52217545723006609, 12.00000000000000000 ) ) ;
#1519 = CIRCLE ( 'NONE', #11910, 1.000000000000000000 ) ;
#1520 = DIRECTION ( 'NONE',  ( 0.000000000000000000, 0.000000000000000000, 1.000000000000000000 ) ) ;
#1521 = CARTESIAN_POINT ( 'NONE',  ( -15.15015520025801443, 37.49267296096588353, 9.500000000000000000 ) ) ;
#1522 = CARTESIAN_POINT ( 'NONE',  ( 13.24038105676655164, 15.43301270189216368, 10.49999999999999822 ) ) ;
#1523 = EDGE_CURVE ( 'NONE', #36376, #3606, #10317, .T. ) ;
#1524 = EDGE_LOOP ( 'NONE', ( #13086, #5976, #3796, #38278, #10393 ) ) ;
#1525 = CARTESIAN_POINT ( 'NONE',  ( -9.183247089818959097, 16.78440424842446532, 12.00000000000000000 ) ) ;
#1526 = AXIS2_PLACEMENT_3D ( 'NONE', #35749, #32090, #7292 ) ;
#1527 = DIRECTION ( 'NONE',  ( 1.000000000000000000, 0.000000000000000000, 0.000000000000000000 ) ) ;
#1528 = CARTESIAN_POINT ( 'NONE',  ( 27.06419666510200273, -24.97747390337942619, -7.153125932697236067 ) ) ;
#1529 = EDGE_CURVE ( 'NONE', #14246, #20723, #19724, .T. ) ;
#1530 = CARTESIAN_POINT ( 'NONE',  ( 14.49848586288626429, 20.47339359108930879, 11.00000000000000000 ) ) ;
#1531 = CARTESIAN_POINT ( 'NONE',  ( 14.64210930126480115, 24.20081211342298744, 6.000000000000000000 ) ) ;
#1532 = CARTESIAN_POINT ( 'NONE',  ( 10.61561400868404093, 17.69690613582448080, -28.05214642998929619 ) ) ;
#1533 = CARTESIAN_POINT ( 'NONE',  ( 10.09822582592851603, -27.41751403068707660, 11.00000000000204814 ) ) ;
#1534 = ORIENTED_EDGE ( 'NONE', *, *, #21059, .F. ) ;
#1535 = CIRCLE ( 'NONE', #24899, 1.000000000000000000 ) ;
#1536 = CARTESIAN_POINT ( 'NONE',  ( -16.97888402983207001, 18.46751920095590194, -12.77518134462292920 ) ) ;
#1537 = CARTESIAN_POINT ( 'NONE',  ( -21.42047163595255910, -15.86044052053618003, 20.99999999999999645 ) ) ;
#1538 = CARTESIAN_POINT ( 'NONE',  ( 11.46880063084097578, -20.98643766582429393, -19.50507162110192638 ) ) ;
#1539 = ADVANCED_FACE ( 'NONE', ( #34700 ), #6853, .F. ) ;
#1540 = PLANE ( 'NONE',  #21107 ) ;
#1541 = CARTESIAN_POINT ( 'NONE',  ( 15.02941416159078791, 25.93298973513185146, -9.238761048664686726 ) ) ;
#1542 = ORIENTED_EDGE ( 'NONE', *, *, #12015, .F. ) ;
#1543 = CARTESIAN_POINT ( 'NONE',  ( 15.39919595897972826, 26.75075905497473627, -5.946079338151666782 ) ) ;
#1544 = ORIENTED_EDGE ( 'NONE', *, *, #26999, .T. ) ;
#1546 = CARTESIAN_POINT ( 'NONE',  ( 14.17145697063259391, 26.57885438195654970, 10.94387467463490538 ) ) ;
#1545 = CARTESIAN_POINT ( 'NONE',  ( -13.99993087335245256, 24.00799898784267583, -13.50638822794025629 ) ) ;
#1547 = CARTESIAN_POINT ( 'NONE',  ( -9.487969581998370927, -18.17220041443854583, -29.34855226819949081 ) ) ;
#1548 = CARTESIAN_POINT ( 'NONE',  ( -29.92393930196035612, -26.04303208588115126, 11.55979286843952103 ) ) ;
#1549 = CARTESIAN_POINT ( 'NONE',  ( -19.95015686455310799, -12.87654000693452083, -21.84574686077818484 ) ) ;
#1550 = CIRCLE ( 'NONE', #15810, 0.5000000000000000000 ) ;
#1551 = CARTESIAN_POINT ( 'NONE',  ( -6.273692019901858430, -19.88452076598854745, -26.48636925569244127 ) ) ;
#1552 = CARTESIAN_POINT ( 'NONE',  ( 11.77204130854469000, 17.01331900727792856, -27.49973913441361972 ) ) ;
#1553 = VERTEX_POINT ( 'NONE', #25546 ) ;
#1554 = CARTESIAN_POINT ( 'NONE',  ( 21.35817030649165105, 7.746940167569142943, -17.95549415092490975 ) ) ;
#1555 = CARTESIAN_POINT ( 'NONE',  ( 8.559505275947156377, 25.28115294937476065, 12.00000000000000000 ) ) ;
#1556 = CARTESIAN_POINT ( 'NONE',  ( -11.19134295108999311, 14.88397459621566554, 10.50000000000000000 ) ) ;
#1557 = DIRECTION ( 'NONE',  ( 1.000000000000000000, 0.000000000000000000, 0.000000000000000000 ) ) ;
#1558 = EDGE_LOOP ( 'NONE', ( #20598, #31967, #32905, #25702 ) ) ;
#1559 = CARTESIAN_POINT ( 'NONE',  ( -25.18061870383569811, -0.9857286467851488210, -18.27162094256875591 ) ) ;
#1560 = AXIS2_PLACEMENT_3D ( 'NONE', #4826, #17232, #29608 ) ;
#1561 = CARTESIAN_POINT ( 'NONE',  ( -19.99288511733821139, -2.332377806177347690, 20.94377226548488125 ) ) ;
#1562 = EDGE_LOOP ( 'NONE', ( #30202, #37119, #17318, #13317 ) ) ;
#1563 = CARTESIAN_POINT ( 'NONE',  ( 23.10579450714144301, -17.79557859931273356, 20.82122704794064916 ) ) ;
#1564 = CARTESIAN_POINT ( 'NONE',  ( -8.577547685840080760, 11.84256962714647798, 6.000000000000000000 ) ) ;
#1565 = EDGE_CURVE ( 'NONE', #37722, #22206, #24914, .T. ) ;
#1566 = SURFACE_STYLE_FILL_AREA ( #8256 ) ;
#1567 = CARTESIAN_POINT ( 'NONE',  ( 18.88476749628562246, -8.988548275649279162, -26.97612708522287761 ) ) ;
#1568 = CARTESIAN_POINT ( 'NONE',  ( 36.55626306615705090, -16.65168930787738688, 12.73282698324840823 ) ) ;
#1569 = AXIS2_PLACEMENT_3D ( 'NONE', #19000, #31392, #18413 ) ;
#1570 = VERTEX_POINT ( 'NONE', #22899 ) ;
#1571 = CARTESIAN_POINT ( 'NONE',  ( -21.94497077913238314, 33.50980436007203878, 9.500000000000000000 ) ) ;
#1572 = DIRECTION ( 'NONE',  ( -0.000000000000000000, -0.000000000000000000, -1.000000000000000000 ) ) ;
#1573 = CARTESIAN_POINT ( 'NONE',  ( 7.577540944421576441, 33.15743037285414374, 6.000000000000000000 ) ) ;
#1574 = EDGE_LOOP ( 'NONE', ( #25578, #22925, #37462, #6000 ) ) ;
#1575 = CARTESIAN_POINT ( 'NONE',  ( -0.4624081962452046834, 23.76772061069408792, -21.83626832166117282 ) ) ;
#1576 = DIRECTION ( 'NONE',  ( 1.000000000000000000, 0.000000000000000000, 0.000000000000000000 ) ) ;
#1577 = EDGE_CURVE ( 'NONE', #32176, #28480, #7460, .T. ) ;
#1578 = DIRECTION ( 'NONE',  ( 0.6724985119639580455, -0.2185080122244185408, -0.7071067811865444641 ) ) ;
#1579 = DIRECTION ( 'NONE',  ( -0.7071067811865474617, 0.000000000000000000, -0.7071067811865474617 ) ) ;
#1581 = LINE ( 'NONE', #23108, #4820 ) ;
#1580 = PRODUCT_DEFINITION ( 'UNKNOWN', '', #13877, #24826 ) ;
#1582 = CARTESIAN_POINT ( 'NONE',  ( -14.26585111513660031, 17.86474508437623143, 6.000000000000000000 ) ) ;
#1583 = AXIS2_PLACEMENT_3D ( 'NONE', #2088, #14468, #37006 ) ;
#1584 = CARTESIAN_POINT ( 'NONE',  ( 12.73726530754508701, 25.36863251623071491, -14.28276732290829898 ) ) ;
#1585 = CARTESIAN_POINT ( 'NONE',  ( -13.37378135583788286, 20.59160479820268108, 10.00000000000000000 ) ) ;
#1586 = VERTEX_POINT ( 'NONE', #2586 ) ;
#1588 = FACE_OUTER_BOUND ( 'NONE', #22780, .T. ) ;
#1587 = CARTESIAN_POINT ( 'NONE',  ( -20.06818878704502751, 14.54951294394186689, -7.913531450302784265 ) ) ;
#1589 = EDGE_CURVE ( 'NONE', #2436, #14685, #14573, .T. ) ;
#1590 = DIRECTION ( 'NONE',  ( 0.000000000000000000, 0.000000000000000000, 1.000000000000000000 ) ) ;
#1591 = CARTESIAN_POINT ( 'NONE',  ( 15.44320054554677846, -26.65646054649087660, -6.416728767745834894 ) ) ;
#1592 = EDGE_CURVE ( 'NONE', #35323, #33546, #6114, .T. ) ;
#1593 = CARTESIAN_POINT ( 'NONE',  ( -5.947717410344456113, 34.62949535663729250, 9.500000000000000000 ) ) ;
#1594 = CARTESIAN_POINT ( 'NONE',  ( 13.75002412159893694, 23.44003394427787512, -14.47165457257529653 ) ) ;
#1595 = CARTESIAN_POINT ( 'NONE',  ( -27.08779848459120743, 7.221796966026712283, -13.42901749168596481 ) ) ;
#1596 = DIRECTION ( 'NONE',  ( -1.000000000000000000, 0.000000000000000000, 0.000000000000000000 ) ) ;
#1597 = AXIS2_PLACEMENT_3D ( 'NONE', #38393, #1228, #29449 ) ;
#1598 = CARTESIAN_POINT ( 'NONE',  ( -15.21888313924808855, -14.28223729339822157, -27.05990642766832721 ) ) ;
#1599 = CARTESIAN_POINT ( 'NONE',  ( 3.973911541953894400, -24.68614102020093881, -7.909360114664225172 ) ) ;
#1600 = CARTESIAN_POINT ( 'NONE',  ( 12.57937835649980052, 20.24290211102249160, -19.52900479813045465 ) ) ;
#1601 = CARTESIAN_POINT ( 'NONE',  ( 18.03593615372940917, 12.02637506715544724, -21.17004988786488084 ) ) ;
#1602 = CARTESIAN_POINT ( 'NONE',  ( -8.183247089818959097, 16.78440424842446532, 6.000000000000000000 ) ) ;
#1603 = ORIENTED_EDGE ( 'NONE', *, *, #27527, .F. ) ;
#1604 = CARTESIAN_POINT ( 'NONE',  ( -4.144713709954233494, 20.47503900711864588, -27.03594048031756358 ) ) ;
#1605 = ORIENTED_EDGE ( 'NONE', *, *, #26621, .T. ) ;
#1606 = DIRECTION ( 'NONE',  ( 0.1045284632676566766, 0.9945218953682730678, 0.000000000000000000 ) ) ;
#1607 = ORIENTED_EDGE ( 'NONE', *, *, #31486, .F. ) ;
#1608 = FACE_OUTER_BOUND ( 'NONE', #23351, .T. ) ;
#1609 = ADVANCED_FACE ( 'NONE', ( #26963 ), #20476, .T. ) ;
#1610 = DIRECTION ( 'NONE',  ( 0.000000000000000000, 0.000000000000000000, 1.000000000000000000 ) ) ;
#1611 = EDGE_CURVE ( 'NONE', #22260, #113, #18363, .T. ) ;
#1612 = EDGE_LOOP ( 'NONE', ( #18659, #38492 ) ) ;
#1613 = CARTESIAN_POINT ( 'NONE',  ( -20.96534858468971407, 0.8490077867318273075, -26.22846716918471799 ) ) ;
#1614 = VERTEX_POINT ( 'NONE', #23318 ) ;
#1615 = CARTESIAN_POINT ( 'NONE',  ( 21.10173320963569310, -5.688633216797759573, -24.40913811835638114 ) ) ;
#1616 = CIRCLE ( 'NONE', #27560, 0.5000000000000004441 ) ;
#1617 = EDGE_LOOP ( 'NONE', ( #6826, #36816, #20076, #26907 ) ) ;
#1618 = CARTESIAN_POINT ( 'NONE',  ( 0.000000000000000000, 0.000000000000000000, 0.000000000000000000 ) ) ;
#1619 = CARTESIAN_POINT ( 'NONE',  ( 6.330070799514983193, 27.28854476845134513, 13.00000000000000178 ) ) ;
#1620 = ORIENTED_EDGE ( 'NONE', *, *, #28007, .T. ) ;
#1621 = DIRECTION ( 'NONE',  ( 0.000000000000000000, 0.000000000000000000, 1.000000000000000000 ) ) ;
#1622 = AXIS2_PLACEMENT_3D ( 'NONE', #1740, #25900, #10676 ) ;
#1623 = CARTESIAN_POINT ( 'NONE',  ( -9.831584923911586671, 26.22020669908462764, 10.50000000000000000 ) ) ;
#1624 =( BOUNDED_CURVE ( )  B_SPLINE_CURVE ( 2, ( #20187, #30129, #14483 ),
 .UNSPECIFIED., .F., .F. ) 
 B_SPLINE_CURVE_WITH_KNOTS ( ( 3, 3 ),
 ( 0.000000000000000000, 1.000000000000000000 ),
 .UNSPECIFIED. ) 
 CURVE ( )  GEOMETRIC_REPRESENTATION_ITEM ( )  RATIONAL_B_SPLINE_CURVE ( ( 1.000000000000000000, 0.7071067811865474617, 1.000000000000000000 ) ) 
 REPRESENTATION_ITEM ( '' )  );
#1625 = CARTESIAN_POINT ( 'NONE',  ( 9.924110812760721601, 32.99075218357499750, 17.92354375535250455 ) ) ;
#1626 = DIRECTION ( 'NONE',  ( 1.000000000000000000, 0.000000000000000000, 0.000000000000000000 ) ) ;
#1627 = ORIENTED_EDGE ( 'NONE', *, *, #22674, .T. ) ;
#1628 = DIRECTION ( 'NONE',  ( 0.000000000000000000, 0.000000000000000000, 1.000000000000000000 ) ) ;
#1629 = PLANE ( 'NONE',  #29300 ) ;
#1630 = CYLINDRICAL_SURFACE ( 'NONE', #11080, 6.000000000000003553 ) ;
#1631 = EDGE_CURVE ( 'NONE', #25278, #4444, #33076, .T. ) ;
#1632 = CARTESIAN_POINT ( 'NONE',  ( 15.29022352314591870, 13.67480013622697044, -29.41691902321640129 ) ) ;
#1633 = CARTESIAN_POINT ( 'NONE',  ( 6.698736661597710196, 23.19293624795248121, -20.94025436800699680 ) ) ;
#1634 = ORIENTED_EDGE ( 'NONE', *, *, #8604, .T. ) ;
#1635 = CARTESIAN_POINT ( 'NONE',  ( -4.987329993433320396E-14, 13.65543219052647927, 9.000000000000001776 ) ) ;
#1636 = DIRECTION ( 'NONE',  ( -0.7071067811865503483, 0.000000000000000000, -0.7071067811865446862 ) ) ;
#1637 = CARTESIAN_POINT ( 'NONE',  ( 16.00895768845574096, -26.86996021029318626, -5.000000000000000888 ) ) ;
#1638 = CARTESIAN_POINT ( 'NONE',  ( 17.42101839920123041, -19.25229542401860527, 20.69868183039781329 ) ) ;
#1639 = CARTESIAN_POINT ( 'NONE',  ( -6.572794801194226544, 16.58182897866500127, 9.000000000000001776 ) ) ;
#1640 = CIRCLE ( 'NONE', #12654, 1.000000000000000000 ) ;
#1641 = ORIENTED_EDGE ( 'NONE', *, *, #34748, .T. ) ;
#1642 = CARTESIAN_POINT ( 'NONE',  ( -10.97587534684186927, 17.31416389292776614, -29.99999999999999289 ) ) ;
#1643 = CARTESIAN_POINT ( 'NONE',  ( -32.48135758214319679, -20.75321993593849257, 16.30093088680156299 ) ) ;
#1644 = CARTESIAN_POINT ( 'NONE',  ( 14.88849274807932765, -26.59100623965352739, -5.474081762690492958 ) ) ;
#1645 = DIRECTION ( 'NONE',  ( -0.000000000000000000, -0.000000000000000000, 1.000000000000000000 ) ) ;
#1646 = VERTEX_POINT ( 'NONE', #32871 ) ;
#1647 = ORIENTED_EDGE ( 'NONE', *, *, #28867, .T. ) ;
#1648 = CARTESIAN_POINT ( 'NONE',  ( -9.086544612771062290, 22.80237608603660959, -20.06330228535229310 ) ) ;
#1649 = AXIS2_PLACEMENT_3D ( 'NONE', #3131, #12277, #15528 ) ;
#1650 = CARTESIAN_POINT ( 'NONE',  ( 7.688300058587269170, 16.47782454277055564, 6.000000000000000000 ) ) ;
#1651 = PLANE ( 'NONE',  #26970 ) ;
#1652 = AXIS2_PLACEMENT_3D ( 'NONE', #24702, #28341, #15562 ) ;
#1654 = AXIS2_PLACEMENT_3D ( 'NONE', #13831, #38417, #10389 ) ;
#1653 = CARTESIAN_POINT ( 'NONE',  ( -26.18072848307312483, -5.656370036759490461, -17.86034429590615602 ) ) ;
#1655 = DIRECTION ( 'NONE',  ( 0.000000000000000000, 0.000000000000000000, 1.000000000000000000 ) ) ;
#1656 = ORIENTED_EDGE ( 'NONE', *, *, #3598, .F. ) ;
#1657 = CARTESIAN_POINT ( 'NONE',  ( 29.30560488958938237, 0.1302769183488891036, -10.65503282581417643 ) ) ;
#1658 = FACE_OUTER_BOUND ( 'NONE', #39573, .T. ) ;
#1659 = LINE ( 'NONE', #20755, #17439 ) ;
#1660 = CARTESIAN_POINT ( 'NONE',  ( -14.98890121934603314, -28.67928442654204346, 11.00000000000000000 ) ) ;
#1661 = ORIENTED_EDGE ( 'NONE', *, *, #25292, .T. ) ;
#1662 = CARTESIAN_POINT ( 'NONE',  ( -20.61119921438281821, 0.8364689388151540506, -28.07681394956128784 ) ) ;
#1663 = CARTESIAN_POINT ( 'NONE',  ( -8.118377661053486349, 10.47536095541708967, 11.00000000000000000 ) ) ;
#1665 = EDGE_CURVE ( 'NONE', #12491, #1261, #14472, .T. ) ;
#1664 = ORIENTED_EDGE ( 'NONE', *, *, #22285, .F. ) ;
#1666 = CARTESIAN_POINT ( 'NONE',  ( 33.23936858253276228, -3.197057837266320313, -6.364182858326340231 ) ) ;
#1667 = CARTESIAN_POINT ( 'NONE',  ( 36.30242391553733228, -14.63578948164456683, 14.53008259254010959 ) ) ;
#1668 = ORIENTED_EDGE ( 'NONE', *, *, #24369, .T. ) ;
#1669 = CARTESIAN_POINT ( 'NONE',  ( 11.65184672541106359, 34.81748849094131515, 15.13084544680210719 ) ) ;
#1670 = CARTESIAN_POINT ( 'NONE',  ( 4.272934335498898793E-14, -21.05812563137664739, 19.27171037444156809 ) ) ;
#1671 = DIRECTION ( 'NONE',  ( 0.5877852522924686962, -0.8090169943749506709, 0.000000000000000000 ) ) ;
#1672 = CARTESIAN_POINT ( 'NONE',  ( -6.367390439426523940, 24.26983560722021949, 20.94377226548378346 ) ) ;
#1673 = FACE_OUTER_BOUND ( 'NONE', #30728, .T. ) ;
#1674 = VERTEX_POINT ( 'NONE', #20679 ) ;
#1675 = CARTESIAN_POINT ( 'NONE',  ( 3.211395437248501850, 12.61633075744433796, 13.00000000000000178 ) ) ;
#1676 = AXIS2_PLACEMENT_3D ( 'NONE', #9385, #27868, #33971 ) ;
#1677 = EDGE_CURVE ( 'NONE', #4321, #14858, #2166, .T. ) ;
#1678 = CIRCLE ( 'NONE', #6845, 1.000000000000000000 ) ;
#1679 = CARTESIAN_POINT ( 'NONE',  ( 6.086663952044554016, 37.28955090192621213, -5.862872072945212842 ) ) ;
#1680 = VECTOR ( 'NONE', #22961, 1000.000000000000000 ) ;
#1681 = DIRECTION ( 'NONE',  ( -0.000000000000000000, -0.000000000000000000, -1.000000000000000000 ) ) ;
#1682 = EDGE_CURVE ( 'NONE', #30242, #19894, #9951, .T. ) ;
#1683 = CARTESIAN_POINT ( 'NONE',  ( 30.57450045108190650, -0.3656520783221823279, 16.87380292611441490 ) ) ;
#1684 = CARTESIAN_POINT ( 'NONE',  ( 18.27717518933982177, -25.33298382040178609, -11.36505120164252247 ) ) ;
#1685 = DIRECTION ( 'NONE',  ( 0.000000000000000000, 0.000000000000000000, 1.000000000000000000 ) ) ;
#1686 = CARTESIAN_POINT ( 'NONE',  ( -13.30786737757920335, 15.60543024394081080, 10.49999999999999822 ) ) ;
#1687 = CARTESIAN_POINT ( 'NONE',  ( 0.5000000000000001110, 37.00000000000000711, 9.500000000000000000 ) ) ;
#1688 = ORIENTED_EDGE ( 'NONE', *, *, #32117, .T. ) ;
#1689 = CARTESIAN_POINT ( 'NONE',  ( 15.37200336808687950, 26.84711675505732131, -5.945063123470434974 ) ) ;
#1690 = VERTEX_POINT ( 'NONE', #18029 ) ;
#1691 = CARTESIAN_POINT ( 'NONE',  ( -11.29390458575034373, 17.10922195600983997, -29.99999999999999645 ) ) ;
#1692 = EDGE_CURVE ( 'NONE', #37009, #39268, #29406, .T. ) ;
#1693 = CARTESIAN_POINT ( 'NONE',  ( -27.14644468510475406, -3.730463242939707769, 19.99202127657103389 ) ) ;
#1694 = DIRECTION ( 'NONE',  ( 0.000000000000000000, 0.000000000000000000, 1.000000000000000000 ) ) ;
#1695 = CARTESIAN_POINT ( 'NONE',  ( 14.06582128944119070, 23.85096756361283354, -13.51722347730761697 ) ) ;
#1696 = EDGE_LOOP ( 'NONE', ( #16701, #34705, #38462, #6147 ) ) ;
#1697 = CARTESIAN_POINT ( 'NONE',  ( 28.82830481445685677, -17.06062050408562669, -12.88833261073628478 ) ) ;
#1698 = ORIENTED_EDGE ( 'NONE', *, *, #13240, .F. ) ;
#1700 = FACE_OUTER_BOUND ( 'NONE', #6725, .T. ) ;
#1699 = CARTESIAN_POINT ( 'NONE',  ( -11.51955146840040456, 19.07033770647171877, -22.70621963616805061 ) ) ;
#1701 = CARTESIAN_POINT ( 'NONE',  ( -10.72424208444558147, -18.49280626366203961, -24.92494540156139138 ) ) ;
#1702 = CARTESIAN_POINT ( 'NONE',  ( -14.57486473880221745, 26.18419839932921533, 7.000000000000000000 ) ) ;
#1703 = EDGE_LOOP ( 'NONE', ( #29129, #16048, #24200, #27157 ) ) ;
#1704 = CARTESIAN_POINT ( 'NONE',  ( -35.38382356931356298, -13.39769055746643112, -5.000000000000005329 ) ) ;
#1705 = CARTESIAN_POINT ( 'NONE',  ( -10.14892113523442951, -19.68697069789514842, -22.78142312659023005 ) ) ;
#1706 = CARTESIAN_POINT ( 'NONE',  ( 25.22779562677032672, -30.53001673900870472, 23.00000000000093792 ) ) ;
#1707 = CARTESIAN_POINT ( 'NONE',  ( 14.83185561455345791, 18.64992817094902122, -17.71824246541178738 ) ) ;
#1708 = ORIENTED_EDGE ( 'NONE', *, *, #26546, .T. ) ;
#1709 = CARTESIAN_POINT ( 'NONE',  ( 21.00252652683522570, 3.785488330333473872, -24.15676876065577972 ) ) ;
#1710 = DIRECTION ( 'NONE',  ( 0.000000000000000000, 0.000000000000000000, 1.000000000000000000 ) ) ;
#1711 = CARTESIAN_POINT ( 'NONE',  ( -23.54493052986492430, -14.21898406159475137, 23.00000000000000000 ) ) ;
#1712 = EDGE_CURVE ( 'NONE', #27384, #5452, #20876, .T. ) ;
#1713 = CIRCLE ( 'NONE', #23097, 6.000000000000006217 ) ;
#1714 = ORIENTED_EDGE ( 'NONE', *, *, #9208, .T. ) ;
#1715 = EDGE_CURVE ( 'NONE', #40077, #18785, #11904, .T. ) ;
#1716 = CARTESIAN_POINT ( 'NONE',  ( -31.05219368549945003, -0.2312423517573455878, -5.943383185067190766 ) ) ;
#1717 = EDGE_CURVE ( 'NONE', #11442, #35565, #7437, .T. ) ;
#1718 = CARTESIAN_POINT ( 'NONE',  ( 20.99902718400924329, 0.4997691857017135253, -26.19762432007799546 ) ) ;
#1719 = VECTOR ( 'NONE', #17197, 1000.000000000000000 ) ;
#1720 = CARTESIAN_POINT ( 'NONE',  ( 30.40813597975501636, -7.345136026722032696, 19.66345542862497098 ) ) ;
#1721 = CIRCLE ( 'NONE', #21165, 15.00000000000000000 ) ;
#1722 = EDGE_LOOP ( 'NONE', ( #16171, #11373, #19448, #17460 ) ) ;
#1723 = CARTESIAN_POINT ( 'NONE',  ( -28.19395260050296770, 0.9484113493885590884, -11.62985173043690246 ) ) ;
#1724 = CARTESIAN_POINT ( 'NONE',  ( -15.29245034862078256, 32.56469986091995850, -13.99876745781543441 ) ) ;
#1725 = CARTESIAN_POINT ( 'NONE',  ( 14.75233815192021858, 19.78246761888935268, 7.202682876670055911 ) ) ;
#1726 = DIRECTION ( 'NONE',  ( 0.000000000000000000, 0.000000000000000000, -1.000000000000000000 ) ) ;
#1727 = EDGE_CURVE ( 'NONE', #14625, #5931, #1784, .T. ) ;
#1728 = CYLINDRICAL_SURFACE ( 'NONE', #5217, 0.5000000000000000000 ) ;
#1729 = DIRECTION ( 'NONE',  ( 1.000000000000000000, 0.000000000000000000, 0.000000000000000000 ) ) ;
#1730 = ADVANCED_FACE ( 'NONE', ( #29809 ), #39146, .F. ) ;
#1731 = DIRECTION ( 'NONE',  ( 0.000000000000000000, 0.000000000000000000, 1.000000000000000000 ) ) ;
#1732 = ORIENTED_EDGE ( 'NONE', *, *, #2639, .T. ) ;
#1733 = CARTESIAN_POINT ( 'NONE',  ( -21.26609381498803231, 5.820186529508268869, -21.02685273093531748 ) ) ;
#1734 = CYLINDRICAL_SURFACE ( 'NONE', #3431, 20.00000000000003908 ) ;
#1735 = DIRECTION ( 'NONE',  ( 0.000000000000000000, 0.000000000000000000, 1.000000000000000000 ) ) ;
#1736 = CARTESIAN_POINT ( 'NONE',  ( 15.94941446643157512, -13.01052313326162491, -28.46982544010355198 ) ) ;
#1737 = CARTESIAN_POINT ( 'NONE',  ( -14.36830325120615548, 20.48707633493503621, 9.000000000000001776 ) ) ;
#1738 = CARTESIAN_POINT ( 'NONE',  ( -14.85579657860262337, 20.34187940403377581, 10.49999999999999822 ) ) ;
#1739 = CARTESIAN_POINT ( 'NONE',  ( 11.83975480655455392, 20.26533495932481799, -20.48298615583043869 ) ) ;
#1740 = CARTESIAN_POINT ( 'NONE',  ( 8.559505275947156377, 25.28115294937476065, 12.00000000000000000 ) ) ;
#1741 = ORIENTED_EDGE ( 'NONE', *, *, #23042, .T. ) ;
#1743 = VECTOR ( 'NONE', #5536, 1000.000000000000000 ) ;
#1742 = CARTESIAN_POINT ( 'NONE',  ( -13.44539276212325341, 15.67996942108016967, -27.60600344130554262 ) ) ;
#1744 = CARTESIAN_POINT ( 'NONE',  ( -22.84262768307197788, -16.00844090263207065, 21.00000000000000000 ) ) ;
#1745 = CARTESIAN_POINT ( 'NONE',  ( 14.90790700096789045, -25.97435605518935731, -9.239200025327670929 ) ) ;
#1746 = LINE ( 'NONE', #11487, #24987 ) ;
#1747 = CARTESIAN_POINT ( 'NONE',  ( 14.54031622545319813, 24.94891456728954537, -11.59962563409148650 ) ) ;
#1748 = ORIENTED_EDGE ( 'NONE', *, *, #24410, .F. ) ;
#1749 = FACE_OUTER_BOUND ( 'NONE', #3413, .T. ) ;
#1750 = ORIENTED_EDGE ( 'NONE', *, *, #3369, .F. ) ;
#1752 = DIRECTION ( 'NONE',  ( 0.3090169943749457304, -0.9510565162951540863, 0.000000000000000000 ) ) ;
#1751 = CARTESIAN_POINT ( 'NONE',  ( -14.49572269434710137, 25.07545077057084981, -11.59117096907117173 ) ) ;
#1753 = CARTESIAN_POINT ( 'NONE',  ( -9.942277346636780422, -18.82355019788865746, -25.01733364873610199 ) ) ;
#1754 = CARTESIAN_POINT ( 'NONE',  ( -20.78821643698918109, -29.20280246618806430, 11.55979286843934872 ) ) ;
#1755 = CARTESIAN_POINT ( 'NONE',  ( -26.28505616161186964, -16.99079149096458607, -14.73553854996467827 ) ) ;
#1756 = CARTESIAN_POINT ( 'NONE',  ( -7.384991535497307247, -21.86536290796619397, -18.83959722162714812 ) ) ;
#1757 = CARTESIAN_POINT ( 'NONE',  ( 15.64374290521436706, 24.45313499581702743, -8.785383034557462167 ) ) ;
#1758 = ORIENTED_EDGE ( 'NONE', *, *, #12792, .T. ) ;
#1759 = CARTESIAN_POINT ( 'NONE',  ( 19.22578323039330428, 8.090122520240742077, -25.48513230106247107 ) ) ;
#1760 = CARTESIAN_POINT ( 'NONE',  ( 13.82587227205762481, 37.11292025503284009, 11.00000000000000000 ) ) ;
#1761 = CARTESIAN_POINT ( 'NONE',  ( -12.59277403104497850, 14.34973136966057616, 7.455686640544903376 ) ) ;
#1762 = DIRECTION ( 'NONE',  ( 1.000000000000000000, 0.000000000000000000, 0.000000000000000000 ) ) ;
#1763 = ORIENTED_EDGE ( 'NONE', *, *, #15705, .F. ) ;
#1764 = CARTESIAN_POINT ( 'NONE',  ( -32.47918921017399896, -2.488034356860049368, -7.737705398647766408 ) ) ;
#1765 = CARTESIAN_POINT ( 'NONE',  ( -26.56332897234805301, -4.302820985777816354, 20.25080042701566541 ) ) ;
#1766 = CARTESIAN_POINT ( 'NONE',  ( 18.64638308222462371, -17.01267446048655430, 20.99999999999995026 ) ) ;
#1767 = CARTESIAN_POINT ( 'NONE',  ( 2.525645716490518389, 8.212903943950921715, 9.000000000000001776 ) ) ;
#1768 = EDGE_CURVE ( 'NONE', #8057, #24946, #11230, .T. ) ;
#1769 = LINE ( 'NONE', #38737, #38488 ) ;
#1770 = CARTESIAN_POINT ( 'NONE',  ( 25.18859414265934049, -11.95731909848912089, -17.61046221350143526 ) ) ;
#1771 = DIRECTION ( 'NONE',  ( -0.4731467892558104960, 0.5254827454987662794, -0.7071067811865450192 ) ) ;
#1772 = CIRCLE ( 'NONE', #4980, 1.000000000000000888 ) ;
#1773 = AXIS2_PLACEMENT_3D ( 'NONE', #27581, #5638, #21092 ) ;
#1774 = ORIENTED_EDGE ( 'NONE', *, *, #27618, .T. ) ;
#1775 = DIRECTION ( 'NONE',  ( 1.000000000000000000, 0.000000000000000000, 0.000000000000000000 ) ) ;
#1776 = AXIS2_PLACEMENT_3D ( 'NONE', #39774, #14803, #20706 ) ;
#1777 = CIRCLE ( 'NONE', #28349, 1.000000000000000888 ) ;
#1778 = FACE_OUTER_BOUND ( 'NONE', #29743, .T. ) ;
#1779 = VERTEX_POINT ( 'NONE', #11329 ) ;
#1780 = CARTESIAN_POINT ( 'NONE',  ( 0.4095834978660508607, 38.24721862872263500, -6.696645721537974438 ) ) ;
#1781 = CARTESIAN_POINT ( 'NONE',  ( 6.953805871968278929, 30.22298757065274444, 13.00000000000000178 ) ) ;
#1782 = DIRECTION ( 'NONE',  ( -0.3090169943749573322, -0.9510565162951505336, 0.000000000000000000 ) ) ;
#1783 = DIRECTION ( 'NONE',  ( -0.3090169943749573878, -0.9510565162951503115, -0.000000000000000000 ) ) ;
#1784 = LINE ( 'NONE', #30215, #4083 ) ;
#1785 = CARTESIAN_POINT ( 'NONE',  ( 5.348106467989403257, 35.16482219193073178, 12.00000000000000000 ) ) ;
#1786 = CARTESIAN_POINT ( 'NONE',  ( 12.58176986377051954, 23.30251563080998878, -16.31430736139012083 ) ) ;
#1787 = DIRECTION ( 'NONE',  ( -1.000000000000000000, 0.000000000000000000, 0.000000000000000000 ) ) ;
#1788 = ORIENTED_EDGE ( 'NONE', *, *, #1813, .T. ) ;
#1790 = CARTESIAN_POINT ( 'NONE',  ( 9.831584923911648843, 26.22020669908450330, 11.00000000000000000 ) ) ;
#1789 = CARTESIAN_POINT ( 'NONE',  ( -17.05764571048761624, 11.96101966799990812, -25.49672756633158599 ) ) ;
#1791 = CARTESIAN_POINT ( 'NONE',  ( -13.67111072870484811, 27.95752071293692964, 10.49999999999999822 ) ) ;
#1792 = CARTESIAN_POINT ( 'NONE',  ( 11.92998010801955289, -21.48326688710186616, -18.44930693513468967 ) ) ;
#1793 = FACE_OUTER_BOUND ( 'NONE', #18159, .T. ) ;
#1794 = CARTESIAN_POINT ( 'NONE',  ( 12.63339664555651609, 21.08327326440629079, -18.44782762665456843 ) ) ;
#1795 = FACE_OUTER_BOUND ( 'NONE', #40017, .T. ) ;
#1796 = CARTESIAN_POINT ( 'NONE',  ( -24.22337021529747147, -9.561219044741108064, 22.99999999999999289 ) ) ;
#1797 = AXIS2_PLACEMENT_3D ( 'NONE', #34578, #6336, #21983 ) ;
#1798 = CIRCLE ( 'NONE', #30361, 1.000000000000000000 ) ;
#1799 = CARTESIAN_POINT ( 'NONE',  ( -15.54722730493476135, -13.72744853134184062, -27.75932108635244333 ) ) ;
#1800 = CARTESIAN_POINT ( 'NONE',  ( 1.815840917229304186, -24.74890125078012915, -5.967798877961429049 ) ) ;
#1801 = CARTESIAN_POINT ( 'NONE',  ( 15.30416110356804182, 25.85440126521964999, -8.300953238907675669 ) ) ;
#1802 = CARTESIAN_POINT ( 'NONE',  ( 17.40089361578718297, 12.57718761390114715, -22.22887343362824097 ) ) ;
#1803 = DIRECTION ( 'NONE',  ( -1.224646799147351235E-16, 1.000000000000000000, 0.000000000000000000 ) ) ;
#1804 = EDGE_LOOP ( 'NONE', ( #23516, #20092, #3804, #30968 ) ) ;
#1805 = B_SPLINE_CURVE_WITH_KNOTS ( 'NONE', 3,
 ( #22643, #10263, #16973, #35049 ),
 .UNSPECIFIED., .F., .F.,
 ( 4, 4 ),
 ( 0.000000000000000000, 1.000000000000000000 ),
 .UNSPECIFIED. ) ;
#1806 = CARTESIAN_POINT ( 'NONE',  ( -4.503003596829367794, 22.23197666336542255, -23.10559598243666812 ) ) ;
#1807 = AXIS2_PLACEMENT_3D ( 'NONE', #17374, #39086, #17572 ) ;
#1808 = EDGE_LOOP ( 'NONE', ( #37828, #25664 ) ) ;
#1809 = CIRCLE ( 'NONE', #6343, 15.00000000000000000 ) ;
#1810 = PLANE ( 'NONE',  #39047 ) ;
#1811 = ORIENTED_EDGE ( 'NONE', *, *, #34625, .T. ) ;
#1812 = CARTESIAN_POINT ( 'NONE',  ( 22.37674264578617667, 24.85189042352198641, 7.000000000000000000 ) ) ;
#1813 = EDGE_CURVE ( 'NONE', #35819, #22041, #23556, .T. ) ;
#1814 = DIRECTION ( 'NONE',  ( 0.3090169943749450643, -0.9510565162951544194, 0.000000000000000000 ) ) ;
#1815 = EDGE_LOOP ( 'NONE', ( #20216, #34 ) ) ;
#1816 = CARTESIAN_POINT ( 'NONE',  ( -30.29861199217504009, 0.4131864886508529455, -6.889171040952208891 ) ) ;
#1817 = ORIENTED_EDGE ( 'NONE', *, *, #21931, .T. ) ;
#1818 = CARTESIAN_POINT ( 'NONE',  ( 34.32017124965129540, -10.33516403750143198, -8.900617703435305117 ) ) ;
#1819 = ADVANCED_FACE ( 'NONE', ( #2186 ), #8875, .T. ) ;
#1820 = ADVANCED_FACE ( 'NONE', ( #21265 ), #15965, .F. ) ;
#1821 = ORIENTED_EDGE ( 'NONE', *, *, #14362, .F. ) ;
#1822 = CONTEXT_DEPENDENT_SHAPE_REPRESENTATION ( #17150, #16514 ) ;
#1823 = CARTESIAN_POINT ( 'NONE',  ( 10.72918489117958174, 32.98258515686296732, 7.499999999999997335 ) ) ;
#1824 = VERTEX_POINT ( 'NONE', #37503 ) ;
#1825 = EDGE_CURVE ( 'NONE', #3811, #17784, #36546, .T. ) ;
#1826 = CIRCLE ( 'NONE', #36844, 1.000000000000000000 ) ;
#1827 = CARTESIAN_POINT ( 'NONE',  ( 0.7344908159097338629, 8.754836972118123839, 13.00000000000000178 ) ) ;
#1828 = CARTESIAN_POINT ( 'NONE',  ( 1.853166178176219203, 23.42705098312512746, 13.00000000000000178 ) ) ;
#1829 = CARTESIAN_POINT ( 'NONE',  ( 8.307596863005482390, 33.43166269068607477, 18.42518152272108978 ) ) ;
#1830 = CIRCLE ( 'NONE', #39428, 18.00000000000003553 ) ;
#1831 = CIRCLE ( 'NONE', #28436, 6.000000000000003553 ) ;
#1832 = DIRECTION ( 'NONE',  ( -0.5720614028176804755, -0.4156269377774462481, 0.7071067811865549002 ) ) ;
#1833 = ORIENTED_EDGE ( 'NONE', *, *, #7795, .F. ) ;
#1834 = CYLINDRICAL_SURFACE ( 'NONE', #29490, 0.5000000000000004441 ) ;
#1835 = DIRECTION ( 'NONE',  ( 0.000000000000000000, 0.000000000000000000, 1.000000000000000000 ) ) ;
#1836 = AXIS2_PLACEMENT_3D ( 'NONE', #37041, #11861, #2523 ) ;
#1837 = CARTESIAN_POINT ( 'NONE',  ( 10.10646936306337729, 32.94553861768082470, 11.00000000000000000 ) ) ;
#1838 = CARTESIAN_POINT ( 'NONE',  ( 15.49054523282929807, 15.24218747636109050, -22.10330208559187426 ) ) ;
#1839 = AXIS2_PLACEMENT_3D ( 'NONE', #33935, #205, #34531 ) ;
#1840 = CARTESIAN_POINT ( 'NONE',  ( 6.309536247299392109, 19.51471286317475773, -29.99999999999999645 ) ) ;
#1841 = VERTEX_POINT ( 'NONE', #18819 ) ;
#1842 = CARTESIAN_POINT ( 'NONE',  ( 12.80736835487432934, 15.68301270189215835, 11.00000000000000000 ) ) ;
#1843 = FACE_OUTER_BOUND ( 'NONE', #7888, .T. ) ;
#1844 = EDGE_CURVE ( 'NONE', #22956, #31091, #3177, .T. ) ;
#1845 = ADVANCED_FACE ( 'NONE', ( #2978 ), #19027, .T. ) ;
#1846 = CARTESIAN_POINT ( 'NONE',  ( 15.43059434986342104, -26.34277824748516039, -8.288079929563053838 ) ) ;
#1847 = CARTESIAN_POINT ( 'NONE',  ( 37.48557158514985588, -11.25000000000009415, 0.000000000000000000 ) ) ;
#1848 = DIRECTION ( 'NONE',  ( 0.7431448254773862505, -0.6691306063588670083, 0.000000000000000000 ) ) ;
#1849 = CARTESIAN_POINT ( 'NONE',  ( -14.73215445377065258, 25.41255716721991220, -10.65209943420422434 ) ) ;
#1850 = CARTESIAN_POINT ( 'NONE',  ( -29.60586052328872597, -25.59238499872923711, 13.92931973827819725 ) ) ;
#1851 = CARTESIAN_POINT ( 'NONE',  ( 14.23504194582299753, -26.35893216010225615, -6.418547458806204808 ) ) ;
#1852 = LINE ( 'NONE', #11188, #36742 ) ;
#1853 = EDGE_LOOP ( 'NONE', ( #36304, #15483, #37549, #20225, #29233, #37704, #6383 ) ) ;
#1854 = ORIENTED_EDGE ( 'NONE', *, *, #31044, .T. ) ;
#1855 = CARTESIAN_POINT ( 'NONE',  ( -8.078176917764361420, 20.10266963944688356, -24.61727802958278133 ) ) ;
#1856 = CARTESIAN_POINT ( 'NONE',  ( 10.44103466624280685, 32.57396620494213124, 7.000000000000000000 ) ) ;
#1857 = FACE_BOUND ( 'NONE', #16912, .T. ) ;
#1858 = AXIS2_PLACEMENT_3D ( 'NONE', #18848, #21298, #157 ) ;
#1859 = VECTOR ( 'NONE', #13838, 999.9999999999998863 ) ;
#1860 = CARTESIAN_POINT ( 'NONE',  ( -26.92548543374830672, -4.182384202632584369, -16.97462146561391805 ) ) ;
#1861 = DIRECTION ( 'NONE',  ( 0.000000000000000000, -1.000000000000000000, -0.000000000000000000 ) ) ;
#1862 = ORIENTED_EDGE ( 'NONE', *, *, #14052, .F. ) ;
#1863 = CARTESIAN_POINT ( 'NONE',  ( 26.45401934139566791, 0.3544644617807020670, -15.45655976044637825 ) ) ;
#1864 = DIRECTION ( 'NONE',  ( 1.000000000000000000, 0.000000000000000000, 0.000000000000000000 ) ) ;
#1865 = FACE_OUTER_BOUND ( 'NONE', #11055, .T. ) ;
#1866 = CARTESIAN_POINT ( 'NONE',  ( -2.109203785269543996, 7.931710454523169140, 10.49999999999999822 ) ) ;
#1867 = CIRCLE ( 'NONE', #33659, 1.000000000000000444 ) ;
#1868 = ORIENTED_EDGE ( 'NONE', *, *, #12854, .F. ) ;
#1869 = CARTESIAN_POINT ( 'NONE',  ( -21.70835098058958934, 0.7322611594438664939, -23.85456472341968492 ) ) ;
#1870 = EDGE_CURVE ( 'NONE', #15928, #13281, #21656, .T. ) ;
#1871 = DIRECTION ( 'NONE',  ( 0.000000000000000000, 0.000000000000000000, 1.000000000000000000 ) ) ;
#1872 = VERTEX_POINT ( 'NONE', #24907 ) ;
#1873 = CARTESIAN_POINT ( 'NONE',  ( 22.74168006064742187, -2.578368022317651054, -22.34712926292036883 ) ) ;
#1874 = AXIS2_PLACEMENT_3D ( 'NONE', #15398, #5853, #11953 ) ;
#1875 = CARTESIAN_POINT ( 'NONE',  ( 34.08416769313340211, -19.67850339273466176, 15.13084544680213739 ) ) ;
#1876 = ORIENTED_EDGE ( 'NONE', *, *, #24459, .F. ) ;
#1877 = CARTESIAN_POINT ( 'NONE',  ( -5.476246462222815303, 38.75671607062959367, 14.53008259254010959 ) ) ;
#1878 = CARTESIAN_POINT ( 'NONE',  ( -10.51283450064414637, -24.98199432659117747, 16.87380292611976884 ) ) ;
#1879 = CARTESIAN_POINT ( 'NONE',  ( 4.984135866956514782, 36.15314577889351000, 9.500000000000000000 ) ) ;
#1880 = CARTESIAN_POINT ( 'NONE',  ( 3.486159013132950513, 30.04627872069376338, 20.69868183039781684 ) ) ;
#1881 = DIRECTION ( 'NONE',  ( 1.000000000000000000, 0.000000000000000000, 0.000000000000000000 ) ) ;
#1882 = ORIENTED_EDGE ( 'NONE', *, *, #24342, .T. ) ;
#1883 = CARTESIAN_POINT ( 'NONE',  ( -8.744117900323422177, 12.16605582823074982, 10.50000000000000000 ) ) ;
#1884 = TOROIDAL_SURFACE ( 'NONE', #18100, 1.000000000000000000, 0.5000000000000000000 ) ;
#1886 = AXIS2_PLACEMENT_3D ( 'NONE', #1185, #28606, #29412 ) ;
#1885 = CARTESIAN_POINT ( 'NONE',  ( 5.995512085838934802, 36.57033614599139781, -7.995356539080317404 ) ) ;
#1887 = CARTESIAN_POINT ( 'NONE',  ( -4.577399223880544099, 35.23960032125097541, 9.500000000000000000 ) ) ;
#1888 = CARTESIAN_POINT ( 'NONE',  ( 15.48226359616410086, 8.938689054910316401, 20.50957957746029336 ) ) ;
#1889 = EDGE_CURVE ( 'NONE', #33038, #25337, #3370, .T. ) ;
#1890 = CARTESIAN_POINT ( 'NONE',  ( 11.74422086145278499, -16.80344316252863734, -29.99999999999999289 ) ) ;
#1891 = CARTESIAN_POINT ( 'NONE',  ( -3.900486991066764553, 40.17991855517990274, 11.00000000000018474 ) ) ;
#1892 = AXIS2_PLACEMENT_3D ( 'NONE', #20958, #2671, #33765 ) ;
#1893 = CARTESIAN_POINT ( 'NONE',  ( -35.48557158811166090, -13.25318502726451442, -4.999999999999997335 ) ) ;
#1894 = CARTESIAN_POINT ( 'NONE',  ( -9.183247089818959097, 16.78440424842446532, 6.000000000000000000 ) ) ;
#1895 = ORIENTED_EDGE ( 'NONE', *, *, #32466, .F. ) ;
#1896 = CARTESIAN_POINT ( 'NONE',  ( 12.06198199496667023, 20.00631599209042832, -20.52696379477532673 ) ) ;
#1897 = VERTEX_POINT ( 'NONE', #9678 ) ;
#1898 = CARTESIAN_POINT ( 'NONE',  ( -14.84652007656822015, 25.07892745533905554, -10.66023937599700844 ) ) ;
#1899 = CARTESIAN_POINT ( 'NONE',  ( -29.95834561893252612, -4.698932123269424999, 19.27171037444122703 ) ) ;
#1900 = DIRECTION ( 'NONE',  ( 0.000000000000000000, 0.000000000000000000, 1.000000000000000000 ) ) ;
#1901 = CARTESIAN_POINT ( 'NONE',  ( 12.97456259195843131, 21.57840362866582140, -17.44539012491156171 ) ) ;
#1902 = EDGE_LOOP ( 'NONE', ( #18747, #37802, #33933, #21876 ) ) ;
#1903 = CARTESIAN_POINT ( 'NONE',  ( 31.48159048268411908, -18.63039699574827779, -9.724746473303273575 ) ) ;
#1904 = EDGE_LOOP ( 'NONE', ( #9050, #2463, #21703, #1664 ) ) ;
#1906 = CARTESIAN_POINT ( 'NONE',  ( 13.49038105676655164, 15.86602540378438064, 7.000000000000000000 ) ) ;
#1905 = CARTESIAN_POINT ( 'NONE',  ( -12.34485101014255015, 21.50093162914449962, -18.38636203722984774 ) ) ;
#1907 = CARTESIAN_POINT ( 'NONE',  ( -15.27090603634302468, -24.25807912277981160, -13.38554782441437574 ) ) ;
#1908 = CARTESIAN_POINT ( 'NONE',  ( -13.63581098909220479, 27.45627467658446008, 7.000000000000000000 ) ) ;
#1909 = ORIENTED_EDGE ( 'NONE', *, *, #18794, .F. ) ;
#1910 = CARTESIAN_POINT ( 'NONE',  ( -23.87677460445570432, -9.044431454778111501, -19.70507607847654441 ) ) ;
#1911 = CARTESIAN_POINT ( 'NONE',  ( -10.43523929675511752, -20.08486062915910964, -21.66559121846610481 ) ) ;
#1912 = DIRECTION ( 'NONE',  ( -0.000000000000000000, -0.000000000000000000, -1.000000000000000000 ) ) ;
#1913 = CARTESIAN_POINT ( 'NONE',  ( 16.74741356090710909, 20.23878986518512590, -10.77388661789859547 ) ) ;
#1914 = VERTEX_POINT ( 'NONE', #5826 ) ;
#1915 = CARTESIAN_POINT ( 'NONE',  ( 29.41166959288484151, 1.126308269877565937, -7.836244769277370459 ) ) ;
#1916 = DIRECTION ( 'NONE',  ( 0.000000000000000000, 0.000000000000000000, 1.000000000000000000 ) ) ;
#1917 = CARTESIAN_POINT ( 'NONE',  ( -25.22779562677360232, -30.53001673900768864, 11.00000000000000000 ) ) ;
#1918 = ORIENTED_EDGE ( 'NONE', *, *, #2599, .F. ) ;
#1919 = CARTESIAN_POINT ( 'NONE',  ( -27.34250074455049884, -0.04617288401425825167, -14.44431459720212452 ) ) ;
#1920 = EDGE_CURVE ( 'NONE', #4426, #6906, #26801, .T. ) ;
#1921 = CARTESIAN_POINT ( 'NONE',  ( 27.75004729309793561, -0.6577060458606293070, -14.37818117014819919 ) ) ;
#1922 = CIRCLE ( 'NONE', #6417, 0.5000000000000004441 ) ;
#1923 = ADVANCED_FACE ( 'NONE', ( #2776 ), #6602, .T. ) ;
#1924 = CARTESIAN_POINT ( 'NONE',  ( 29.45678984391886246, -18.54179626184217611, 19.27171037444156454 ) ) ;
#1925 = ORIENTED_EDGE ( 'NONE', *, *, #35246, .F. ) ;
#1926 = CARTESIAN_POINT ( 'NONE',  ( -23.83078355888692812, 1.968671533367746695, -18.61202462238880528 ) ) ;
#1927 = AXIS2_PLACEMENT_3D ( 'NONE', #24798, #2870, #6697 ) ;
#1928 = CARTESIAN_POINT ( 'NONE',  ( 9.163310636333564574, 20.63632441393291117, -20.55760979252978871 ) ) ;
#1929 = DIRECTION ( 'NONE',  ( 0.5877852522924689183, -0.8090169943749506709, 0.000000000000000000 ) ) ;
#1930 = EDGE_CURVE ( 'NONE', #36749, #29091, #33866, .T. ) ;
#1931 = CARTESIAN_POINT ( 'NONE',  ( 0.2655024426717602637, 36.24516302788250499, 13.00000000000000178 ) ) ;
#1932 = CARTESIAN_POINT ( 'NONE',  ( -8.137585970691990411, 29.15429895402940730, 10.00000000000000000 ) ) ;
#1933 = DIRECTION ( 'NONE',  ( 0.000000000000000000, 0.000000000000000000, 1.000000000000000000 ) ) ;
#1934 = CARTESIAN_POINT ( 'NONE',  ( -5.022716998311358871, 36.63466579533663747, 7.202682876670054135 ) ) ;
#1935 = VERTEX_POINT ( 'NONE', #15567 ) ;
#1936 = CARTESIAN_POINT ( 'NONE',  ( -19.89457789833269885, 5.001894110080484346, -30.00000000000000355 ) ) ;
#1937 = LINE ( 'NONE', #39095, #9264 ) ;
#1938 = CARTESIAN_POINT ( 'NONE',  ( 9.293999462566146619, 11.53598992149257008, 6.000000000000000000 ) ) ;
#1939 = CARTESIAN_POINT ( 'NONE',  ( 15.08063968188699633, -13.89948965651085544, -29.23638960183474467 ) ) ;
#1940 = ADVANCED_FACE ( 'NONE', ( #3569 ), #9076, .F. ) ;
#1941 = EDGE_CURVE ( 'NONE', #6642, #7803, #7968, .T. ) ;
#1942 = DIRECTION ( 'NONE',  ( 0.2079116908177522649, -0.9781476007338071321, 0.000000000000000000 ) ) ;
#1943 = DIRECTION ( 'NONE',  ( 0.000000000000000000, 0.000000000000000000, 1.000000000000000000 ) ) ;
#1944 = EDGE_CURVE ( 'NONE', #30326, #6441, #36712, .T. ) ;
#1945 = CARTESIAN_POINT ( 'NONE',  ( 12.38141567392068687, 21.44998459107262079, -18.39378981892021514 ) ) ;
#1946 = FACE_OUTER_BOUND ( 'NONE', #40149, .T. ) ;
#1947 = VECTOR ( 'NONE', #31201, 1000.000000000000000 ) ;
#1948 = ORIENTED_EDGE ( 'NONE', *, *, #13340, .F. ) ;
#1949 = CARTESIAN_POINT ( 'NONE',  ( -16.39082840404886454, 22.60326311949512856, -8.330118112291499344 ) ) ;
#1950 = CARTESIAN_POINT ( 'NONE',  ( -24.49409870380020848, -11.70597971641812407, 20.99999999999999645 ) ) ;
#1951 = CARTESIAN_POINT ( 'NONE',  ( 9.747420686303255977, -18.58103426662601976, -26.22846927056824029 ) ) ;
#1952 = CARTESIAN_POINT ( 'NONE',  ( 0.000000000000000000, 22.50000000000000355, 7.000000000000000000 ) ) ;
#1953 = CARTESIAN_POINT ( 'NONE',  ( 12.14677104559135223, 19.90516762884751145, -20.54385670340190728 ) ) ;
#1954 = EDGE_LOOP ( 'NONE', ( #13424, #12399, #14022, #25865 ) ) ;
#1955 = DIRECTION ( 'NONE',  ( 0.3090169943749573878, 0.9510565162951503115, 0.000000000000000000 ) ) ;
#1956 = VECTOR ( 'NONE', #12953, 999.9999999999998863 ) ;
#1957 = ORIENTED_EDGE ( 'NONE', *, *, #21762, .T. ) ;
#1959 = CYLINDRICAL_SURFACE ( 'NONE', #39979, 1.000000000000000000 ) ;
#1958 = CARTESIAN_POINT ( 'NONE',  ( -10.92371859659766997, 17.40081432387707139, -28.70352546633995061 ) ) ;
#1960 = CARTESIAN_POINT ( 'NONE',  ( -14.37944461722531209, -25.07460220977852572, -11.59761445704505434 ) ) ;
#1961 = CARTESIAN_POINT ( 'NONE',  ( -35.07402885326980879, -20.24999999999981881, 11.00000000000000000 ) ) ;
#1962 = CARTESIAN_POINT ( 'NONE',  ( -17.56844388188584105, -11.33456651210386212, -26.97071349576603794 ) ) ;
#1963 = CARTESIAN_POINT ( 'NONE',  ( -6.162728302860261742, -19.68972925932091655, -28.22432696427634724 ) ) ;
#1964 = CARTESIAN_POINT ( 'NONE',  ( 13.25686098472626284, 20.17904452966509865, -18.55287099426779562 ) ) ;
#1965 = ORIENTED_EDGE ( 'NONE', *, *, #20027, .T. ) ;
#1966 = CARTESIAN_POINT ( 'NONE',  ( 24.60674742379866942, 6.403599265695853582, -10.32857759193655767 ) ) ;
#1967 = CARTESIAN_POINT ( 'NONE',  ( 12.80736835487433289, 15.68301270189216545, 11.00000000000000000 ) ) ;
#1968 = CYLINDRICAL_SURFACE ( 'NONE', #10172, 17.00000000000000000 ) ;
#1969 = CARTESIAN_POINT ( 'NONE',  ( 2.199596516245916789, 8.143600047011672061, 10.66666666666666075 ) ) ;
#1970 = VERTEX_POINT ( 'NONE', #6017 ) ;
#1971 = CARTESIAN_POINT ( 'NONE',  ( -28.56073700750507172, -2.042319486728655598, -14.24662277060652649 ) ) ;
#1972 = EDGE_CURVE ( 'NONE', #17859, #7248, #12445, .T. ) ;
#1973 = CARTESIAN_POINT ( 'NONE',  ( 29.61024540805226479, 0.03371321916767414106, -10.18003961060840723 ) ) ;
#1974 = ADVANCED_FACE ( 'NONE', ( #6218 ), #9290, .T. ) ;
#1975 = CARTESIAN_POINT ( 'NONE',  ( -25.38348611796302734, -5.460896781494596119, 20.69868183039781329 ) ) ;
#1976 = ADVANCED_FACE ( 'NONE', ( #22850 ), #10674, .F. ) ;
#1977 = CARTESIAN_POINT ( 'NONE',  ( 25.96434769773125240, -12.55439225991619701, 20.94377226548379411 ) ) ;
#1978 = CARTESIAN_POINT ( 'NONE',  ( -6.282361020112263716, 14.70372268239681190, 10.50000000000000533 ) ) ;
#1979 = B_SPLINE_CURVE_WITH_KNOTS ( 'NONE', 3,
 ( #15645, #28031, #34336, #6487, #9751, #3449, #4247, #37974 ),
 .UNSPECIFIED., .F., .F.,
 ( 4, 2, 2, 4 ),
 ( 0.000000000000000000, 0.0002364868538934304361, 0.0004729737077868608722, 0.0009459474155737221781 ),
 .UNSPECIFIED. ) ;
#1980 = SURFACE_SIDE_STYLE ('',( #1566 ) ) ;
#1981 = CARTESIAN_POINT ( 'NONE',  ( 4.724371395536106633, 32.23037938972932892, 6.000000000000000000 ) ) ;
#1982 = ORIENTED_EDGE ( 'NONE', *, *, #11505, .F. ) ;
#1983 = AXIS2_PLACEMENT_3D ( 'NONE', #5219, #17631, #8670 ) ;
#1984 = DIRECTION ( 'NONE',  ( -0.6123724356957936932, -0.3535533905932657373, -0.7071067811865523467 ) ) ;
#1985 = CARTESIAN_POINT ( 'NONE',  ( -2.525645716490711568, 8.212903943950959018, 9.500000000000000000 ) ) ;
#1986 = EDGE_LOOP ( 'NONE', ( #20235, #23112, #9530, #9981 ) ) ;
#1987 = CARTESIAN_POINT ( 'NONE',  ( 0.2523995269484193282, 23.75652376906266738, -21.83831241996571748 ) ) ;
#1988 = CARTESIAN_POINT ( 'NONE',  ( 3.211395437248501850, 12.61633075744433796, 6.000000000000000000 ) ) ;
#1989 = CARTESIAN_POINT ( 'NONE',  ( 14.81881748179396219, 20.25565617689056452, 10.49999999999999822 ) ) ;
#1990 = DIRECTION ( 'NONE',  ( -0.3090169943749448977, 0.9510565162951543083, 0.000000000000000000 ) ) ;
#1991 = DIRECTION ( 'NONE',  ( 0.000000000000000000, 0.000000000000000000, 1.000000000000000000 ) ) ;
#1992 = DIRECTION ( 'NONE',  ( -0.9781476007338069101, -0.2079116908177535972, 0.000000000000000000 ) ) ;
#1993 = ADVANCED_FACE ( 'NONE', ( #9866 ), #37892, .T. ) ;
#1994 = CARTESIAN_POINT ( 'NONE',  ( 10.68390316795789907, 19.09395626910841059, -23.73008332297526835 ) ) ;
#1995 = CARTESIAN_POINT ( 'NONE',  ( 14.36830325120613594, 20.48707633493483371, 9.000000000000001776 ) ) ;
#1996 = ORIENTED_EDGE ( 'NONE', *, *, #24508, .T. ) ;
#1997 = AXIS2_PLACEMENT_3D ( 'NONE', #31151, #25638, #37442 ) ;
#1999 = CARTESIAN_POINT ( 'NONE',  ( -21.55328011382844977, 16.02264588471131646, 11.00000000000000000 ) ) ;
#1998 = CARTESIAN_POINT ( 'NONE',  ( -17.59558984373777335, 14.85646055678510180, -16.92593635294098675 ) ) ;
#2000 = CARTESIAN_POINT ( 'NONE',  ( -14.48927117870118408, -30.61587158504671535, 23.00000000000000355 ) ) ;
#2001 = AXIS2_PLACEMENT_3D ( 'NONE', #13298, #25694, #10874 ) ;
#2002 = CARTESIAN_POINT ( 'NONE',  ( 9.540684313847151543, -18.19539630009126796, -28.70617519958423358 ) ) ;
#2003 = DIRECTION ( 'NONE',  ( -0.9135454576426006446, 0.4067366430758008744, 0.000000000000000000 ) ) ;
#2004 = CARTESIAN_POINT ( 'NONE',  ( 11.01682622236871190, 17.44023727289612680, -28.07602756421292511 ) ) ;
#2005 = CARTESIAN_POINT ( 'NONE',  ( -14.97009266215794021, 21.42933399866948463, 10.49999999999999822 ) ) ;
#2006 = DIRECTION ( 'NONE',  ( 1.000000000000000000, 0.000000000000000000, 0.000000000000000000 ) ) ;
#2007 = CARTESIAN_POINT ( 'NONE',  ( -16.02710008567369471, -14.15296568158351675, -25.66971380233889377 ) ) ;
#2008 = CARTESIAN_POINT ( 'NONE',  ( 1.777943910967427765, -24.47318281018553776, -8.902071781458595012 ) ) ;
#2009 = CARTESIAN_POINT ( 'NONE',  ( 15.15225747352173080, 25.54735692720815621, -9.243652212863397111 ) ) ;
#2010 = CARTESIAN_POINT ( 'NONE',  ( 16.79293355945483768, 12.02408141436283096, -27.16697041235419263 ) ) ;
#2011 = CARTESIAN_POINT ( 'NONE',  ( 3.853166178176219425, 23.42705098312512746, 6.000000000000000000 ) ) ;
#2012 = ORIENTED_EDGE ( 'NONE', *, *, #1026, .T. ) ;
#2013 = AXIS2_PLACEMENT_3D ( 'NONE', #25802, #19709, #38198 ) ;
#2014 = CARTESIAN_POINT ( 'NONE',  ( -5.483409067041409735, 26.92266725723538912, -17.70185542587633520 ) ) ;
#2015 = VERTEX_POINT ( 'NONE', #16569 ) ;
#2016 = DIRECTION ( 'NONE',  ( 1.000000000000000000, 0.000000000000000000, 0.000000000000000000 ) ) ;
#2017 = ORIENTED_EDGE ( 'NONE', *, *, #19039, .T. ) ;
#2018 = EDGE_CURVE ( 'NONE', #19442, #30652, #35888, .T. ) ;
#2019 = DIRECTION ( 'NONE',  ( -1.000000000000000000, 0.000000000000000000, 0.000000000000000000 ) ) ;
#2020 = DIRECTION ( 'NONE',  ( 0.1045284632676566766, 0.9945218953682730678, 0.000000000000000000 ) ) ;
#2021 = VERTEX_POINT ( 'NONE', #10467 ) ;
#2022 = CARTESIAN_POINT ( 'NONE',  ( -28.99011627634691379, 0.4950866871714426076, -10.66519856541149203 ) ) ;
#2023 = ORIENTED_EDGE ( 'NONE', *, *, #236, .T. ) ;
#2024 = CARTESIAN_POINT ( 'NONE',  ( 21.66385282246533706, -6.550364480499578868, -23.14497041608409944 ) ) ;
#2025 = VECTOR ( 'NONE', #33954, 1000.000000000000000 ) ;
#2026 = ORIENTED_EDGE ( 'NONE', *, *, #23863, .F. ) ;
#2027 = ITEM_DEFINED_TRANSFORMATION ( 'NONE', 'NONE', #20362,  #24238 ) ;
#2028 = CARTESIAN_POINT ( 'NONE',  ( 1.590043107810628964, 12.61456814725305442, 10.49999999999999467 ) ) ;
#2029 = ORIENTED_EDGE ( 'NONE', *, *, #28253, .F. ) ;
#2030 = CARTESIAN_POINT ( 'NONE',  ( 4.458865582155095986, 18.48521636184714012, 12.00000000000000000 ) ) ;
#2031 = DIRECTION ( 'NONE',  ( -0.6916548014802247346, -0.1470157664651938756, 0.7071067811865492381 ) ) ;
#2032 = CARTESIAN_POINT ( 'NONE',  ( 8.007761790012084546, 9.776959832083274904, 10.49999999999999822 ) ) ;
#2033 = VERTEX_POINT ( 'NONE', #13103 ) ;
#2034 = LINE ( 'NONE', #14414, #10664 ) ;
#2035 = CARTESIAN_POINT ( 'NONE',  ( 1.358225888363031819, 11.68927977431952137, 12.00000000000000000 ) ) ;
#2036 = VECTOR ( 'NONE', #34902, 1000.000000000000000 ) ;
#2037 = CARTESIAN_POINT ( 'NONE',  ( -2.476907992048017260, 18.63850621467409496, 12.00000000000000000 ) ) ;
#2038 = CARTESIAN_POINT ( 'NONE',  ( 17.38826120058489977, 16.41976207655657305, -14.83715943985794006 ) ) ;
#2039 = CARTESIAN_POINT ( 'NONE',  ( 7.074295817134445663, 19.80110017896302921, -26.49286407288892420 ) ) ;
#2040 = ORIENTED_EDGE ( 'NONE', *, *, #10805, .F. ) ;
#2041 = LINE ( 'NONE', #32316, #7339 ) ;
#2042 = LINE ( 'NONE', #2241, #12971 ) ;
#2043 = EDGE_CURVE ( 'NONE', #15223, #19849, #19655, .T. ) ;
#2044 = CARTESIAN_POINT ( 'NONE',  ( 15.12144832649043913, -25.88752217724391969, -9.695795975739306627 ) ) ;
#2045 = FACE_OUTER_BOUND ( 'NONE', #24586, .T. ) ;
#2046 = CARTESIAN_POINT ( 'NONE',  ( 12.05832241004688399, 18.99596958976722760, -21.04195414767209726 ) ) ;
#2047 = CARTESIAN_POINT ( 'NONE',  ( -11.89245061573173956, 19.38187911134576069, -21.61709387797126425 ) ) ;
#2048 = AXIS2_PLACEMENT_3D ( 'NONE', #20521, #26604, #7914 ) ;
#2049 = CARTESIAN_POINT ( 'NONE',  ( -36.43809855126085750, -10.93713533239294300, 15.13084544680293497 ) ) ;
#2050 = CARTESIAN_POINT ( 'NONE',  ( 11.73272494866245097, -22.55029353769394618, -16.51294986919664254 ) ) ;
#2051 = AXIS2_PLACEMENT_3D ( 'NONE', #11019, #19958, #38239 ) ;
#2052 = LINE ( 'NONE', #29469, #23768 ) ;
#2053 = EDGE_CURVE ( 'NONE', #21971, #38824, #31800, .T. ) ;
#2054 = VERTEX_POINT ( 'NONE', #926 ) ;
#2055 = ORIENTED_EDGE ( 'NONE', *, *, #14868, .F. ) ;
#2056 = CARTESIAN_POINT ( 'NONE',  ( -9.368025324006740817, 25.77638131019460843, -16.93723336282096881 ) ) ;
#2057 = CARTESIAN_POINT ( 'NONE',  ( -5.440908595777636414, 35.94977745735568675, 7.000000000000000000 ) ) ;
#2058 = DIRECTION ( 'NONE',  ( 0.9510565162951548634, 0.3090169943749434545, 0.000000000000000000 ) ) ;
#2059 = CARTESIAN_POINT ( 'NONE',  ( -12.19134295108997890, 16.61602540378455117, 9.500000000000000000 ) ) ;
#2060 = ORIENTED_EDGE ( 'NONE', *, *, #13963, .T. ) ;
#2061 = CARTESIAN_POINT ( 'NONE',  ( 21.26977380105256898, 0.8230692367304124346, -25.01963132466870121 ) ) ;
#2062 = CARTESIAN_POINT ( 'NONE',  ( 11.11016527260166953, 31.83082137946472656, 11.00000000000000000 ) ) ;
#2063 = LINE ( 'NONE', #39421, #12227 ) ;
#2064 = AXIS2_PLACEMENT_3D ( 'NONE', #10796, #29875, #26226 ) ;
#2065 = CARTESIAN_POINT ( 'NONE',  ( -2.544902299099670362, 8.122308845603198435, 10.99387789255783332 ) ) ;
#2066 = ORIENTED_EDGE ( 'NONE', *, *, #19550, .F. ) ;
#2067 = CARTESIAN_POINT ( 'NONE',  ( -22.21787668464120813, 0.6769409624482073395, -22.73667545006919255 ) ) ;
#2068 = CARTESIAN_POINT ( 'NONE',  ( -13.74617375768319327, 27.96120515612786761, 10.49999999999999467 ) ) ;
#2069 = EDGE_LOOP ( 'NONE', ( #28914, #13912, #28736, #3484, #2314 ) ) ;
#2070 = CARTESIAN_POINT ( 'NONE',  ( 24.27315791929659028, -3.535071426570953523, -20.06604538996125697 ) ) ;
#2071 = CARTESIAN_POINT ( 'NONE',  ( 36.37100582830206719, -12.78888441968064349, 15.13084544680218002 ) ) ;
#2072 = VERTEX_POINT ( 'NONE', #25493 ) ;
#2073 = CARTESIAN_POINT ( 'NONE',  ( -10.37941170769518529, 36.15788802554169479, 14.53008259254010959 ) ) ;
#2074 = ADVANCED_FACE ( 'NONE', ( #16165 ), #28949, .F. ) ;
#2075 = CARTESIAN_POINT ( 'NONE',  ( -10.35515495760927784, -25.90830221534925926, 15.72805884749706529 ) ) ;
#2076 = CARTESIAN_POINT ( 'NONE',  ( 5.953805871968278929, 30.22298757065274444, 13.00000000000000178 ) ) ;
#2077 = CARTESIAN_POINT ( 'NONE',  ( -2.638259136957760820, 30.33190274691516208, 20.69868183039781329 ) ) ;
#2078 = CIRCLE ( 'NONE', #29962, 1.000000000000000888 ) ;
#2079 = CARTESIAN_POINT ( 'NONE',  ( -3.607749162633401507, 7.931741834401821123, 10.49999999999999822 ) ) ;
#2080 = ORIENTED_EDGE ( 'NONE', *, *, #19695, .T. ) ;
#2081 = LINE ( 'NONE', #5120, #32752 ) ;
#2082 = CARTESIAN_POINT ( 'NONE',  ( 8.806975420853749625, 31.15003855377755571, 12.00000000000000000 ) ) ;
#2083 = CARTESIAN_POINT ( 'NONE',  ( 3.791040245356329663, 23.32460076806784599, -21.91667373837261223 ) ) ;
#2084 = DIRECTION ( 'NONE',  ( 1.000000000000000000, 0.000000000000000000, 0.000000000000000000 ) ) ;
#2085 = CARTESIAN_POINT ( 'NONE',  ( 12.58275666885947075, 13.96078236990229016, 20.50957957746036442 ) ) ;
#2086 = AXIS2_PLACEMENT_3D ( 'NONE', #33850, #5409, #36298 ) ;
#2087 = CARTESIAN_POINT ( 'NONE',  ( 12.56835645552544811, -16.80047637095704971, -26.57836621293479951 ) ) ;
#2088 = CARTESIAN_POINT ( 'NONE',  ( 5.440908595777814050, 35.94977745735560859, 7.000000000000000000 ) ) ;
#2089 = CARTESIAN_POINT ( 'NONE',  ( -13.28710325169430106, 15.51393791734817640, 10.49999999999999822 ) ) ;
#2090 = CARTESIAN_POINT ( 'NONE',  ( -1.000000000000000000, 37.00000000000000711, 11.00000000000000000 ) ) ;
#2091 = EDGE_CURVE ( 'NONE', #21646, #3260, #1328, .T. ) ;
#2092 = ORIENTED_EDGE ( 'NONE', *, *, #33477, .F. ) ;
#2093 = CARTESIAN_POINT ( 'NONE',  ( 11.05230858265422711, 17.66332026264438682, -26.82356531899860741 ) ) ;
#2094 = EDGE_LOOP ( 'NONE', ( #27297, #23033, #29887, #26081, #30239 ) ) ;
#2095 = CARTESIAN_POINT ( 'NONE',  ( -13.72572330278604014, 22.36032731891220848, -15.48384944483169257 ) ) ;
#2096 = CARTESIAN_POINT ( 'NONE',  ( -33.23893881994145261, -12.50319288011963081, 18.42518152272109688 ) ) ;
#2097 = CARTESIAN_POINT ( 'NONE',  ( -14.30862178846737187, 26.15670448022670413, 10.49999999999999822 ) ) ;
#2098 = CARTESIAN_POINT ( 'NONE',  ( 12.72840175812996755, 20.94423838021117845, -18.46516121132114208 ) ) ;
#2099 = EDGE_CURVE ( 'NONE', #16943, #29068, #7003, .T. ) ;
#2100 = ORIENTED_EDGE ( 'NONE', *, *, #6542, .T. ) ;
#2101 = CARTESIAN_POINT ( 'NONE',  ( 23.60227988993529280, -14.95294269409316001, -17.59782747150006443 ) ) ;
#2102 = EDGE_LOOP ( 'NONE', ( #14826, #14127, #27212, #32370, #31551, #19970, #30137 ) ) ;
#2104 = CYLINDRICAL_SURFACE ( 'NONE', #15357, 0.5000000000000004441 ) ;
#2103 = CARTESIAN_POINT ( 'NONE',  ( -15.14733410328086549, 27.40717930319807749, -6.405640806656524688 ) ) ;
#2105 = CARTESIAN_POINT ( 'NONE',  ( -12.40151229802639676, -20.21468385990432282, -20.38444596684770360 ) ) ;
#2106 = LINE ( 'NONE', #30731, #24355 ) ;
#2107 = ORIENTED_EDGE ( 'NONE', *, *, #6049, .T. ) ;
#2108 = CARTESIAN_POINT ( 'NONE',  ( -34.94561069989751445, -10.89217094161273103, -7.586357350432970215 ) ) ;
#2109 = CARTESIAN_POINT ( 'NONE',  ( -13.90572124313496971, -24.99301111420016497, -11.61183353183253253 ) ) ;
#2110 = AXIS2_PLACEMENT_3D ( 'NONE', #27906, #24264, #34407 ) ;
#2111 = CARTESIAN_POINT ( 'NONE',  ( 23.19735768193459791, -14.64350930037804055, 23.00000000000000000 ) ) ;
#2112 = VERTEX_POINT ( 'NONE', #13302 ) ;
#2113 = CARTESIAN_POINT ( 'NONE',  ( 20.51349737526394179, 3.099829992517171728, -26.98082256979993687 ) ) ;
#2114 = CARTESIAN_POINT ( 'NONE',  ( -8.247851828378241379, 9.985713325475984448, 10.49999999999999822 ) ) ;
#2115 = CARTESIAN_POINT ( 'NONE',  ( -34.33271597228890215, -24.82403720151341986, 11.00000000000000000 ) ) ;
#2116 = ORIENTED_EDGE ( 'NONE', *, *, #10994, .F. ) ;
#2117 = CARTESIAN_POINT ( 'NONE',  ( -30.06351586540304766, -0.04787271998934088807, -9.233772743391703841 ) ) ;
#2118 = CARTESIAN_POINT ( 'NONE',  ( 29.03390384994953521, -0.7637727643468541494, -12.46392547968639164 ) ) ;
#2119 = CARTESIAN_POINT ( 'NONE',  ( 29.86387254395472723, -6.221772116352023652, 19.66345542862529783 ) ) ;
#2120 = EDGE_CURVE ( 'NONE', #14734, #7713, #10266, .T. ) ;
#2121 = VERTEX_POINT ( 'NONE', #38498 ) ;
#2122 = CARTESIAN_POINT ( 'NONE',  ( -21.05807794215131068, 2.162551090963098943, -25.15387685026987796 ) ) ;
#2123 = EDGE_CURVE ( 'NONE', #22721, #18984, #35459, .T. ) ;
#2124 = CARTESIAN_POINT ( 'NONE',  ( -9.331903152615899089, 11.35703883385581037, 7.500000000000000888 ) ) ;
#2125 = DIRECTION ( 'NONE',  ( 1.000000000000000000, 0.000000000000000000, 0.000000000000000000 ) ) ;
#2126 = CARTESIAN_POINT ( 'NONE',  ( 0.5000000000000000000, 37.50000000000000711, 11.00000000000000000 ) ) ;
#2127 = DIRECTION ( 'NONE',  ( 1.000000000000000000, 0.000000000000000000, 0.000000000000000000 ) ) ;
#2128 = DIRECTION ( 'NONE',  ( 1.000000000000000000, 0.000000000000000000, 0.000000000000000000 ) ) ;
#2129 = CARTESIAN_POINT ( 'NONE',  ( -5.537946624085890335, 36.44027069998196566, 7.500000000000000888 ) ) ;
#2130 = VERTEX_POINT ( 'NONE', #25699 ) ;
#2131 = CARTESIAN_POINT ( 'NONE',  ( -20.93483025502773742, 5.035493566568158386, -23.14963160484778015 ) ) ;
#2132 = DIRECTION ( 'NONE',  ( -0.9510565162951504226, 0.3090169943749573322, 0.000000000000000000 ) ) ;
#2133 = CARTESIAN_POINT ( 'NONE',  ( -5.982165713378357452, 28.55918256678905465, 7.000000000000000000 ) ) ;
#2134 = CARTESIAN_POINT ( 'NONE',  ( 26.03909628386253061, -25.46251251313952935, -7.164779507717623730 ) ) ;
#2135 = CARTESIAN_POINT ( 'NONE',  ( -12.80736835487442349, 15.68301270189233954, 11.00000000000000000 ) ) ;
#2136 = DIRECTION ( 'NONE',  ( 0.8660254037844362651, -0.5000000000000041078, 0.000000000000000000 ) ) ;
#2137 = EDGE_CURVE ( 'NONE', #24274, #12134, #28093, .T. ) ;
#2138 = CARTESIAN_POINT ( 'NONE',  ( 11.58716084138019831, 19.70196545170939473, -21.55946877410309881 ) ) ;
#2139 = CIRCLE ( 'NONE', #34006, 0.4999999999999997780 ) ;
#2140 = CARTESIAN_POINT ( 'NONE',  ( 15.27443809246256734, -27.57253143578338594, 15.13084544680213561 ) ) ;
#2141 = VERTEX_POINT ( 'NONE', #38297 ) ;
#2142 = CARTESIAN_POINT ( 'NONE',  ( -16.33001031136068448, 22.49441389709989991, -8.808442500960499189 ) ) ;
#2143 = CARTESIAN_POINT ( 'NONE',  ( -25.35679574134486813, -6.615406304683630445, 20.82122704794080548 ) ) ;
#2144 = AXIS2_PLACEMENT_3D ( 'NONE', #27850, #9570, #15863 ) ;
#2145 = DIRECTION ( 'NONE',  ( 0.000000000000000000, 0.000000000000000000, 1.000000000000000000 ) ) ;
#2146 = CARTESIAN_POINT ( 'NONE',  ( 11.00857322187251164, 17.29338995577434446, -30.00000000000000000 ) ) ;
#2147 = ORIENTED_EDGE ( 'NONE', *, *, #34957, .F. ) ;
#2148 = CARTESIAN_POINT ( 'NONE',  ( 11.47989394144910058, 18.44111857959348200, -23.85327845104781019 ) ) ;
#2149 = ORIENTED_EDGE ( 'NONE', *, *, #28641, .F. ) ;
#2151 = DIRECTION ( 'NONE',  ( 1.000000000000000000, 0.000000000000000000, 0.000000000000000000 ) ) ;
#2150 = CARTESIAN_POINT ( 'NONE',  ( -14.46546301679569346, 25.16057478527850932, -11.58477129654782978 ) ) ;
#2152 = CARTESIAN_POINT ( 'NONE',  ( -14.95434924768307461, -25.85156499263970531, -9.704675056642397379 ) ) ;
#2153 = CARTESIAN_POINT ( 'NONE',  ( -32.84658669524026919, -23.46788009898592264, 10.99999999999981881 ) ) ;
#2154 = CIRCLE ( 'NONE', #24846, 1.000000000000011324 ) ;
#2155 = CARTESIAN_POINT ( 'NONE',  ( -18.86238051352358269, -11.38456432792228945, -24.21681366675842284 ) ) ;
#2156 = CARTESIAN_POINT ( 'NONE',  ( -11.57545763705510922, -25.81734924782649543, -5.000000000000000000 ) ) ;
#2157 = CARTESIAN_POINT ( 'NONE',  ( -23.43324262027537586, -8.134040356058612531, 20.99999999999999289 ) ) ;
#2158 = CARTESIAN_POINT ( 'NONE',  ( 12.88915114296325015, 19.83580132678993735, -19.58108076636484896 ) ) ;
#2159 = VERTEX_POINT ( 'NONE', #527 ) ;
#2160 = CARTESIAN_POINT ( 'NONE',  ( 24.92982005813157542, 6.438780434261885510, -8.860171362492041069 ) ) ;
#2161 = CARTESIAN_POINT ( 'NONE',  ( 17.34253826539385201, 27.32041144647958575, -13.70816084473008800 ) ) ;
#2162 = FACE_OUTER_BOUND ( 'NONE', #37524, .T. ) ;
#2163 = DIRECTION ( 'NONE',  ( 1.000000000000000000, 0.000000000000000000, 0.000000000000000000 ) ) ;
#2164 = VERTEX_POINT ( 'NONE', #12909 ) ;
#2165 = CARTESIAN_POINT ( 'NONE',  ( -23.09408679231368211, -0.7667527528709867646, -21.43583835363619983 ) ) ;
#2166 = CIRCLE ( 'NONE', #27461, 0.5000000000000004441 ) ;
#2167 = CARTESIAN_POINT ( 'NONE',  ( 21.72087342840458746, 0.6664541231550867861, -23.84654602765732179 ) ) ;
#2168 = DIRECTION ( 'NONE',  ( 0.000000000000000000, 0.000000000000000000, 1.000000000000000000 ) ) ;
#2169 = CARTESIAN_POINT ( 'NONE',  ( 20.82679397340719873, -18.60878629326332501, 20.82122704794080903 ) ) ;
#2170 = LINE ( 'NONE', #32449, #14167 ) ;
#2171 = CARTESIAN_POINT ( 'NONE',  ( -5.237540274239744775, 35.49300472853438038, 10.00000000000000000 ) ) ;
#2172 = EDGE_CURVE ( 'NONE', #17610, #9003, #24214, .T. ) ;
#2173 = CIRCLE ( 'NONE', #36555, 0.5000000000000004441 ) ;
#2174 = DIRECTION ( 'NONE',  ( -0.7431448254773962425, -0.6691306063588560171, 0.000000000000000000 ) ) ;
#2175 = MECHANICAL_DESIGN_GEOMETRIC_PRESENTATION_REPRESENTATION (  '', ( #39801 ), #30067 ) ;
#2176 = ORIENTED_EDGE ( 'NONE', *, *, #37827, .T. ) ;
#2177 = DIRECTION ( 'NONE',  ( -0.8090169943749426773, 0.5877852522924797984, 0.000000000000000000 ) ) ;
#2178 = AXIS2_PLACEMENT_3D ( 'NONE', #34148, #25386, #25790 ) ;
#2179 = CARTESIAN_POINT ( 'NONE',  ( -8.118377661053486349, 10.47536095541709145, 9.500000000000000000 ) ) ;
#2180 = CYLINDRICAL_SURFACE ( 'NONE', #4086, 0.5000000000000004441 ) ;
#2181 = CARTESIAN_POINT ( 'NONE',  ( 0.2177955101729588394, 20.58580882239673926, -28.44449306209597239 ) ) ;
#2182 = DIRECTION ( 'NONE',  ( -0.1045284632676570929, -0.9945218953682730678, 0.000000000000000000 ) ) ;
#2183 = DIRECTION ( 'NONE',  ( 0.2079116908177532363, -0.9781476007338070211, 6.938893903907217334E-15 ) ) ;
#2184 = DIRECTION ( 'NONE',  ( -0.6691306063588569053, 0.7431448254773954654, 0.000000000000000000 ) ) ;
#2185 = DIRECTION ( 'NONE',  ( -0.000000000000000000, -0.000000000000000000, -1.000000000000000000 ) ) ;
#2186 = FACE_OUTER_BOUND ( 'NONE', #17740, .T. ) ;
#2187 = ADVANCED_FACE ( 'NONE', ( #35052 ), #7206, .F. ) ;
#2188 = CARTESIAN_POINT ( 'NONE',  ( 18.23649648353778474, -16.09146789626167262, 23.00000000000000000 ) ) ;
#2189 = CARTESIAN_POINT ( 'NONE',  ( 14.58515322177743023, 27.60815066180548882, -8.705533694680715584 ) ) ;
#2190 = DIRECTION ( 'NONE',  ( 0.000000000000000000, 0.000000000000000000, 1.000000000000000000 ) ) ;
#2191 = ORIENTED_EDGE ( 'NONE', *, *, #28729, .T. ) ;
#2193 = DIRECTION ( 'NONE',  ( -0.000000000000000000, -0.000000000000000000, -1.000000000000000000 ) ) ;
#2192 = CARTESIAN_POINT ( 'NONE',  ( -17.80184909226064960, 15.08711156140914689, -15.89312851988550968 ) ) ;
#2194 = AXIS2_PLACEMENT_3D ( 'NONE', #5367, #11469, #14716 ) ;
#2195 = CARTESIAN_POINT ( 'NONE',  ( -13.52529089031622078, 27.94609563178166667, 10.49999999999999822 ) ) ;
#2196 = EDGE_CURVE ( 'NONE', #33602, #21186, #32001, .T. ) ;
#2197 = CARTESIAN_POINT ( 'NONE',  ( 14.90512858723619161, -25.84045694921644554, -9.707335597051320875 ) ) ;
#2198 = DIRECTION ( 'NONE',  ( 1.000000000000000000, 0.000000000000000000, 0.000000000000000000 ) ) ;
#2199 = CARTESIAN_POINT ( 'NONE',  ( 12.64006179627876314, 21.07329801286157434, -18.44930732498576376 ) ) ;
#2200 = CARTESIAN_POINT ( 'NONE',  ( 6.155076441694338207, 21.71698211341367113, -30.00000000000000000 ) ) ;
#2201 = CARTESIAN_POINT ( 'NONE',  ( 18.77248996150425597, -31.35432035810270435, 11.00000000000000178 ) ) ;
#2202 = MECHANICAL_DESIGN_GEOMETRIC_PRESENTATION_REPRESENTATION (  '', ( #9960 ), #2829 ) ;
#2203 = EDGE_CURVE ( 'NONE', #3338, #23748, #25511, .T. ) ;
#2204 = CARTESIAN_POINT ( 'NONE',  ( -24.39385489856421074, -19.12778200130764006, -14.77000471112758007 ) ) ;
#2205 = CARTESIAN_POINT ( 'NONE',  ( 1.706488926421375396, -23.94603835514126899, -11.88489013895719815 ) ) ;
#2206 = CARTESIAN_POINT ( 'NONE',  ( 11.17946636088399615, 17.33251866449996825, -28.08565060215844866 ) ) ;
#2207 = CARTESIAN_POINT ( 'NONE',  ( 17.93241811013781017, 10.94633007592474172, -24.41574245663013443 ) ) ;
#2208 = DIRECTION ( 'NONE',  ( 1.000000000000000000, 0.000000000000000000, 0.000000000000000000 ) ) ;
#2209 = EDGE_LOOP ( 'NONE', ( #14768, #4118, #23816 ) ) ;
#2210 = CARTESIAN_POINT ( 'NONE',  ( -6.555649915732293387, 32.00450200170969595, -12.95390610774645879 ) ) ;
#2211 = VERTEX_POINT ( 'NONE', #5571 ) ;
#2212 = AXIS2_PLACEMENT_3D ( 'NONE', #2423, #39983, #33313 ) ;
#2213 = CARTESIAN_POINT ( 'NONE',  ( -24.77298340259705256, 8.359746025953324278, 15.13084544680308419 ) ) ;
#2214 = ORIENTED_EDGE ( 'NONE', *, *, #1589, .T. ) ;
#2215 = CARTESIAN_POINT ( 'NONE',  ( -1.000000000000000000, 37.00000000000000711, 10.50000000000000178 ) ) ;
#2216 = CARTESIAN_POINT ( 'NONE',  ( 0.3762615568374529929, 19.56555719779890978, 12.00000000000000000 ) ) ;
#2217 = VERTEX_POINT ( 'NONE', #8019 ) ;
#2218 = CARTESIAN_POINT ( 'NONE',  ( -20.60288636730601297, 0.9732602012211746256, -28.08358842701117553 ) ) ;
#2219 = EDGE_CURVE ( 'NONE', #3881, #28480, #37836, .T. ) ;
#2220 = EDGE_LOOP ( 'NONE', ( #38643, #904, #30878, #30669 ) ) ;
#2221 = CARTESIAN_POINT ( 'NONE',  ( 35.51876124919839839, -10.74978321004375559, -5.000000000000007105 ) ) ;
#2222 = EDGE_CURVE ( 'NONE', #39268, #32514, #20343, .T. ) ;
#2223 = AXIS2_PLACEMENT_3D ( 'NONE', #19253, #22698, #772 ) ;
#2224 = ORIENTED_EDGE ( 'NONE', *, *, #668, .F. ) ;
#2225 = CARTESIAN_POINT ( 'NONE',  ( 11.03640989728592281, 29.14264673470096767, 13.00000000000000178 ) ) ;
#2226 = ORIENTED_EDGE ( 'NONE', *, *, #21195, .F. ) ;
#2227 = PLANE ( 'NONE',  #28118 ) ;
#2228 = CARTESIAN_POINT ( 'NONE',  ( 14.47283171447379146, 21.48159823030311344, 7.000000000000000000 ) ) ;
#2229 = DIRECTION ( 'NONE',  ( 1.000000000000000000, 0.000000000000000000, -0.000000000000000000 ) ) ;
#2230 = ORIENTED_EDGE ( 'NONE', *, *, #8735, .F. ) ;
#2231 = DIRECTION ( 'NONE',  ( -0.7071067811865489050, 0.000000000000000000, -0.7071067811865462405 ) ) ;
#2232 = DIRECTION ( 'NONE',  ( -0.000000000000000000, -0.000000000000000000, -1.000000000000000000 ) ) ;
#2233 = DIRECTION ( 'NONE',  ( -1.000000000000000000, 0.000000000000000000, 0.000000000000000000 ) ) ;
#2234 = EDGE_CURVE ( 'NONE', #11472, #6733, #8004, .T. ) ;
#2235 = CARTESIAN_POINT ( 'NONE',  ( 14.80471852002763100, 14.23397828709298629, -28.82854777094696885 ) ) ;
#2236 = CARTESIAN_POINT ( 'NONE',  ( 10.76129760716440487, 27.89257969453655051, -14.07744184314324620 ) ) ;
#2237 = AXIS2_PLACEMENT_3D ( 'NONE', #12110, #5609, #27348 ) ;
#2238 = ORIENTED_EDGE ( 'NONE', *, *, #8676, .T. ) ;
#2239 = CARTESIAN_POINT ( 'NONE',  ( -20.42711629762379744, 10.01608555171554471, -16.97676697675829871 ) ) ;
#2240 = DIRECTION ( 'NONE',  ( -0.000000000000000000, -0.000000000000000000, -1.000000000000000000 ) ) ;
#2241 = CARTESIAN_POINT ( 'NONE',  ( 12.63581098909226341, 27.45627467658428955, 7.000000000000000000 ) ) ;
#2242 = EDGE_CURVE ( 'NONE', #634, #15741, #10881, .T. ) ;
#2243 = CARTESIAN_POINT ( 'NONE',  ( 9.940439430138624743, -18.49387460801144911, -26.20988832591048734 ) ) ;
#2244 = CARTESIAN_POINT ( 'NONE',  ( -0.2474735156158440752, 16.63111439559750693, 13.00000000000000178 ) ) ;
#2245 = LINE ( 'NONE', #39607, #19188 ) ;
#2246 = CARTESIAN_POINT ( 'NONE',  ( -11.88487758710532027, 19.39000425891907042, -21.61563605934467702 ) ) ;
#2247 = CARTESIAN_POINT ( 'NONE',  ( 11.89833276060662115, -23.50684206517228603, -14.55647595399420169 ) ) ;
#2248 = CARTESIAN_POINT ( 'NONE',  ( 11.36213480545086441, 32.05769576588207315, 10.87262190629440717 ) ) ;
#2249 = ORIENTED_EDGE ( 'NONE', *, *, #12360, .F. ) ;
#2250 = ORIENTED_EDGE ( 'NONE', *, *, #9412, .T. ) ;
#2251 = CARTESIAN_POINT ( 'NONE',  ( -11.54439467976890654, 29.21207630366558305, -12.21176094404378354 ) ) ;
#2252 = CYLINDRICAL_SURFACE ( 'NONE', #30846, 0.5000000000000008882 ) ;
#2253 = CARTESIAN_POINT ( 'NONE',  ( -4.980911888400493481, 31.22871793335027490, 10.50000000000000533 ) ) ;
#2254 = VECTOR ( 'NONE', #6076, 1000.000000000000000 ) ;
#2255 = DIRECTION ( 'NONE',  ( -0.6123724356957908066, 0.3535533905932753962, 0.7071067811865500152 ) ) ;
#2256 = ORIENTED_EDGE ( 'NONE', *, *, #9432, .F. ) ;
#2257 = CARTESIAN_POINT ( 'NONE',  ( 30.83880836401509029, 0.02450782886024076290, -5.474181074949118653 ) ) ;
#2258 = CARTESIAN_POINT ( 'NONE',  ( -1.829593030691901284E-15, 22.50000000000001066, 0.000000000000000000 ) ) ;
#2259 = DIRECTION ( 'NONE',  ( 0.7886751345948049829, -0.2113248654051909647, 0.5773502691896350569 ) ) ;
#2260 = CARTESIAN_POINT ( 'NONE',  ( -7.530592408761010326, 11.28437794979203268, 9.500000000000000000 ) ) ;
#2261 = VERTEX_POINT ( 'NONE', #38704 ) ;
#2262 = AXIS2_PLACEMENT_3D ( 'NONE', #25496, #22248, #3767 ) ;
#2263 = CARTESIAN_POINT ( 'NONE',  ( -22.72401455592816077, 0.6329401436149191262, -21.62019267060189165 ) ) ;
#2264 = DIRECTION ( 'NONE',  ( 0.000000000000000000, 0.000000000000000000, 1.000000000000000000 ) ) ;
#2265 = ORIENTED_EDGE ( 'NONE', *, *, #21986, .F. ) ;
#2266 = CARTESIAN_POINT ( 'NONE',  ( 34.17835999317385642, -5.203673669061616991, -6.341916554725859356 ) ) ;
#2267 = AXIS2_PLACEMENT_3D ( 'NONE', #14457, #36006, #5316 ) ;
#2268 = CARTESIAN_POINT ( 'NONE',  ( 32.59722377598627219, -23.23978988006441782, 13.32518128616629305 ) ) ;
#2269 = ORIENTED_EDGE ( 'NONE', *, *, #23711, .T. ) ;
#2270 = CARTESIAN_POINT ( 'NONE',  ( 3.781581747449316744, 39.64129210796443203, 13.92931973827821146 ) ) ;
#2271 = EDGE_CURVE ( 'NONE', #14129, #36946, #30720, .T. ) ;
#2272 = LINE ( 'NONE', #11615, #35346 ) ;
#2273 = CARTESIAN_POINT ( 'NONE',  ( -17.00000000000000000, 22.50000000000000355, 10.00000000000000000 ) ) ;
#2274 = CARTESIAN_POINT ( 'NONE',  ( 5.140622461635829588, 27.93365566737693229, 20.82122704794079837 ) ) ;
#2275 = DIRECTION ( 'NONE',  ( 0.2079116908177535972, -0.9781476007338069101, 0.000000000000000000 ) ) ;
#2276 = EDGE_LOOP ( 'NONE', ( #38018, #7279, #33317, #4998 ) ) ;
#2277 = CARTESIAN_POINT ( 'NONE',  ( 7.014595103779619478, 35.79644522156321074, 10.49999999999999822 ) ) ;
#2278 = CARTESIAN_POINT ( 'NONE',  ( 3.161220354320216419, 12.43736188311278212, 10.49999999999999289 ) ) ;
#2279 = CIRCLE ( 'NONE', #27592, 6.000000000000005329 ) ;
#2280 = CARTESIAN_POINT ( 'NONE',  ( 7.040733923968011787, 36.25288937278184420, -7.575589961396375749 ) ) ;
#2281 = DIRECTION ( 'NONE',  ( 1.000000000000000000, 0.000000000000000000, 0.000000000000000000 ) ) ;
#2282 = CARTESIAN_POINT ( 'NONE',  ( 12.61496056324080683, 7.283250877003740520, 20.99999999999999645 ) ) ;
#2283 = B_SPLINE_CURVE_WITH_KNOTS ( 'NONE', 3,
 ( #3022, #18468, #15412, #21314, #20913, #39390 ),
 .UNSPECIFIED., .F., .F.,
 ( 4, 2, 4 ),
 ( 0.000000000000000000, 0.5000000000000000000, 1.000000000000000000 ),
 .UNSPECIFIED. ) ;
#2284 = CARTESIAN_POINT ( 'NONE',  ( 18.69514969737914001, -27.26850006250750624, -5.000000000000007105 ) ) ;
#2285 = CARTESIAN_POINT ( 'NONE',  ( -12.44178368932702661, 35.65276919562055014, 11.00000000000005684 ) ) ;
#2286 = AXIS2_PLACEMENT_3D ( 'NONE', #39508, #8231, #26524 ) ;
#2287 = CYLINDRICAL_SURFACE ( 'NONE', #25446, 1.000000000000000000 ) ;
#2288 = CARTESIAN_POINT ( 'NONE',  ( 4.780767545418608933, 35.69637305007220363, 9.500000000000000000 ) ) ;
#2289 = ORIENTED_EDGE ( 'NONE', *, *, #33735, .T. ) ;
#2290 = CARTESIAN_POINT ( 'NONE',  ( 10.89778913317478626, 17.36343269013392643, -30.00000000000000000 ) ) ;
#2291 = VERTEX_POINT ( 'NONE', #24067 ) ;
#2292 = VECTOR ( 'NONE', #37148, 1000.000000000000000 ) ;
#2293 = CARTESIAN_POINT ( 'NONE',  ( -15.39107358607109610, 26.18243249704805820, -7.359043735441920475 ) ) ;
#2294 = AXIS2_PLACEMENT_3D ( 'NONE', #7981, #19987, #23433 ) ;
#2295 = CARTESIAN_POINT ( 'NONE',  ( -30.59707569446036501, -4.299442758149942811, 18.87996532025748309 ) ) ;
#2296 = ADVANCED_FACE ( 'NONE', ( #39301 ), #8223, .T. ) ;
#2297 = CARTESIAN_POINT ( 'NONE',  ( -2.525645716490711123, 8.212903943950955465, 11.00000000000000000 ) ) ;
#2298 = CARTESIAN_POINT ( 'NONE',  ( 11.54739967089177810, 18.38288522691597748, -23.86353388501674644 ) ) ;
#2299 = ORIENTED_EDGE ( 'NONE', *, *, #4556, .T. ) ;
#2300 = CARTESIAN_POINT ( 'NONE',  ( 25.52108459349270930, -16.17540792513675640, -15.67991740391578048 ) ) ;
#2301 = EDGE_LOOP ( 'NONE', ( #10276, #6341, #12281, #38075, #5978, #11958, #32596 ) ) ;
#2303 = LINE ( 'NONE', #4945, #38709 ) ;
#2302 = CARTESIAN_POINT ( 'NONE',  ( -14.04492652393572527, 25.09326306025475972, -12.49859865225124267 ) ) ;
#2304 = CARTESIAN_POINT ( 'NONE',  ( -17.46439735134465820, -26.04403205724830528, -10.03879580357975421 ) ) ;
#2305 = DIRECTION ( 'NONE',  ( 0.5877852522924689183, -0.8090169943749505599, -0.000000000000000000 ) ) ;
#2306 = VERTEX_POINT ( 'NONE', #26711 ) ;
#2307 = CARTESIAN_POINT ( 'NONE',  ( -21.45327189537562518, -7.409941418364766719, -23.09511941793392253 ) ) ;
#2308 = CARTESIAN_POINT ( 'NONE',  ( -14.88933002184502108, -26.10237849226964002, -8.769526409485358442 ) ) ;
#2309 = CARTESIAN_POINT ( 'NONE',  ( 23.43324262027504190, -8.134040356058543253, 23.00000000000000000 ) ) ;
#2310 = ORIENTED_EDGE ( 'NONE', *, *, #1930, .T. ) ;
#2311 = CARTESIAN_POINT ( 'NONE',  ( 20.29617916935422528, 3.110535768804490786, -28.77477341303289293 ) ) ;
#2312 = CARTESIAN_POINT ( 'NONE',  ( -8.172817770806704019, 10.40043057260432668, 10.99387789255784043 ) ) ;
#2313 = LINE ( 'NONE', #29934, #33589 ) ;
#2314 = ORIENTED_EDGE ( 'NONE', *, *, #13952, .F. ) ;
#2315 = CARTESIAN_POINT ( 'NONE',  ( -30.08515734786159967, -0.07135867236674159342, -9.232266537557617170 ) ) ;
#2316 = ORIENTED_EDGE ( 'NONE', *, *, #21883, .F. ) ;
#2317 = CARTESIAN_POINT ( 'NONE',  ( 20.73387816077086399, 0.03120835422459670647, -27.39522693578182455 ) ) ;
#2318 = CARTESIAN_POINT ( 'NONE',  ( 31.03731131719052883, -12.30244853585591969, 19.66345542862526230 ) ) ;
#2319 = EDGE_CURVE ( 'NONE', #29659, #34986, #18402, .T. ) ;
#2320 = ORIENTED_EDGE ( 'NONE', *, *, #20865, .T. ) ;
#2321 = CARTESIAN_POINT ( 'NONE',  ( -20.33089032344865998, 3.598786340304104048, -27.59557066844887174 ) ) ;
#2322 = VECTOR ( 'NONE', #1694, 1000.000000000000000 ) ;
#2323 = DIRECTION ( 'NONE',  ( -0.000000000000000000, -0.000000000000000000, -1.000000000000000000 ) ) ;
#2324 = DIRECTION ( 'NONE',  ( -0.8090169943749504489, -0.5877852522924690293, 0.000000000000000000 ) ) ;
#2325 = CIRCLE ( 'NONE', #27599, 1.000000000000000000 ) ;
#2326 = CIRCLE ( 'NONE', #34739, 0.4999999999999998335 ) ;
#2327 = LINE ( 'NONE', #27101, #3162 ) ;
#2328 = EDGE_CURVE ( 'NONE', #35366, #11163, #36460, .T. ) ;
#2329 = DIRECTION ( 'NONE',  ( 1.000000000000000000, 0.000000000000000000, 0.000000000000000000 ) ) ;
#2330 = EDGE_CURVE ( 'NONE', #31697, #24869, #30927, .T. ) ;
#2331 = CARTESIAN_POINT ( 'NONE',  ( 6.440829913680675034, 10.60893893836775348, 12.00000000000000000 ) ) ;
#2332 = CARTESIAN_POINT ( 'NONE',  ( -5.265294543811100070, 36.54569740949598611, 7.381627713044570882 ) ) ;
#2333 = ORIENTED_EDGE ( 'NONE', *, *, #950, .F. ) ;
#2334 = CARTESIAN_POINT ( 'NONE',  ( -20.08579387813589179, 4.300271612531742171, -28.80311731544902187 ) ) ;
#2335 = DIRECTION ( 'NONE',  ( -0.3090169943749560000, -0.9510565162951507556, 0.000000000000000000 ) ) ;
#2336 = CARTESIAN_POINT ( 'NONE',  ( -4.817371740575545402, 23.83900317890010001, 20.99999999999999645 ) ) ;
#2337 = CARTESIAN_POINT ( 'NONE',  ( 25.39385983464903873, -24.87502355768076967, -8.913805553225882861 ) ) ;
#2338 = DIRECTION ( 'NONE',  ( 0.000000000000000000, 0.000000000000000000, -1.000000000000000000 ) ) ;
#2339 = DIRECTION ( 'NONE',  ( 0.000000000000000000, 0.000000000000000000, 1.000000000000000000 ) ) ;
#2340 = CARTESIAN_POINT ( 'NONE',  ( 11.15208866170259761, 18.71877292872446574, -23.80158545199737574 ) ) ;
#2341 = CARTESIAN_POINT ( 'NONE',  ( 10.10865978838830515, -27.35622988134924327, 12.14047268033177573 ) ) ;
#2342 = ORIENTED_EDGE ( 'NONE', *, *, #2684, .F. ) ;
#2343 = CARTESIAN_POINT ( 'NONE',  ( -16.95359871692699727, 21.80622970928592608, -6.428279578752638557 ) ) ;
#2344 = CARTESIAN_POINT ( 'NONE',  ( -26.53285431386355597, -6.841436363529350473, 20.69868183039763210 ) ) ;
#2345 = EDGE_CURVE ( 'NONE', #7792, #11093, #26828, .T. ) ;
#2346 = EDGE_CURVE ( 'NONE', #8691, #659, #11082, .T. ) ;
#2347 = DIRECTION ( 'NONE',  ( 0.000000000000000000, 0.000000000000000000, 1.000000000000000000 ) ) ;
#2348 = CARTESIAN_POINT ( 'NONE',  ( 15.18952781818666331, 26.23141474697915498, -8.298106924336673629 ) ) ;
#2349 = ORIENTED_EDGE ( 'NONE', *, *, #17055, .T. ) ;
#2350 = CARTESIAN_POINT ( 'NONE',  ( 6.282361020112160688, 14.70372268239673197, 10.50000000000000000 ) ) ;
#2351 = EDGE_LOOP ( 'NONE', ( #18823, #14815, #1312, #20592 ) ) ;
#2352 = VECTOR ( 'NONE', #2496, 1000.000000000000000 ) ;
#2354 = DIRECTION ( 'NONE',  ( -0.9510565162951540863, -0.3090169943749457304, 0.000000000000000000 ) ) ;
#2353 = CARTESIAN_POINT ( 'NONE',  ( -14.79703636326500060, 25.74263473257225243, -10.17218918890135271 ) ) ;
#2355 = CARTESIAN_POINT ( 'NONE',  ( -12.71873048370224346, -22.55951204540982147, -16.43669669196557237 ) ) ;
#2356 = CARTESIAN_POINT ( 'NONE',  ( 7.983541495324169013, 10.37739674670157441, 10.83333333333332860 ) ) ;
#2357 = VECTOR ( 'NONE', #20692, 1000.000000000000114 ) ;
#2358 = CARTESIAN_POINT ( 'NONE',  ( -17.77200783866643263, -10.72547896874518258, -27.70459291383746248 ) ) ;
#2359 = CARTESIAN_POINT ( 'NONE',  ( -4.746940016115302363, -20.05784295341780776, -27.67719817960474415 ) ) ;
#2360 = CARTESIAN_POINT ( 'NONE',  ( 5.132330917503148626, 36.34800796123236211, 10.49999999999999822 ) ) ;
#2361 = CARTESIAN_POINT ( 'NONE',  ( 13.38699610197189571, 19.18010719891643845, -19.66077882286520406 ) ) ;
#2362 = ORIENTED_EDGE ( 'NONE', *, *, #8529, .F. ) ;
#2363 = CARTESIAN_POINT ( 'NONE',  ( 24.20446040187360026, 7.319688609815201197, -9.361820473650304564 ) ) ;
#2364 = VECTOR ( 'NONE', #30625, 1000.000000000000000 ) ;
#2365 = DIRECTION ( 'NONE',  ( 0.000000000000000000, 0.000000000000000000, 1.000000000000000000 ) ) ;
#2366 = DIRECTION ( 'NONE',  ( 1.000000000000000000, 0.000000000000000000, 0.000000000000000000 ) ) ;
#2367 = CARTESIAN_POINT ( 'NONE',  ( -11.39464589777670867, 26.66807349098043289, 13.00000000000000178 ) ) ;
#2368 = EDGE_LOOP ( 'NONE', ( #6099, #35990, #11275 ) ) ;
#2369 = CARTESIAN_POINT ( 'NONE',  ( -27.18895464093139935, -0.8152009208677085672, -15.32376075612282662 ) ) ;
#2370 = CARTESIAN_POINT ( 'NONE',  ( 25.89641589905429697, 0.2649541786267404220, -16.43670733185422961 ) ) ;
#2371 = CARTESIAN_POINT ( 'NONE',  ( 2.568190708544435541, 12.82247983807080871, 10.50000000000000000 ) ) ;
#2372 = CARTESIAN_POINT ( 'NONE',  ( 22.04303751225581465, -17.34387783897721746, 20.94377226548377280 ) ) ;
#2373 = ADVANCED_FACE ( 'NONE', ( #35857 ), #9693, .T. ) ;
#2374 = CARTESIAN_POINT ( 'NONE',  ( 35.84808252048253507, -3.038699442442316379, -13.99876745781542553 ) ) ;
#2375 = CARTESIAN_POINT ( 'NONE',  ( 37.51589702892713518, -12.89337557385772470, 11.00000000000017053 ) ) ;
#2376 = ORIENTED_EDGE ( 'NONE', *, *, #23048, .T. ) ;
#2377 = DIRECTION ( 'NONE',  ( -0.000000000000000000, -0.000000000000000000, 1.000000000000000000 ) ) ;
#2378 = LINE ( 'NONE', #36106, #16885 ) ;
#2379 = ORIENTED_EDGE ( 'NONE', *, *, #27745, .F. ) ;
#2380 = CARTESIAN_POINT ( 'NONE',  ( 1.572519005230682332, 38.31547560893784521, -6.276489886563880738 ) ) ;
#2381 = CARTESIAN_POINT ( 'NONE',  ( 8.304868622281791346, 28.96851274765995043, 10.75000000000000178 ) ) ;
#2382 = AXIS2_PLACEMENT_3D ( 'NONE', #33788, #30538, #23830 ) ;
#2383 = CYLINDRICAL_SURFACE ( 'NONE', #24691, 0.4999999999999997780 ) ;
#2384 = DIRECTION ( 'NONE',  ( 1.000000000000000000, 0.000000000000000000, 0.000000000000000000 ) ) ;
#2385 = CARTESIAN_POINT ( 'NONE',  ( -2.525645716490710679, 8.212903943950959018, 9.000000000000001776 ) ) ;
#2386 = DIRECTION ( 'NONE',  ( 1.000000000000000000, 0.000000000000000000, 0.000000000000000000 ) ) ;
#2387 = CARTESIAN_POINT ( 'NONE',  ( 14.48927117870126580, -30.61587158504672601, 11.00000000000000000 ) ) ;
#2388 = CARTESIAN_POINT ( 'NONE',  ( 14.62822902851280027, 28.63951968782866331, -6.846782395405623056 ) ) ;
#2389 = CARTESIAN_POINT ( 'NONE',  ( -7.249505266586148799, 35.63236627514445587, 7.102637441331451029 ) ) ;
#2390 = VERTEX_POINT ( 'NONE', #12272 ) ;
#2392 = DIRECTION ( 'NONE',  ( 1.000000000000000000, 0.000000000000000000, 0.000000000000000000 ) ) ;
#2391 = CARTESIAN_POINT ( 'NONE',  ( -16.28833159386192975, 13.37804228123318318, -24.36285121532279518 ) ) ;
#2393 = CARTESIAN_POINT ( 'NONE',  ( -13.72389693702418789, 27.48489553602896152, 10.99387789255782977 ) ) ;
#2394 = CARTESIAN_POINT ( 'NONE',  ( 15.25261056305548735, -26.39471828263916109, -7.827771010459708911 ) ) ;
#2395 = EDGE_CURVE ( 'NONE', #16360, #21859, #32017, .T. ) ;
#2396 = CARTESIAN_POINT ( 'NONE',  ( 14.53140152873307578, 24.97328356840179353, -11.59890379914566338 ) ) ;
#2397 = CARTESIAN_POINT ( 'NONE',  ( 11.87877828677522984, 19.39653357432699821, -21.61446414259498994 ) ) ;
#2398 = VERTEX_POINT ( 'NONE', #40095 ) ;
#2399 = CARTESIAN_POINT ( 'NONE',  ( -28.79410123593970638, 4.962698632456613801, -4.999999999999999112 ) ) ;
#2400 = CARTESIAN_POINT ( 'NONE',  ( -12.49038105676665644, 14.13397459621567798, 10.50000000000000000 ) ) ;
#2401 = CARTESIAN_POINT ( 'NONE',  ( -29.70272037912319263, -23.25111303184518619, -6.708336780241142883 ) ) ;
#2402 = CARTESIAN_POINT ( 'NONE',  ( 4.201337036921611201, -20.08771302450454499, -28.83765527686704999 ) ) ;
#2403 = CARTESIAN_POINT ( 'NONE',  ( 11.68239538796815147, 18.26559943105741723, -23.88377865820274693 ) ) ;
#2404 = CARTESIAN_POINT ( 'NONE',  ( 18.51501374778856146, 10.35893760720515466, -23.33396074953557431 ) ) ;
#2405 = DIRECTION ( 'NONE',  ( -0.000000000000000000, 1.000000000000000000, -0.000000000000000000 ) ) ;
#2406 = CARTESIAN_POINT ( 'NONE',  ( -5.159834554421613539, 22.03625837824066025, -23.14505616485400807 ) ) ;
#2407 = ORIENTED_EDGE ( 'NONE', *, *, #25596, .F. ) ;
#2408 = AXIS2_PLACEMENT_3D ( 'NONE', #8042, #29380, #32027 ) ;
#2409 = VECTOR ( 'NONE', #14283, 999.9999999999998863 ) ;
#2410 = CARTESIAN_POINT ( 'NONE',  ( -27.61482536621095818, 3.986323854238359665, 15.72805884749610428 ) ) ;
#2411 = VERTEX_POINT ( 'NONE', #36857 ) ;
#2412 = CYLINDRICAL_SURFACE ( 'NONE', #8262, 0.5000000000000007772 ) ;
#2413 = DIRECTION ( 'NONE',  ( 0.9945218953682729568, -0.1045284632676569680, 0.000000000000000000 ) ) ;
#2414 = CARTESIAN_POINT ( 'NONE',  ( -22.18768002425451513, 0.7994764990569520613, -22.75141326800756403 ) ) ;
#2415 = EDGE_CURVE ( 'NONE', #37418, #855, #9628, .T. ) ;
#2416 = CARTESIAN_POINT ( 'NONE',  ( 29.06859794668536878, -9.700207295447865974, -14.81230389778934686 ) ) ;
#2417 = AXIS2_PLACEMENT_3D ( 'NONE', #526, #36711, #8874 ) ;
#2418 = EDGE_CURVE ( 'NONE', #38453, #6898, #12465, .T. ) ;
#2419 = VERTEX_POINT ( 'NONE', #22008 ) ;
#2420 = EDGE_CURVE ( 'NONE', #39537, #15928, #2763, .T. ) ;
#2421 = FACE_OUTER_BOUND ( 'NONE', #4819, .T. ) ;
#2422 = EDGE_LOOP ( 'NONE', ( #33879, #4411 ) ) ;
#2423 = CARTESIAN_POINT ( 'NONE',  ( -11.11016527260153630, 31.83082137946488643, 11.00000000000000000 ) ) ;
#2424 = CARTESIAN_POINT ( 'NONE',  ( 14.36830325120613594, 20.48707633493483371, 7.000000000000000000 ) ) ;
#2425 = EDGE_CURVE ( 'NONE', #21186, #24692, #4710, .T. ) ;
#2426 = DIRECTION ( 'NONE',  ( -0.8660254037844425934, -0.4999999999999933942, -3.469446951953613400E-15 ) ) ;
#2427 = ORIENTED_EDGE ( 'NONE', *, *, #7350, .T. ) ;
#2428 = DIRECTION ( 'NONE',  ( 0.000000000000000000, 0.000000000000000000, -1.000000000000000000 ) ) ;
#2429 = CARTESIAN_POINT ( 'NONE',  ( 2.835130509701798918, 15.55077355964573904, 12.00000000000000000 ) ) ;
#2430 = CARTESIAN_POINT ( 'NONE',  ( -3.460024211650461368, 26.15060946995401281, 23.00000000000000355 ) ) ;
#2431 = CARTESIAN_POINT ( 'NONE',  ( 19.75762832862930907, -16.14151280411838130, -19.70786949030270208 ) ) ;
#2432 = CARTESIAN_POINT ( 'NONE',  ( 15.76482823105918385, 13.10325120709816105, -30.00000000000000711 ) ) ;
#2433 = VECTOR ( 'NONE', #10649, 1000.000000000000000 ) ;
#2434 = CARTESIAN_POINT ( 'NONE',  ( 11.57904490959511712, 30.10906470480531638, -11.27760544223991346 ) ) ;
#2435 = CONICAL_SURFACE ( 'NONE', #40029, 1.000000000000002665, 0.7853981633974476129 ) ;
#2436 = VERTEX_POINT ( 'NONE', #34013 ) ;
#2437 = CARTESIAN_POINT ( 'NONE',  ( -21.75201666326742966, 11.73857275933465871, -6.939711857671738038 ) ) ;
#2438 = CYLINDRICAL_SURFACE ( 'NONE', #24230, 6.000000000000006217 ) ;
#2439 = CARTESIAN_POINT ( 'NONE',  ( -14.70623423376111738, 19.54590544129804286, 7.000000000000000000 ) ) ;
#2440 = CARTESIAN_POINT ( 'NONE',  ( 15.74830575105852226, -26.80738400109229147, -5.472937640529008441 ) ) ;
#2441 = CARTESIAN_POINT ( 'NONE',  ( -11.11016527260153808, 31.83082137946488643, 7.000000000000000000 ) ) ;
#2442 = EDGE_CURVE ( 'NONE', #7574, #1553, #9426, .T. ) ;
#2443 = AXIS2_PLACEMENT_3D ( 'NONE', #1981, #39536, #36496 ) ;
#2444 = ADVANCED_FACE ( 'NONE', ( #18769 ), #33626, .F. ) ;
#2445 = CARTESIAN_POINT ( 'NONE',  ( 13.30736835487433289, 15.68301270189216545, 7.499999999999997335 ) ) ;
#2446 = ADVANCED_FACE ( 'NONE', ( #27312 ), #11874, .F. ) ;
#2447 = CIRCLE ( 'NONE', #3107, 1.000000000000000000 ) ;
#2448 = CARTESIAN_POINT ( 'NONE',  ( -14.01060747619464486, 23.98181712051333747, -13.50887074865789828 ) ) ;
#2449 = CARTESIAN_POINT ( 'NONE',  ( -23.04127009990159891, -25.77385733438709892, -8.962383121669381225 ) ) ;
#2450 = CARTESIAN_POINT ( 'NONE',  ( 8.986720564395060507, -19.19316913704046001, -25.11960455031415407 ) ) ;
#2451 = DIRECTION ( 'NONE',  ( 0.000000000000000000, 0.000000000000000000, 1.000000000000000000 ) ) ;
#2452 = VERTEX_POINT ( 'NONE', #31158 ) ;
#2453 = ORIENTED_EDGE ( 'NONE', *, *, #21012, .T. ) ;
#2454 = CARTESIAN_POINT ( 'NONE',  ( -10.29087960479974839, 28.35764963828314933, -14.04442573278240403 ) ) ;
#2455 = DIRECTION ( 'NONE',  ( 1.000000000000000000, -6.938893903907203923E-15, 0.000000000000000000 ) ) ;
#2456 = CARTESIAN_POINT ( 'NONE',  ( -11.14717238216079842, 32.53695909538301123, 7.000000000000000000 ) ) ;
#2457 = DIRECTION ( 'NONE',  ( -0.3090169943749450643, 0.9510565162951544194, -0.000000000000000000 ) ) ;
#2458 = ORIENTED_EDGE ( 'NONE', *, *, #16442, .T. ) ;
#2459 = CARTESIAN_POINT ( 'NONE',  ( 25.81175492159683316, 0.4056748218298066311, -16.45145585693692070 ) ) ;
#2460 = CARTESIAN_POINT ( 'NONE',  ( 14.47283171447379146, 21.48159823030312054, 11.00000000000000000 ) ) ;
#2461 = FACE_OUTER_BOUND ( 'NONE', #37369, .T. ) ;
#2462 = AXIS2_PLACEMENT_3D ( 'NONE', #20972, #17935, #36411 ) ;
#2463 = ORIENTED_EDGE ( 'NONE', *, *, #32019, .T. ) ;
#2464 = CARTESIAN_POINT ( 'NONE',  ( -30.83932063798821943, -0.01157433484235278337, -5.946084096651039985 ) ) ;
#2465 = LINE ( 'NONE', #18700, #39083 ) ;
#2466 = EDGE_CURVE ( 'NONE', #31286, #37934, #39893, .T. ) ;
#2467 = ORIENTED_EDGE ( 'NONE', *, *, #25481, .F. ) ;
#2468 = CARTESIAN_POINT ( 'NONE',  ( 20.56644879191631858, -2.251167489236703734, -27.92353585182003428 ) ) ;
#2469 = CARTESIAN_POINT ( 'NONE',  ( 34.36757128605636069, -1.941376724489949579, 13.92931973827832159 ) ) ;
#2470 = ADVANCED_FACE ( 'NONE', ( #6362 ), #6171, .T. ) ;
#2471 = EDGE_LOOP ( 'NONE', ( #23597, #2040, #13074 ) ) ;
#2472 = CARTESIAN_POINT ( 'NONE',  ( 10.37941170769460975, 36.15788802554214953, 14.53008259254011136 ) ) ;
#2473 = AXIS2_PLACEMENT_3D ( 'NONE', #36146, #39384, #10966 ) ;
#2474 = CARTESIAN_POINT ( 'NONE',  ( -17.21213525676645162, -20.06193531423545551, 20.50957957746029336 ) ) ;
#2475 = CARTESIAN_POINT ( 'NONE',  ( 1.590043107810626966, 12.61456814725305975, 10.00000000000000000 ) ) ;
#2476 = CARTESIAN_POINT ( 'NONE',  ( 7.420252307063369024, 30.34362403113780715, 19.99202127657103745 ) ) ;
#2477 = CIRCLE ( 'NONE', #16063, 15.00000000000000000 ) ;
#2478 = DIRECTION ( 'NONE',  ( 1.000000000000000000, 0.000000000000000000, 0.000000000000000000 ) ) ;
#2479 = ORIENTED_EDGE ( 'NONE', *, *, #31714, .F. ) ;
#2480 = FACE_OUTER_BOUND ( 'NONE', #621, .T. ) ;
#2481 = CARTESIAN_POINT ( 'NONE',  ( 5.644276917315719899, 36.40655018617690786, 7.000000000000000000 ) ) ;
#2482 = CARTESIAN_POINT ( 'NONE',  ( 4.284595636533838459, 26.24047331256504734, -18.68436667907231552 ) ) ;
#2483 = CARTESIAN_POINT ( 'NONE',  ( -1.247473515615844075, 16.63111439559750693, 12.00000000000000000 ) ) ;
#2484 = CARTESIAN_POINT ( 'NONE',  ( 20.63240589120021795, -1.802217369567702843, 20.82122704794562296 ) ) ;
#2485 = CARTESIAN_POINT ( 'NONE',  ( 15.23343791758566823, -20.13306411397316609, -19.07499260615857395 ) ) ;
#2486 = LINE ( 'NONE', #38855, #36613 ) ;
#2487 = CARTESIAN_POINT ( 'NONE',  ( -8.796116341590805021, 23.42450908139092647, 7.000000000000000000 ) ) ;
#2488 = CARTESIAN_POINT ( 'NONE',  ( 14.63635198741554788, 25.78286467897733303, 7.000000000000000000 ) ) ;
#2489 = ORIENTED_EDGE ( 'NONE', *, *, #37153, .T. ) ;
#2490 = CARTESIAN_POINT ( 'NONE',  ( 12.62004824291777005, 21.10321597694743545, -18.44487059424978170 ) ) ;
#2491 = VECTOR ( 'NONE', #7848, 1000.000000000000000 ) ;
#2492 = ORIENTED_EDGE ( 'NONE', *, *, #20432, .T. ) ;
#2494 = VECTOR ( 'NONE', #31133, 1000.000000000000000 ) ;
#2493 = CARTESIAN_POINT ( 'NONE',  ( -12.41076023834438047, 19.59308009719089583, -20.58983577532683285 ) ) ;
#2495 = CARTESIAN_POINT ( 'NONE',  ( -24.23816072143619493, -22.57437281311074528, 19.27171037444157164 ) ) ;
#2496 = DIRECTION ( 'NONE',  ( -0.000000000000000000, -0.000000000000000000, 1.000000000000000000 ) ) ;
#2497 = CARTESIAN_POINT ( 'NONE',  ( 13.83252988835445230, 23.26147414863088514, -14.48414622511842786 ) ) ;
#2498 = ORIENTED_EDGE ( 'NONE', *, *, #169, .F. ) ;
#2499 = CARTESIAN_POINT ( 'NONE',  ( 20.86300852440544418, -13.20907702042890186, -20.69370547666579441 ) ) ;
#2500 = VERTEX_POINT ( 'NONE', #25057 ) ;
#2501 = CIRCLE ( 'NONE', #5737, 16.99999999999999645 ) ;
#2503 = CARTESIAN_POINT ( 'NONE',  ( 0.000000000000000000, 22.50000000000000355, 7.000000000000000000 ) ) ;
#2502 = CARTESIAN_POINT ( 'NONE',  ( -14.85775003842022102, 28.53279358564904555, -5.000000000000001776 ) ) ;
#2504 = CARTESIAN_POINT ( 'NONE',  ( -10.81924648548876355, -18.06583327712415254, -26.12370104260517678 ) ) ;
#2505 = LINE ( 'NONE', #14485, #7498 ) ;
#2506 = AXIS2_PLACEMENT_3D ( 'NONE', #26784, #20297, #27385 ) ;
#2507 = VERTEX_POINT ( 'NONE', #24458 ) ;
#2508 = CARTESIAN_POINT ( 'NONE',  ( -35.48442078681456024, -11.08901139838818040, -5.000000000000004441 ) ) ;
#2509 = CARTESIAN_POINT ( 'NONE',  ( -9.513019653046374202, -18.52389691873554156, -26.84529393937997099 ) ) ;
#2510 = CARTESIAN_POINT ( 'NONE',  ( 14.03781671904272521, 27.78639141342386765, 7.485646746502379933 ) ) ;
#2511 = ORIENTED_EDGE ( 'NONE', *, *, #38179, .T. ) ;
#2512 = CARTESIAN_POINT ( 'NONE',  ( 29.78831017271203763, 1.106291696078458120, -5.473890122755831200 ) ) ;
#2513 = CARTESIAN_POINT ( 'NONE',  ( -7.773262162581324297, 10.11013643092551284, 10.49999999999999822 ) ) ;
#2514 = CARTESIAN_POINT ( 'NONE',  ( -18.77248997590677604, -31.35432035705904497, 23.00000000000094147 ) ) ;
#2515 = VERTEX_POINT ( 'NONE', #15316 ) ;
#2516 = CARTESIAN_POINT ( 'NONE',  ( -30.41772674068107918, -0.07296283099214972978, -8.294073688046619708 ) ) ;
#2517 = EDGE_LOOP ( 'NONE', ( #30775, #35673 ) ) ;
#2518 = CARTESIAN_POINT ( 'NONE',  ( 21.84932286874548879, -0.09515477611452517748, -23.75395710783811865 ) ) ;
#2519 = CARTESIAN_POINT ( 'NONE',  ( 33.25367603494935764, -15.60696645161989160, 17.92354375535251521 ) ) ;
#2520 = ORIENTED_EDGE ( 'NONE', *, *, #18562, .T. ) ;
#2521 = CARTESIAN_POINT ( 'NONE',  ( -27.27092024678508153, 3.518473056539207722, -8.338086808340122502 ) ) ;
#2522 = CARTESIAN_POINT ( 'NONE',  ( -19.48557158514988785, -11.24999999999987743, 10.00000000000000000 ) ) ;
#2523 = DIRECTION ( 'NONE',  ( 0.4999999999999933942, -0.8660254037844425934, 0.000000000000000000 ) ) ;
#2524 = AXIS2_PLACEMENT_3D ( 'NONE', #26370, #19881, #32270 ) ;
#2525 = CIRCLE ( 'NONE', #4459, 15.00000000000000000 ) ;
#2526 = CARTESIAN_POINT ( 'NONE',  ( 12.80736835487433289, 15.68301270189216545, 7.000000000000000000 ) ) ;
#2527 = PLANE ( 'NONE',  #33778 ) ;
#2528 = AXIS2_PLACEMENT_3D ( 'NONE', #9213, #25433, #15701 ) ;
#2529 = FACE_BOUND ( 'NONE', #10441, .T. ) ;
#2530 = CARTESIAN_POINT ( 'NONE',  ( -6.576253646258509278, 14.29921418520934218, 10.50000000000000000 ) ) ;
#2531 = ORIENTED_EDGE ( 'NONE', *, *, #35614, .T. ) ;
#2532 = CARTESIAN_POINT ( 'NONE',  ( -24.09052910358969157, 6.077159936355657877, -12.79381164378030533 ) ) ;
#2533 = DIRECTION ( 'NONE',  ( 0.000000000000000000, 0.000000000000000000, 1.000000000000000000 ) ) ;
#2534 = CARTESIAN_POINT ( 'NONE',  ( -3.399837471815634338, 8.909889435135630364, 7.499999999999997335 ) ) ;
#2535 = CARTESIAN_POINT ( 'NONE',  ( 15.61423674409565265, -15.29117231345428252, -24.39877605513977343 ) ) ;
#2536 = DIRECTION ( 'NONE',  ( -0.2079116908177663092, -0.9781476007338041345, 0.000000000000000000 ) ) ;
#2537 = CARTESIAN_POINT ( 'NONE',  ( 14.81862396006678750, 26.15963469534062469, -9.689294582542693490 ) ) ;
#2538 = CARTESIAN_POINT ( 'NONE',  ( 4.264734420589964944E-14, -26.44091005802452798, 13.32518128616608877 ) ) ;
#2539 = VERTEX_POINT ( 'NONE', #18372 ) ;
#2540 = CARTESIAN_POINT ( 'NONE',  ( -14.72765650035312035, 19.61305159137336673, -16.65999048068721677 ) ) ;
#2541 = CARTESIAN_POINT ( 'NONE',  ( -17.83459896181207682, -17.64923967996745446, 20.94377226548378346 ) ) ;
#2542 = EDGE_CURVE ( 'NONE', #20981, #36487, #18572, .T. ) ;
#2543 = CARTESIAN_POINT ( 'NONE',  ( -5.184280209938394002, 31.68549066217158483, 10.50000000000000000 ) ) ;
#2544 = CARTESIAN_POINT ( 'NONE',  ( 11.14342221288931967, 17.60014963584713499, -26.83212941470313240 ) ) ;
#2545 = ORIENTED_EDGE ( 'NONE', *, *, #16236, .F. ) ;
#2546 = CARTESIAN_POINT ( 'NONE',  ( 11.07256710390411669, 17.50279746095967326, -27.44776494551611279 ) ) ;
#2547 = ORIENTED_EDGE ( 'NONE', *, *, #14351, .T. ) ;
#2549 = DIRECTION ( 'NONE',  ( 1.000000000000000000, 0.000000000000000000, 0.000000000000000000 ) ) ;
#2548 = CARTESIAN_POINT ( 'NONE',  ( -14.24127349493501526, 24.60312559476172467, -12.53936607505307776 ) ) ;
#2550 = CARTESIAN_POINT ( 'NONE',  ( -9.705925585825449176, -18.43389087049540009, -26.82911780702928084 ) ) ;
#2551 = CARTESIAN_POINT ( 'NONE',  ( -19.26948696230207858, 27.85601271560029701, 11.00000000000000000 ) ) ;
#2552 = AXIS2_PLACEMENT_3D ( 'NONE', #23619, #25500, #20173 ) ;
#2553 = VECTOR ( 'NONE', #8873, 1000.000000000000000 ) ;
#2554 = CARTESIAN_POINT ( 'NONE',  ( -17.94496189389409579, -10.10876580532987390, -28.44359840047881249 ) ) ;
#2555 = CARTESIAN_POINT ( 'NONE',  ( -8.614355843301860105, -20.92117845966354750, -20.81903466987984075 ) ) ;
#2556 = DIRECTION ( 'NONE',  ( 0.000000000000000000, 0.000000000000000000, 1.000000000000000000 ) ) ;
#2557 = CARTESIAN_POINT ( 'NONE',  ( 14.15128070507878633, 21.55177582895931465, -15.54190844270684302 ) ) ;
#2558 = ADVANCED_FACE ( 'NONE', ( #3324 ), #24800, .T. ) ;
#2559 = ORIENTED_EDGE ( 'NONE', *, *, #25538, .F. ) ;
#2560 = CARTESIAN_POINT ( 'NONE',  ( 25.01923217006082112, 6.448405193624610732, -8.373492425512845116 ) ) ;
#2561 = CARTESIAN_POINT ( 'NONE',  ( -8.118377661053489902, 10.47536095541709322, 7.000000000000000000 ) ) ;
#2562 = CARTESIAN_POINT ( 'NONE',  ( -10.39021566973305788, 20.90519018800560858, 10.50000000000000000 ) ) ;
#2563 = EDGE_CURVE ( 'NONE', #21143, #2130, #3126, .T. ) ;
#2564 = CARTESIAN_POINT ( 'NONE',  ( -14.96930490892015797, 21.54088032874991399, 7.500000000000004441 ) ) ;
#2565 = VECTOR ( 'NONE', #34351, 1000.000000000000114 ) ;
#2566 = ORIENTED_EDGE ( 'NONE', *, *, #29697, .T. ) ;
#2567 = CARTESIAN_POINT ( 'NONE',  ( -30.68056625920112523, -0.7425512605776362074, -9.191107723028629550 ) ) ;
#2568 = CARTESIAN_POINT ( 'NONE',  ( 30.85535809781197258, -0.09603343769173000588, -6.415643733099492430 ) ) ;
#2569 = DIRECTION ( 'NONE',  ( 0.000000000000000000, 0.000000000000000000, 1.000000000000000000 ) ) ;
#2570 = CARTESIAN_POINT ( 'NONE',  ( 27.67544922579167022, -7.282050787522788227, 20.50957957746029336 ) ) ;
#2571 = CARTESIAN_POINT ( 'NONE',  ( 37.62663912510992503, -8.659558992827964374, -5.000000000000018652 ) ) ;
#2572 = CARTESIAN_POINT ( 'NONE',  ( 8.927394655428276593, 11.06314620770945290, 7.000000000000000000 ) ) ;
#2573 = ADVANCED_FACE ( 'NONE', ( #8829 ), #5968, .F. ) ;
#2574 = ORIENTED_EDGE ( 'NONE', *, *, #26846, .F. ) ;
#2575 = EDGE_CURVE ( 'NONE', #13129, #10650, #30374, .T. ) ;
#2576 = CARTESIAN_POINT ( 'NONE',  ( 32.33143948541791701, 1.358872982501826865, -5.000000000000000000 ) ) ;
#2577 = CIRCLE ( 'NONE', #20095, 1.000000000000000000 ) ;
#2578 = CARTESIAN_POINT ( 'NONE',  ( -2.629601561899595374, 7.723830143584053509, 11.00000000000000000 ) ) ;
#2579 = CARTESIAN_POINT ( 'NONE',  ( 32.33143948541783885, 1.358872982501748927, -5.000000000000000000 ) ) ;
#2580 = CARTESIAN_POINT ( 'NONE',  ( 1.427212664744208492, 34.45065703016087610, -11.97499105156896881 ) ) ;
#2581 = CARTESIAN_POINT ( 'NONE',  ( -5.139519228945863993, 36.36965741570538313, 10.49999999999999467 ) ) ;
#2582 = CARTESIAN_POINT ( 'NONE',  ( 12.55429062395116446, 25.98950339719798563, 18.87996532025784546 ) ) ;
#2583 = CARTESIAN_POINT ( 'NONE',  ( -12.03641663870442713, 15.85735326529964873, 6.000000000000000000 ) ) ;
#2584 = AXIS2_PLACEMENT_3D ( 'NONE', #13351, #31841, #28794 ) ;
#2585 = DIRECTION ( 'NONE',  ( 1.000000000000000000, 0.000000000000000000, 0.000000000000000000 ) ) ;
#2586 = CARTESIAN_POINT ( 'NONE',  ( 6.101049646137017390, 36.20318186463901355, 7.000000000000000000 ) ) ;
#2587 = FILL_AREA_STYLE ('',( #24707 ) ) ;
#2588 = CARTESIAN_POINT ( 'NONE',  ( 11.74081726099163347, 22.30219342717537856, -18.27100175958907968 ) ) ;
#2589 = DIRECTION ( 'NONE',  ( 1.000000000000000000, 0.000000000000000000, 0.000000000000000000 ) ) ;
#2590 = VERTEX_POINT ( 'NONE', #1081 ) ;
#2592 = LINE ( 'NONE', #20687, #16816 ) ;
#2591 = CARTESIAN_POINT ( 'NONE',  ( -17.65798338100345788, 13.64237717712649811, -19.02918139907341910 ) ) ;
#2593 = LINE ( 'NONE', #21272, #32192 ) ;
#2594 = CARTESIAN_POINT ( 'NONE',  ( 10.54418320030637268, -19.57350299331167065, -22.73395184212085596 ) ) ;
#2595 = CARTESIAN_POINT ( 'NONE',  ( 15.29107182738988158, 26.52751320015942937, -7.357832120508801310 ) ) ;
#2596 = CARTESIAN_POINT ( 'NONE',  ( 11.04637056303654319, 17.52039979612685272, -27.44572375426643163 ) ) ;
#2597 = ORIENTED_EDGE ( 'NONE', *, *, #13699, .F. ) ;
#2598 = CARTESIAN_POINT ( 'NONE',  ( -4.096822963000303019, 8.035697679810709815, 11.00000000000000000 ) ) ;
#2599 = EDGE_CURVE ( 'NONE', #11176, #9944, #13133, .T. ) ;
#2600 = CARTESIAN_POINT ( 'NONE',  ( 35.27612715351751405, 1.213969564528367906, 10.99999999999999822 ) ) ;
#2601 = CARTESIAN_POINT ( 'NONE',  ( -20.13935109294277481, -15.75254866237664153, -19.68832395494088772 ) ) ;
#2602 = CARTESIAN_POINT ( 'NONE',  ( -0.2690799054783746258, -20.63332487587387121, -27.17690005459235181 ) ) ;
#2603 = CARTESIAN_POINT ( 'NONE',  ( 11.21662988401310024, 17.21094317106729576, -28.71561903827853257 ) ) ;
#2604 = CARTESIAN_POINT ( 'NONE',  ( 17.91334720694058902, 10.03521261366046069, -28.86326398646745872 ) ) ;
#2605 = DIRECTION ( 'NONE',  ( -0.000000000000000000, -0.000000000000000000, 1.000000000000000000 ) ) ;
#2606 = CARTESIAN_POINT ( 'NONE',  ( -3.472550923952060220, 20.28740512945706342, -28.47266432443047890 ) ) ;
#2607 = ORIENTED_EDGE ( 'NONE', *, *, #11866, .F. ) ;
#2608 = CARTESIAN_POINT ( 'NONE',  ( -34.11471017283468399, -5.440626125914022282, -7.222970549378350036 ) ) ;
#2609 = CARTESIAN_POINT ( 'NONE',  ( -20.66414367076651715, 17.76245163069309640, 11.55979286843749421 ) ) ;
#2610 = VERTEX_POINT ( 'NONE', #3520 ) ;
#2611 = CARTESIAN_POINT ( 'NONE',  ( 16.00000000000000000, 22.50000000000000355, 11.00000000000000178 ) ) ;
#2612 = DIRECTION ( 'NONE',  ( 0.4156269377774681195, 0.5720614028176796984, -0.7071067811865426878 ) ) ;
#2613 = CARTESIAN_POINT ( 'NONE',  ( -29.40512185744006146, 0.2655052950593886907, -10.18551000707841503 ) ) ;
#2614 = CARTESIAN_POINT ( 'NONE',  ( 35.28872890698186637, -12.99774170744852064, -6.288584514710181317 ) ) ;
#2615 = ORIENTED_EDGE ( 'NONE', *, *, #12904, .T. ) ;
#2616 = EDGE_CURVE ( 'NONE', #27843, #32176, #35849, .T. ) ;
#2617 = CARTESIAN_POINT ( 'NONE',  ( 3.835130509701798918, 15.55077355964573904, 13.00000000000000178 ) ) ;
#2618 = ORIENTED_EDGE ( 'NONE', *, *, #10524, .T. ) ;
#2619 = EDGE_CURVE ( 'NONE', #4159, #31948, #35256, .T. ) ;
#2620 = CARTESIAN_POINT ( 'NONE',  ( -11.94134295108998245, 16.18301270189233065, 10.50000000000000000 ) ) ;
#2621 = PLANE ( 'NONE',  #29940 ) ;
#2622 = AXIS2_PLACEMENT_3D ( 'NONE', #36150, #26599, #21108 ) ;
#2623 = CARTESIAN_POINT ( 'NONE',  ( -3.229437847141423124, 24.50739181907689712, 6.000000000000000000 ) ) ;
#2624 = ORIENTED_EDGE ( 'NONE', *, *, #4066, .F. ) ;
#2625 = DIRECTION ( 'NONE',  ( 1.000000000000000000, 0.000000000000000000, 0.000000000000000000 ) ) ;
#2626 = CYLINDRICAL_SURFACE ( 'NONE', #7890, 0.5000000000000004441 ) ;
#2627 = DIRECTION ( 'NONE',  ( -0.6691306063588569053, 0.7431448254773954654, -0.000000000000000000 ) ) ;
#2628 = CARTESIAN_POINT ( 'NONE',  ( 16.77110579274708968, -12.86178676763160134, -26.29076339887767233 ) ) ;
#2629 = CARTESIAN_POINT ( 'NONE',  ( 19.05516563486750670, 15.43659885783165819, -10.86377891658857031 ) ) ;
#2630 = CARTESIAN_POINT ( 'NONE',  ( 8.895693167633664800, 22.91615671184446867, -20.04609200397479540 ) ) ;
#2631 = ORIENTED_EDGE ( 'NONE', *, *, #37932, .F. ) ;
#2632 = CARTESIAN_POINT ( 'NONE',  ( -22.31145927236271120, 10.79378405826409981, -6.938958974488863340 ) ) ;
#2633 = FACE_OUTER_BOUND ( 'NONE', #5660, .T. ) ;
#2634 = DIRECTION ( 'NONE',  ( 0.000000000000000000, 0.000000000000000000, 1.000000000000000000 ) ) ;
#2635 = CARTESIAN_POINT ( 'NONE',  ( 14.87691899169173659, -25.68218598931080976, -10.17324441562808701 ) ) ;
#2636 = CARTESIAN_POINT ( 'NONE',  ( 0.9999966292907466192, 22.50000000000031264, 12.00000000000000000 ) ) ;
#2637 = CIRCLE ( 'NONE', #14959, 1.000000000000000888 ) ;
#2638 = DIRECTION ( 'NONE',  ( 1.000000000000000000, 0.000000000000000000, 0.000000000000000000 ) ) ;
#2639 = EDGE_CURVE ( 'NONE', #8101, #11482, #365, .T. ) ;
#2640 = CARTESIAN_POINT ( 'NONE',  ( -14.83071926596090329, 25.63857572950853125, -10.17844402408916160 ) ) ;
#2641 = CARTESIAN_POINT ( 'NONE',  ( -23.37310973299193151, -26.11789763318362745, -8.074212004804937948 ) ) ;
#2642 = CARTESIAN_POINT ( 'NONE',  ( 9.006842323280976004, -18.63255999496335136, -27.49008004293749963 ) ) ;
#2643 = EDGE_CURVE ( 'NONE', #22086, #35666, #13052, .T. ) ;
#2644 = CARTESIAN_POINT ( 'NONE',  ( -8.118377661053488126, 10.47536095541708967, 11.00000000000000000 ) ) ;
#2645 = ORIENTED_EDGE ( 'NONE', *, *, #20055, .F. ) ;
#2646 = ORIENTED_EDGE ( 'NONE', *, *, #22480, .F. ) ;
#2647 = CARTESIAN_POINT ( 'NONE',  ( -7.714721346952166492, 25.82618255026152454, -17.82262248225727674 ) ) ;
#2648 = CARTESIAN_POINT ( 'NONE',  ( -4.476907992048016816, 18.63850621467409496, 13.00000000000000178 ) ) ;
#2649 = LINE ( 'NONE', #27428, #36051 ) ;
#2650 = AXIS2_PLACEMENT_3D ( 'NONE', #7659, #38135, #7855 ) ;
#2651 = LINE ( 'NONE', #9145, #3989 ) ;
#2652 = VERTEX_POINT ( 'NONE', #23005 ) ;
#2653 = CARTESIAN_POINT ( 'NONE',  ( 29.98824418678894332, 0.03310433232545182541, -9.238498873535908373 ) ) ;
#2654 = AXIS2_PLACEMENT_3D ( 'NONE', #22846, #3960, #13913 ) ;
#2655 = DIRECTION ( 'NONE',  ( 0.000000000000000000, 0.000000000000000000, 1.000000000000000000 ) ) ;
#2656 = CYLINDRICAL_SURFACE ( 'NONE', #9592, 58.00000000000007105 ) ;
#2657 = ORIENTED_EDGE ( 'NONE', *, *, #38722, .T. ) ;
#2658 = CARTESIAN_POINT ( 'NONE',  ( -30.45863603936437869, 0.01568503498656502113, -7.827967170345961456 ) ) ;
#2659 = CARTESIAN_POINT ( 'NONE',  ( 7.468455364333220103, 29.89744377950669474, 10.50000000000000000 ) ) ;
#2660 = ORIENTED_EDGE ( 'NONE', *, *, #35085, .F. ) ;
#2661 = CARTESIAN_POINT ( 'NONE',  ( 29.18684330182384912, -3.473580796607973920, -14.14225801422634632 ) ) ;
#2662 = CARTESIAN_POINT ( 'NONE',  ( 26.37421498764336292, -27.66411951031065541, 12.73282698324852902 ) ) ;
#2663 = ORIENTED_EDGE ( 'NONE', *, *, #28494, .F. ) ;
#2664 = CARTESIAN_POINT ( 'NONE',  ( 16.30840571581194354, 28.99314201041919503, 13.92931973827851699 ) ) ;
#2665 = VECTOR ( 'NONE', #1579, 1000.000000000000114 ) ;
#2666 = CARTESIAN_POINT ( 'NONE',  ( -11.32166530368854929, -20.22988973188854800, 19.99202127657163430 ) ) ;
#2667 = EDGE_CURVE ( 'NONE', #12151, #36438, #3713, .T. ) ;
#2668 = CYLINDRICAL_SURFACE ( 'NONE', #35774, 0.4999999999999995559 ) ;
#2669 = EDGE_CURVE ( 'NONE', #5543, #37261, #7269, .T. ) ;
#2670 = CARTESIAN_POINT ( 'NONE',  ( -5.569982264783402748, 31.74975025675326989, 19.99202127657043704 ) ) ;
#2671 = DIRECTION ( 'NONE',  ( 0.000000000000000000, 0.000000000000000000, 1.000000000000000000 ) ) ;
#2672 = EDGE_LOOP ( 'NONE', ( #35264, #9022, #13060, #29979 ) ) ;
#2673 = CARTESIAN_POINT ( 'NONE',  ( 2.587660364795204782, 9.681887955242936883, 6.000000000000000000 ) ) ;
#2674 = PLANE ( 'NONE',  #26654 ) ;
#2675 = CARTESIAN_POINT ( 'NONE',  ( 7.188809461230587061, 31.68087858109696597, -12.96927761962711223 ) ) ;
#2676 = AXIS2_PLACEMENT_3D ( 'NONE', #12215, #24607, #37199 ) ;
#2677 = LINE ( 'NONE', #19062, #36605 ) ;
#2678 = CARTESIAN_POINT ( 'NONE',  ( 15.65370567419071079, 2.019989953579482744, 20.99999999999999645 ) ) ;
#2679 = CARTESIAN_POINT ( 'NONE',  ( 11.51504914472953267, -18.67855797424754627, -23.68894626656194546 ) ) ;
#2680 = CARTESIAN_POINT ( 'NONE',  ( 7.910872327081121647, 10.00199400870852529, 10.49999999999999467 ) ) ;
#2681 = DIRECTION ( 'NONE',  ( 0.000000000000000000, 0.000000000000000000, 1.000000000000000000 ) ) ;
#2682 = DIRECTION ( 'NONE',  ( 1.000000000000000000, 0.000000000000000000, 0.000000000000000000 ) ) ;
#2683 = ORIENTED_EDGE ( 'NONE', *, *, #21322, .F. ) ;
#2684 = EDGE_CURVE ( 'NONE', #24176, #17915, #31549, .T. ) ;
#2685 = ORIENTED_EDGE ( 'NONE', *, *, #19102, .F. ) ;
#2686 = CARTESIAN_POINT ( 'NONE',  ( -15.34645457225791887, 26.58874063551486699, -6.887964196757459412 ) ) ;
#2687 = CARTESIAN_POINT ( 'NONE',  ( -23.42865034949355874, -24.48547250943464348, 18.42518152272145215 ) ) ;
#2688 = CARTESIAN_POINT ( 'NONE',  ( 13.65468850750463936, -24.11061919912373597, -13.51576474134096273 ) ) ;
#2689 = EDGE_CURVE ( 'NONE', #4212, #21531, #12862, .T. ) ;
#2690 = DIRECTION ( 'NONE',  ( 1.000000000000000000, 0.000000000000000000, 0.000000000000000000 ) ) ;
#2691 = ORIENTED_EDGE ( 'NONE', *, *, #5546, .F. ) ;
#2692 = VERTEX_POINT ( 'NONE', #25255 ) ;
#2694 = DIRECTION ( 'NONE',  ( 1.000000000000000000, 0.000000000000000000, 0.000000000000000000 ) ) ;
#2693 = CARTESIAN_POINT ( 'NONE',  ( -14.33337269284760751, 29.34602042987353343, -6.833538065190099431 ) ) ;
#2695 = CARTESIAN_POINT ( 'NONE',  ( -16.69208956396090926, -23.66209404026361796, -14.20132963311727714 ) ) ;
#2696 = CARTESIAN_POINT ( 'NONE',  ( 14.86556419889027048, 20.43481210330100240, 10.49999999999999822 ) ) ;
#2697 = VERTEX_POINT ( 'NONE', #38450 ) ;
#2698 = EDGE_CURVE ( 'NONE', #35769, #32713, #19557, .T. ) ;
#2699 = CARTESIAN_POINT ( 'NONE',  ( -28.05765197305022696, -9.635955780168286466, -15.75866516396918726 ) ) ;
#2700 = CARTESIAN_POINT ( 'NONE',  ( -14.97948837623191132, -26.23672582955694921, -8.299150191911987662 ) ) ;
#2701 = CARTESIAN_POINT ( 'NONE',  ( 14.01212783660239580, 27.85398076522207944, 7.455686640544908705 ) ) ;
#2702 = ORIENTED_EDGE ( 'NONE', *, *, #39692, .F. ) ;
#2703 = CARTESIAN_POINT ( 'NONE',  ( 28.88634399658755214, 1.998445312983448741, -6.421604194170203783 ) ) ;
#2704 = CARTESIAN_POINT ( 'NONE',  ( 9.062230821157433169, 11.16111041642485802, 10.83333333333333037 ) ) ;
#2705 = CARTESIAN_POINT ( 'NONE',  ( 7.014595103779618590, 35.79644522156321784, 10.49999999999999822 ) ) ;
#2706 = ORIENTED_EDGE ( 'NONE', *, *, #17533, .T. ) ;
#2707 = CARTESIAN_POINT ( 'NONE',  ( -28.39807035044848860, 0.06794131916572514196, -12.54307312449454415 ) ) ;
#2708 = ORIENTED_EDGE ( 'NONE', *, *, #34640, .F. ) ;
#2709 = CARTESIAN_POINT ( 'NONE',  ( 30.80942456744107005, -0.9143650800732036066, -9.182418516798353636 ) ) ;
#2710 = VECTOR ( 'NONE', #23153, 1000.000000000000000 ) ;
#2711 = CARTESIAN_POINT ( 'NONE',  ( 33.10646761238916014, -9.521241417579867417, 18.42518152272108622 ) ) ;
#2712 = CIRCLE ( 'NONE', #25401, 19.99999999999993605 ) ;
#2713 = ORIENTED_EDGE ( 'NONE', *, *, #6496, .T. ) ;
#2714 = CARTESIAN_POINT ( 'NONE',  ( -21.78239903333861349, 3.553677865574983663, -21.93178419694463344 ) ) ;
#2715 = EDGE_CURVE ( 'NONE', #33392, #16160, #29997, .T. ) ;
#2716 = DIRECTION ( 'NONE',  ( 1.000000000000000000, 0.000000000000000000, 0.000000000000000000 ) ) ;
#2717 = EDGE_CURVE ( 'NONE', #18344, #2814, #20286, .T. ) ;
#2718 = CARTESIAN_POINT ( 'NONE',  ( 5.524694096546953759, 36.45979188825327100, 10.49999999999999822 ) ) ;
#2719 = CARTESIAN_POINT ( 'NONE',  ( -18.03924190088572388, -16.85603499720483001, 20.99999999999999645 ) ) ;
#2720 = AXIS2_PLACEMENT_3D ( 'NONE', #9943, #37578, #31280 ) ;
#2721 = CARTESIAN_POINT ( 'NONE',  ( 10.44103466624280507, 32.57396620494213124, 9.500000000000000000 ) ) ;
#2722 = FACE_BOUND ( 'NONE', #10922, .T. ) ;
#2723 = DIRECTION ( 'NONE',  ( -0.7622652262560031255, -0.2926062055178105248, 0.5773502691896430505 ) ) ;
#2724 = ORIENTED_EDGE ( 'NONE', *, *, #8963, .T. ) ;
#2725 = CARTESIAN_POINT ( 'NONE',  ( -19.95945058307471953, 5.721769224514986263, -26.53156390793591868 ) ) ;
#2726 = CARTESIAN_POINT ( 'NONE',  ( 36.48557158514975640, -11.24999999999995559, 10.00000000000000000 ) ) ;
#2727 = DIRECTION ( 'NONE',  ( -0.000000000000000000, -0.000000000000000000, -1.000000000000000000 ) ) ;
#2728 = CARTESIAN_POINT ( 'NONE',  ( 14.69851482477425719, -14.40017170160419901, -28.50529416406689620 ) ) ;
#2729 = CARTESIAN_POINT ( 'NONE',  ( 8.293999462566144842, 11.53598992149257008, 13.00000000000000178 ) ) ;
#2730 = CARTESIAN_POINT ( 'NONE',  ( 12.22522338894938088, 20.70977026341328653, -19.46168301453599625 ) ) ;
#2731 = CARTESIAN_POINT ( 'NONE',  ( 10.09822582592846096, -27.41751403068768056, 11.55979286844081244 ) ) ;
#2732 = ORIENTED_EDGE ( 'NONE', *, *, #37444, .F. ) ;
#2733 = CARTESIAN_POINT ( 'NONE',  ( -16.03826714829968125, 24.67705000163143580, -5.474135182149290735 ) ) ;
#2734 = CARTESIAN_POINT ( 'NONE',  ( -20.67756819927166134, -17.78966421867582781, 20.94377226548369109 ) ) ;
#2735 = ADVANCED_FACE ( 'NONE', ( #31753 ), #22843, .T. ) ;
#2736 = DIRECTION ( 'NONE',  ( -1.000000000000000000, 0.000000000000000000, 0.000000000000000000 ) ) ;
#2737 = CARTESIAN_POINT ( 'NONE',  ( 14.75231007449413312, 25.35299502146948925, -10.65417580594813174 ) ) ;
#2738 = EDGE_LOOP ( 'NONE', ( #36414, #4286, #37880, #26014 ) ) ;
#2739 = FACE_OUTER_BOUND ( 'NONE', #19124, .T. ) ;
#2740 = ORIENTED_EDGE ( 'NONE', *, *, #36853, .F. ) ;
#2742 = DIRECTION ( 'NONE',  ( 0.000000000000000000, 0.000000000000000000, 1.000000000000000000 ) ) ;
#2741 = CARTESIAN_POINT ( 'NONE',  ( -10.90492496769149433, 17.35893878472046126, -29.34663910038763746 ) ) ;
#2743 = CARTESIAN_POINT ( 'NONE',  ( -15.22980700598171211, -26.18112790717167826, -8.761347792469088347 ) ) ;
#2744 = DIRECTION ( 'NONE',  ( 1.000000000000000000, -0.000000000000000000, 0.000000000000000000 ) ) ;
#2745 = CARTESIAN_POINT ( 'NONE',  ( -21.52496464139200683, -12.12314022445560724, -20.68871519823034077 ) ) ;
#2746 = CARTESIAN_POINT ( 'NONE',  ( -11.78551508893061417, -23.03824580411184186, -15.52955309715219023 ) ) ;
#2747 = FACE_OUTER_BOUND ( 'NONE', #17861, .T. ) ;
#2748 = CARTESIAN_POINT ( 'NONE',  ( 12.28898657554147711, 17.72469657176861091, -23.97054147917551603 ) ) ;
#2749 = VERTEX_POINT ( 'NONE', #22600 ) ;
#2750 = CARTESIAN_POINT ( 'NONE',  ( 19.15330224686634963, 7.305649259636135540, -30.00000000000000000 ) ) ;
#2751 = DIRECTION ( 'NONE',  ( -0.000000000000000000, -0.000000000000000000, -1.000000000000000000 ) ) ;
#2752 = CIRCLE ( 'NONE', #18953, 1.000000000000000888 ) ;
#2753 = DIRECTION ( 'NONE',  ( 1.000000000000000000, 0.000000000000000000, 0.000000000000000000 ) ) ;
#2754 = CARTESIAN_POINT ( 'NONE',  ( -8.843266739736662885, 16.81698729810787540, 11.00000000000000000 ) ) ;
#2755 = VERTEX_POINT ( 'NONE', #28698 ) ;
#2756 = CARTESIAN_POINT ( 'NONE',  ( -25.04116001157528970, -0.6213440581654174899, -18.31437346914016828 ) ) ;
#2757 = CARTESIAN_POINT ( 'NONE',  ( 23.36948692125722005, 0.4087503446080729130, -20.52222899045708715 ) ) ;
#2758 = AXIS2_PLACEMENT_3D ( 'NONE', #19676, #24085, #17608 ) ;
#2759 = CARTESIAN_POINT ( 'NONE',  ( 13.95683075005237050, 28.08631143191933432, 11.00000000000000000 ) ) ;
#2760 = CARTESIAN_POINT ( 'NONE',  ( 21.85869495253959371, -19.21667513322869780, 20.69868183039798737 ) ) ;
#2761 = CARTESIAN_POINT ( 'NONE',  ( 19.48557158514982746, -11.25000000000009415, 3.000000000000000000 ) ) ;
#2762 = DIRECTION ( 'NONE',  ( 0.000000000000000000, 0.000000000000000000, 1.000000000000000000 ) ) ;
#2763 = CIRCLE ( 'NONE', #2110, 0.4999999999999997780 ) ;
#2764 = ORIENTED_EDGE ( 'NONE', *, *, #14758, .F. ) ;
#2765 = ADVANCED_FACE ( 'NONE', ( #22801 ), #28903, .F. ) ;
#2766 = LINE ( 'NONE', #36500, #39833 ) ;
#2767 = CONICAL_SURFACE ( 'NONE', #20957, 0.5000000000000023315, 0.7853981633974499443 ) ;
#2768 = DIRECTION ( 'NONE',  ( -0.6916548014802258448, -0.1470157664651941254, -0.7071067811865482389 ) ) ;
#2769 = DIRECTION ( 'NONE',  ( 0.000000000000000000, 0.000000000000000000, 1.000000000000000000 ) ) ;
#2770 = CARTESIAN_POINT ( 'NONE',  ( 3.295098241983883014, 32.08381273648824106, -13.82339927732507512 ) ) ;
#2771 = DIRECTION ( 'NONE',  ( -0.4156269377774565732, -0.5720614028176828070, -0.7071067811865469066 ) ) ;
#2772 = CARTESIAN_POINT ( 'NONE',  ( 2.317734025672769427, 9.191051544684729180, 9.500000000000000000 ) ) ;
#2773 = AXIS2_PLACEMENT_3D ( 'NONE', #11010, #4706, #29487 ) ;
#2774 = CARTESIAN_POINT ( 'NONE',  ( -0.5000000000000000000, 37.00000000000000711, 9.500000000000000000 ) ) ;
#2775 = CARTESIAN_POINT ( 'NONE',  ( -14.31603901957233482, 19.98981538725089990, 9.500000000000000000 ) ) ;
#2776 = FACE_OUTER_BOUND ( 'NONE', #32903, .T. ) ;
#2777 = DIRECTION ( 'NONE',  ( -0.9135454576426059736, -0.4067366430757888285, 0.000000000000000000 ) ) ;
#2778 = CARTESIAN_POINT ( 'NONE',  ( 11.53528522782755417, 20.60494803806667008, -20.42540399034420773 ) ) ;
#2779 = DIRECTION ( 'NONE',  ( 0.1045284632676422437, -0.9945218953682746221, 0.000000000000000000 ) ) ;
#2780 = ORIENTED_EDGE ( 'NONE', *, *, #34355, .F. ) ;
#2781 = AXIS2_PLACEMENT_3D ( 'NONE', #8402, #36035, #17357 ) ;
#2783 = CARTESIAN_POINT ( 'NONE',  ( 7.766013557953383106, 28.81973365084986938, 10.50000000000000178 ) ) ;
#2782 = CARTESIAN_POINT ( 'NONE',  ( -19.34266190408123975, 15.30325114017860066, -9.874887699621096360 ) ) ;
#2784 = DIRECTION ( 'NONE',  ( 0.6724985119639518283, 0.2185080122244121292, -0.7071067811865521247 ) ) ;
#2785 = CARTESIAN_POINT ( 'NONE',  ( 13.38383379236761961, -23.62348432274365351, -14.47560677120037731 ) ) ;
#2786 = CARTESIAN_POINT ( 'NONE',  ( -22.16237596998683657, -26.26640487554014314, -8.538874403386357059 ) ) ;
#2787 = CARTESIAN_POINT ( 'NONE',  ( -12.77091082532341382, 29.60251629318183575, 12.00000000000000000 ) ) ;
#2788 = B_SPLINE_CURVE_WITH_KNOTS ( 'NONE', 3,
 ( #36402, #24802, #21360, #17923, #21157, #33565 ),
 .UNSPECIFIED., .F., .F.,
 ( 4, 2, 4 ),
 ( 0.000000000000000000, 0.5000000000000000000, 1.000000000000000000 ),
 .UNSPECIFIED. ) ;
#2789 = CARTESIAN_POINT ( 'NONE',  ( 14.27584049633174246, 24.51164464966358025, -12.54715642964581157 ) ) ;
#2790 = ORIENTED_EDGE ( 'NONE', *, *, #22755, .T. ) ;
#2791 = DIRECTION ( 'NONE',  ( 0.000000000000000000, 0.000000000000000000, 1.000000000000000000 ) ) ;
#2792 = CARTESIAN_POINT ( 'NONE',  ( -6.440836655099179353, 34.39106106163288246, 6.000000000000000000 ) ) ;
#2793 = CARTESIAN_POINT ( 'NONE',  ( -30.82617745331405246, -24.12092658898454189, 14.53008259254011492 ) ) ;
#2794 = CARTESIAN_POINT ( 'NONE',  ( -28.22238894054767044, -23.52913000678562838, -8.433307499048945388 ) ) ;
#2795 = CARTESIAN_POINT ( 'NONE',  ( -0.3713521775821578275, -24.14560739446480042, -10.88444230627014520 ) ) ;
#2796 = CARTESIAN_POINT ( 'NONE',  ( 11.26908400546618871, 17.12495040990986794, -30.00000000000000355 ) ) ;
#2797 = CARTESIAN_POINT ( 'NONE',  ( 19.58307402619674775, 12.02054371642003083, -15.94811493075723163 ) ) ;
#2798 = EDGE_CURVE ( 'NONE', #8550, #34673, #11022, .T. ) ;
#2799 = CARTESIAN_POINT ( 'NONE',  ( -3.563111756202009595, 20.80833165756875758, -26.31733160343138067 ) ) ;
#2800 = ORIENTED_EDGE ( 'NONE', *, *, #14509, .F. ) ;
#2801 = CARTESIAN_POINT ( 'NONE',  ( -33.94661022151303342, -5.405014578827573857, -7.666919038779478335 ) ) ;
#2802 = AXIS2_PLACEMENT_3D ( 'NONE', #24162, #27016, #11381 ) ;
#2803 = CARTESIAN_POINT ( 'NONE',  ( -20.60789226802554808, 17.73598670051888604, 12.14047268032921956 ) ) ;
#2804 = ORIENTED_EDGE ( 'NONE', *, *, #31693, .F. ) ;
#2805 = CARTESIAN_POINT ( 'NONE',  ( 2.368912364081567024, 7.688072489931943032, 7.455539900862791391 ) ) ;
#2806 = CIRCLE ( 'NONE', #15759, 1.000000000000000888 ) ;
#2807 = CARTESIAN_POINT ( 'NONE',  ( 7.611215932167711529, 18.68301270189218855, 7.000000000000000000 ) ) ;
#2808 = CARTESIAN_POINT ( 'NONE',  ( -29.94900022519512461, 0.8516863067260661557, -6.418642555037194164 ) ) ;
#2809 = CARTESIAN_POINT ( 'NONE',  ( 19.23659220497393108, -7.112289578705962789, -30.00000000000000000 ) ) ;
#2810 = CONICAL_SURFACE ( 'NONE', #28755, 1.000000000000016431, 0.7853981633974533860 ) ;
#2811 = ADVANCED_FACE ( 'NONE', ( #8382 ), #2287, .F. ) ;
#2812 = ORIENTED_EDGE ( 'NONE', *, *, #3348, .T. ) ;
#2813 = CARTESIAN_POINT ( 'NONE',  ( 8.100578861132808228, 28.44816123811117592, 10.50000000000000178 ) ) ;
#2814 = VERTEX_POINT ( 'NONE', #23216 ) ;
#2815 = CARTESIAN_POINT ( 'NONE',  ( 11.14716901145161643, 12.46304090461738667, 12.00000000000000000 ) ) ;
#2816 = FACE_OUTER_BOUND ( 'NONE', #1853, .T. ) ;
#2817 = ADVANCED_FACE ( 'NONE', ( #19968 ), #20378, .T. ) ;
#2818 = AXIS2_PLACEMENT_3D ( 'NONE', #2729, #5776, #24659 ) ;
#2819 = CARTESIAN_POINT ( 'NONE',  ( -13.94482798346716557, 26.50521816028930289, 11.00000000000000000 ) ) ;
#2820 = ORIENTED_EDGE ( 'NONE', *, *, #6864, .F. ) ;
#2821 = EDGE_CURVE ( 'NONE', #25235, #1258, #39735, .T. ) ;
#2822 = CARTESIAN_POINT ( 'NONE',  ( -1.644293514239202558, 20.68013128552042446, -27.71419510687025323 ) ) ;
#2823 = DIRECTION ( 'NONE',  ( 0.000000000000000000, 0.000000000000000000, 1.000000000000000000 ) ) ;
#2824 = DIRECTION ( 'NONE',  ( -1.000000000000000000, 0.000000000000000000, 0.000000000000000000 ) ) ;
#2825 = EDGE_CURVE ( 'NONE', #751, #30937, #10533, .T. ) ;
#2826 = DIRECTION ( 'NONE',  ( 0.000000000000000000, 0.000000000000000000, -1.000000000000000000 ) ) ;
#2827 = CARTESIAN_POINT ( 'NONE',  ( 29.14969154284566955, -23.82267159204295837, -6.287676784333006808 ) ) ;
#2828 = CARTESIAN_POINT ( 'NONE',  ( 16.77886244865171150, 13.09686862389438211, -23.29364800532082569 ) ) ;
#2829 =( GEOMETRIC_REPRESENTATION_CONTEXT ( 3 ) GLOBAL_UNCERTAINTY_ASSIGNED_CONTEXT ( ( #10802 ) ) GLOBAL_UNIT_ASSIGNED_CONTEXT ( ( #25494, #37301, #31402 ) ) REPRESENTATION_CONTEXT ( 'NONE', 'WORKASPACE' ) );
#2830 = CARTESIAN_POINT ( 'NONE',  ( 10.66234920991248103, 30.15450380941021535, -12.15963120324809843 ) ) ;
#2831 = ORIENTED_EDGE ( 'NONE', *, *, #14626, .F. ) ;
#2832 = CARTESIAN_POINT ( 'NONE',  ( -21.77806019913552404, 11.75179560353630848, -6.453505103389286290 ) ) ;
#2833 = FACE_OUTER_BOUND ( 'NONE', #21196, .T. ) ;
#2834 = AXIS2_PLACEMENT_3D ( 'NONE', #19697, #37986, #25986 ) ;
#2835 = CARTESIAN_POINT ( 'NONE',  ( 12.38193221270099365, -22.02126375945465142, -17.42657776036095996 ) ) ;
#2836 = DIRECTION ( 'NONE',  ( 0.000000000000000000, 0.000000000000000000, 1.000000000000000000 ) ) ;
#2837 = CARTESIAN_POINT ( 'NONE',  ( 19.79815887584821610, 19.84782313723624370, -13.42901749168597192 ) ) ;
#2838 = CARTESIAN_POINT ( 'NONE',  ( -15.40119896161133006, 26.83624744099596171, -5.473949411210034199 ) ) ;
#2839 = AXIS2_PLACEMENT_3D ( 'NONE', #10969, #20310, #38790 ) ;
#2840 = CARTESIAN_POINT ( 'NONE',  ( -14.34583555374895525, -17.16037222123812356, -23.35150257132816876 ) ) ;
#2841 = CARTESIAN_POINT ( 'NONE',  ( 10.66118309792825336, -25.49418724601090247, -7.379814460239313867 ) ) ;
#2842 = EDGE_CURVE ( 'NONE', #10050, #34846, #18968, .T. ) ;
#2843 = CYLINDRICAL_SURFACE ( 'NONE', #34158, 0.5000000000000000000 ) ;
#2844 = EDGE_CURVE ( 'NONE', #29799, #20155, #23814, .T. ) ;
#2845 = ORIENTED_EDGE ( 'NONE', *, *, #210, .T. ) ;
#2846 = ORIENTED_EDGE ( 'NONE', *, *, #35816, .T. ) ;
#2847 = CARTESIAN_POINT ( 'NONE',  ( -10.22043165594364034, 34.42610915102720526, -7.180433678547599285 ) ) ;
#2848 = CARTESIAN_POINT ( 'NONE',  ( 0.5000000000000002220, 37.50000000000000711, 10.49999999999999822 ) ) ;
#2849 = DIRECTION ( 'NONE',  ( 0.000000000000000000, 0.000000000000000000, 1.000000000000000000 ) ) ;
#2850 = VECTOR ( 'NONE', #7811, 999.9999999999998863 ) ;
#2851 = LINE ( 'NONE', #15239, #17000 ) ;
#2852 = EDGE_LOOP ( 'NONE', ( #28372, #25079, #12755, #29327 ) ) ;
#2853 = CARTESIAN_POINT ( 'NONE',  ( 22.21841090602945457, 0.6747637996796579385, -22.73641212969366876 ) ) ;
#2854 = CARTESIAN_POINT ( 'NONE',  ( -14.09933648065464062, 26.02968990214173317, 10.50000000000000533 ) ) ;
#2855 = LINE ( 'NONE', #12791, #34246 ) ;
#2856 = B_SPLINE_SURFACE_WITH_KNOTS ( 'NONE', 1, 3, ( 
 ( #24221, #18331, #12031, #33387, #39459, #8582, #20979, #18531, #30922, #37014 ),
 ( #2887, #33580, #21766, #17941, #3085, #30726, #15479, #12230, #30324, #15279 ) ),
 .UNSPECIFIED., .F., .F., .F.,
 ( 2, 2 ),
 ( 4, 2, 2, 2, 4 ),
 ( 0.000000000000000000, 1.000000000000000000 ),
 ( -1.421612811542164678, -1.028913729843439651, -0.6362146481447145119, -0.2435155664459894009, 0.1491835152527357100 ),
 .UNSPECIFIED. ) ;
#2857 = VERTEX_POINT ( 'NONE', #14676 ) ;
#2858 = CARTESIAN_POINT ( 'NONE',  ( -26.47678993223912869, 0.3192213469539110227, -15.45381411608538968 ) ) ;
#2859 = CARTESIAN_POINT ( 'NONE',  ( -8.626760388790547296, 16.94198729810787185, 10.74999999999999822 ) ) ;
#2860 = ORIENTED_EDGE ( 'NONE', *, *, #21555, .T. ) ;
#2861 = CARTESIAN_POINT ( 'NONE',  ( 24.34856821748838129, -4.279746131925105779, -19.99731643529021241 ) ) ;
#2862 = CONICAL_SURFACE ( 'NONE', #16488, 0.4999999999999997780, 0.7853981633974524978 ) ;
#2863 = ORIENTED_EDGE ( 'NONE', *, *, #8963, .F. ) ;
#2864 = CARTESIAN_POINT ( 'NONE',  ( 1.940950748631622647, 40.43805239114133343, 12.14047268033097815 ) ) ;
#2865 = CARTESIAN_POINT ( 'NONE',  ( 6.008588623656380356, -15.38567963534269900, 20.94377226548378701 ) ) ;
#2866 = DIRECTION ( 'NONE',  ( -0.000000000000000000, -0.000000000000000000, -1.000000000000000000 ) ) ;
#2867 = EDGE_CURVE ( 'NONE', #21617, #5911, #11632, .T. ) ;
#2868 = CARTESIAN_POINT ( 'NONE',  ( -8.231369907346209658, 29.48764348321983420, 19.99202127657101258 ) ) ;
#2869 = CIRCLE ( 'NONE', #22986, 1.000000000000004441 ) ;
#2870 = DIRECTION ( 'NONE',  ( 0.000000000000000000, 0.000000000000000000, 1.000000000000000000 ) ) ;
#2871 = ORIENTED_EDGE ( 'NONE', *, *, #2319, .F. ) ;
#2872 = CARTESIAN_POINT ( 'NONE',  ( 3.987511920225066397, 8.280017797930394607, 10.49999999999999822 ) ) ;
#2873 = DIRECTION ( 'NONE',  ( 0.000000000000000000, 0.000000000000000000, 1.000000000000000000 ) ) ;
#2874 = CARTESIAN_POINT ( 'NONE',  ( 2.629601561899395534, 7.723830143584016206, 11.00000000000000000 ) ) ;
#2875 = DIRECTION ( 'NONE',  ( -0.000000000000000000, 0.000000000000000000, -1.000000000000000000 ) ) ;
#2876 = CARTESIAN_POINT ( 'NONE',  ( 8.060800481109751559, 35.74480146002363767, -7.585522589778642910 ) ) ;
#2877 = CARTESIAN_POINT ( 'NONE',  ( 5.400683141673458643, 15.91724817395916070, 9.000000000000001776 ) ) ;
#2878 = CARTESIAN_POINT ( 'NONE',  ( 14.68260282716209630, -21.83111036330549481, -17.17910696205039756 ) ) ;
#2879 = CARTESIAN_POINT ( 'NONE',  ( 7.790810073469618402, 10.07556825234751408, 10.49999999999999822 ) ) ;
#2880 = DIRECTION ( 'NONE',  ( -1.000000000000000000, 0.000000000000000000, 0.000000000000000000 ) ) ;
#2881 = CARTESIAN_POINT ( 'NONE',  ( 13.87104230352200140, 20.53934056656866147, 10.00000000000000000 ) ) ;
#2882 = CIRCLE ( 'NONE', #21701, 0.5000000000000004441 ) ;
#2883 = ORIENTED_EDGE ( 'NONE', *, *, #22924, .T. ) ;
#2884 = CARTESIAN_POINT ( 'NONE',  ( -11.91667304890831680, 19.35618664243762765, -21.62132196524237671 ) ) ;
#2885 = CARTESIAN_POINT ( 'NONE',  ( -28.60197298176802860, -19.58586899272916781, 19.27171037444157520 ) ) ;
#2886 = CARTESIAN_POINT ( 'NONE',  ( 14.88441567456970915, -26.21443660824652255, -8.299845255435092994 ) ) ;
#2887 = CARTESIAN_POINT ( 'NONE',  ( -3.607749162633399731, 7.931741834401828228, 10.49999999999999645 ) ) ;
#2888 = ORIENTED_EDGE ( 'NONE', *, *, #29011, .F. ) ;
#2889 = ORIENTED_EDGE ( 'NONE', *, *, #34484, .F. ) ;
#2890 = CARTESIAN_POINT ( 'NONE',  ( -10.79837678754097574, 21.37684657782732245, -20.29484020400954236 ) ) ;
#2891 = CARTESIAN_POINT ( 'NONE',  ( -12.22911246598414614, -17.74238687663815739, -24.74578340650955610 ) ) ;
#2892 = CARTESIAN_POINT ( 'NONE',  ( 11.31392148919590923, 36.91540483778863546, -5.000000000000002665 ) ) ;
#2893 = EDGE_CURVE ( 'NONE', #22834, #5201, #5972, .T. ) ;
#2894 = AXIS2_PLACEMENT_3D ( 'NONE', #28848, #38196, #3864 ) ;
#2895 = ORIENTED_EDGE ( 'NONE', *, *, #10144, .F. ) ;
#2896 = CARTESIAN_POINT ( 'NONE',  ( -34.27855427131117949, -9.549784089487717509, -8.912513341492028118 ) ) ;
#2897 = CARTESIAN_POINT ( 'NONE',  ( -13.74267396692251531, -24.56729334661521946, -12.56146162201199878 ) ) ;
#2898 = CARTESIAN_POINT ( 'NONE',  ( 2.317734025672765430, 9.191051544684729180, 10.50000000000000000 ) ) ;
#2899 = ORIENTED_EDGE ( 'NONE', *, *, #16069, .F. ) ;
#2900 = CARTESIAN_POINT ( 'NONE',  ( 30.42361321058833212, 0.1827335297003471470, -7.358803297337979998 ) ) ;
#2901 = PLANE ( 'NONE',  #23894 ) ;
#2902 = CARTESIAN_POINT ( 'NONE',  ( -10.52087624881762196, 22.14834255721595824, 10.74999999999998934 ) ) ;
#2903 = EDGE_LOOP ( 'NONE', ( #37586, #21867, #5252, #24338, #553 ) ) ;
#2904 = CARTESIAN_POINT ( 'NONE',  ( -29.67980999164576872, -0.04279675855848630306, -10.17325362659203414 ) ) ;
#2905 = EDGE_LOOP ( 'NONE', ( #38137, #14487, #10573, #9669 ) ) ;
#2906 = CARTESIAN_POINT ( 'NONE',  ( 21.43241828677356864, -0.7131419970486393423, -24.85227051139408516 ) ) ;
#2907 = CARTESIAN_POINT ( 'NONE',  ( 24.28032989564875876, -12.76774640304083164, 21.00000000000001066 ) ) ;
#2908 = CARTESIAN_POINT ( 'NONE',  ( 25.04152548477498996, -24.48861404543278653, 17.92354375535251521 ) ) ;
#2909 = VERTEX_POINT ( 'NONE', #26259 ) ;
#2910 = CARTESIAN_POINT ( 'NONE',  ( -25.82288576596329932, 3.514228647792512206, -12.69986980209609762 ) ) ;
#2911 = DIRECTION ( 'NONE',  ( 0.6123724356957948034, 0.3535533905932776721, -0.7071067811865452413 ) ) ;
#2912 = EDGE_CURVE ( 'NONE', #32554, #20514, #8595, .T. ) ;
#2913 = VECTOR ( 'NONE', #34711, 1000.000000000000114 ) ;
#2914 = CARTESIAN_POINT ( 'NONE',  ( -5.724378136954611840, 12.76962061027129458, 12.00000000000000000 ) ) ;
#2915 = FACE_OUTER_BOUND ( 'NONE', #9754, .T. ) ;
#2916 = EDGE_CURVE ( 'NONE', #1914, #22045, #26091, .T. ) ;
#2917 = DIRECTION ( 'NONE',  ( 0.5000000000000039968, 0.8660254037844363761, -0.000000000000000000 ) ) ;
#2918 = AXIS2_PLACEMENT_3D ( 'NONE', #40147, #30817, #12322 ) ;
#2919 =( BOUNDED_SURFACE ( )  B_SPLINE_SURFACE ( 2, 3, ( 
 ( #5150, #20799, #20193, #8194, #20601, #32999, #29930, #2111, #5348, #38674, #29330, #8596, #10847, #20993, #30136, #14695, #2309, #27086 ),
 ( #23239, #39475, #35632, #11654, #1706, #33401, #5542, #1500, #7790, #32589, #4748, #17155, #14086, #21385, #30542, #18152, #15288, #33792 ),
 ( #17953, #12639, #12042, #28073, #6138, #30338, #27676, #34380, #3097, #18343, #27479, #40063, #8802, #15492, #24630, #33594, #31130, #36825 ) ),
 .UNSPECIFIED., .F., .F., .F. ) 
 B_SPLINE_SURFACE_WITH_KNOTS ( ( 3, 3 ),
 ( 4, 2, 2, 2, 2, 2, 2, 2, 4 ),
 ( 0.000000000000000000, 1.000000000000000000 ),
 ( 4.459899766721548531, 4.784821457936484279, 5.109743149151420027, 5.434664840366355776, 5.759586531581291524, 6.084508222796227273, 6.409429914011163021, 6.734351605226098769, 7.059273296441033629 ),
 .UNSPECIFIED. ) 
 GEOMETRIC_REPRESENTATION_ITEM ( )  RATIONAL_B_SPLINE_SURFACE ( (
 ( 1.000000000000000000, 1.000000000000000000, 1.000000000000000000, 1.000000000000000000, 1.000000000000000000, 1.000000000000000000, 1.000000000000000000, 1.000000000000000000, 1.000000000000000000, 1.000000000000000000, 1.000000000000000000, 1.000000000000000000, 1.000000000000000000, 1.000000000000000000, 1.000000000000000000, 1.000000000000000000, 1.000000000000000000, 1.000000000000000000),
 ( 0.7071067811865474617, 0.7071067811865474617, 0.7071067811865474617, 0.7071067811865474617, 0.7071067811865475727, 0.7071067811865475727, 0.7071067811865475727, 0.7071067811865475727, 0.7071067811865474617, 0.7071067811865474617, 0.7071067811865474617, 0.7071067811865474617, 0.7071067811865474617, 0.7071067811865474617, 0.7071067811865474617, 0.7071067811865474617, 0.7071067811865475727, 0.7071067811865475727),
 ( 1.000000000000000000, 1.000000000000000000, 1.000000000000000000, 1.000000000000000000, 1.000000000000000000, 1.000000000000000000, 1.000000000000000000, 1.000000000000000000, 1.000000000000000000, 1.000000000000000000, 1.000000000000000000, 1.000000000000000000, 1.000000000000000000, 1.000000000000000000, 1.000000000000000000, 1.000000000000000000, 1.000000000000000000, 1.000000000000000000) ) ) 
 REPRESENTATION_ITEM ( '' )  SURFACE ( )  );
#2920 = ADVANCED_FACE ( 'NONE', ( #32569 ), #20172, .F. ) ;
#2921 = FACE_BOUND ( 'NONE', #19584, .T. ) ;
#2922 = CARTESIAN_POINT ( 'NONE',  ( 25.55085611915419364, 8.900480655592511781, 12.73282698324917384 ) ) ;
#2923 = ORIENTED_EDGE ( 'NONE', *, *, #30613, .F. ) ;
#2924 = CARTESIAN_POINT ( 'NONE',  ( -24.17774524110126322, 7.027723166510716268, -10.34013492986881744 ) ) ;
#2925 = DIRECTION ( 'NONE',  ( 0.000000000000000000, 0.000000000000000000, 1.000000000000000000 ) ) ;
#2926 = DIRECTION ( 'NONE',  ( 0.000000000000000000, 0.000000000000000000, 1.000000000000000000 ) ) ;
#2927 = CARTESIAN_POINT ( 'NONE',  ( 14.10981997949339117, -15.61727850128731987, -26.45440405776506765 ) ) ;
#2928 = CARTESIAN_POINT ( 'NONE',  ( 5.440908595777814050, 35.94977745735560859, 9.000000000000001776 ) ) ;
#2929 = CARTESIAN_POINT ( 'NONE',  ( 10.82808496700584477, 17.46135606781462712, -28.69954358548662299 ) ) ;
#2930 = ORIENTED_EDGE ( 'NONE', *, *, #20002, .F. ) ;
#2931 = CARTESIAN_POINT ( 'NONE',  ( -15.87097346945386889, 23.44423284912781469, -9.272708727512497973 ) ) ;
#2932 = CARTESIAN_POINT ( 'NONE',  ( -24.40183261524807889, -16.82966968839920341, 20.82122704794079837 ) ) ;
#2933 = DIRECTION ( 'NONE',  ( 0.000000000000000000, 0.000000000000000000, 1.000000000000000000 ) ) ;
#2934 = CARTESIAN_POINT ( 'NONE',  ( 12.66836227548348326, 21.03152034328669018, -18.45485530985660461 ) ) ;
#2935 = VERTEX_POINT ( 'NONE', #30115 ) ;
#2936 = DIRECTION ( 'NONE',  ( 0.8090169943749421222, -0.5877852522924804646, 0.000000000000000000 ) ) ;
#2937 = ADVANCED_FACE ( 'NONE', ( #23618 ), #34340, .T. ) ;
#2938 = EDGE_LOOP ( 'NONE', ( #31533, #39184, #15875, #24617 ) ) ;
#2940 = DIRECTION ( 'NONE',  ( 0.3090169943749448977, -0.9510565162951543083, 0.000000000000000000 ) ) ;
#2939 = CARTESIAN_POINT ( 'NONE',  ( -12.82069841282840095, 21.83108406841477844, -17.41332505554854393 ) ) ;
#2941 = ADVANCED_FACE ( 'NONE', ( #37208 ), #13777, .T. ) ;
#2942 = CARTESIAN_POINT ( 'NONE',  ( -12.76993028032038602, -22.56078344509325007, -16.43107071015407783 ) ) ;
#2943 = CARTESIAN_POINT ( 'NONE',  ( -14.98890121934612019, -28.67928442654180898, 11.00000000000000000 ) ) ;
#2944 = EDGE_CURVE ( 'NONE', #39810, #17859, #36497, .T. ) ;
#2945 = VECTOR ( 'NONE', #32735, 1000.000000000000000 ) ;
#2946 = CARTESIAN_POINT ( 'NONE',  ( -26.35083455085015558, -14.83645574100917131, -15.67644099750071440 ) ) ;
#2947 = CARTESIAN_POINT ( 'NONE',  ( -13.59131951343294276, -25.82231284968012019, -8.782825323748010504 ) ) ;
#2948 = DIRECTION ( 'NONE',  ( 1.000000000000000000, 1.224646799147353947E-16, 0.000000000000000000 ) ) ;
#2949 = CARTESIAN_POINT ( 'NONE',  ( 15.68066481369410248, 23.61642061338914189, -9.744478434708410575 ) ) ;
#2950 = VERTEX_POINT ( 'NONE', #24014 ) ;
#2951 = CARTESIAN_POINT ( 'NONE',  ( 25.90794112815367356, 5.571130670237141480, -6.915715379737312318 ) ) ;
#2952 = CARTESIAN_POINT ( 'NONE',  ( 9.356056665764066693, 26.06569820189703179, 10.50000000000000000 ) ) ;
#2953 = CARTESIAN_POINT ( 'NONE',  ( 6.914817619329722831, 35.81128241919675759, 7.381627713044574435 ) ) ;
#2954 = DIRECTION ( 'NONE',  ( -0.2079116908177663092, -0.9781476007338041345, 0.000000000000000000 ) ) ;
#2955 = CIRCLE ( 'NONE', #4250, 0.5000000000000002220 ) ;
#2956 = ORIENTED_EDGE ( 'NONE', *, *, #14335, .T. ) ;
#2957 = CARTESIAN_POINT ( 'NONE',  ( -20.64517791135504510, -0.4843551386664524672, -28.01037723252847655 ) ) ;
#2958 = CARTESIAN_POINT ( 'NONE',  ( 31.05798941631825727, -0.2002603227334578129, -4.999999999999999112 ) ) ;
#2959 = AXIS2_PLACEMENT_3D ( 'NONE', #10460, #1731, #32201 ) ;
#2960 = AXIS2_PLACEMENT_3D ( 'NONE', #9346, #21726, #34132 ) ;
#2961 = CARTESIAN_POINT ( 'NONE',  ( -7.096882951594430722, 29.56287847632736288, 10.49999999999999822 ) ) ;
#2962 = CARTESIAN_POINT ( 'NONE',  ( 24.76266088601874671, -18.72941319223726353, 20.50957957746007310 ) ) ;
#2963 = ORIENTED_EDGE ( 'NONE', *, *, #33839, .T. ) ;
#2964 = CARTESIAN_POINT ( 'NONE',  ( 21.88444403592371756, 6.126538576424477966, -30.00000000000001066 ) ) ;
#2965 = EDGE_CURVE ( 'NONE', #21746, #3779, #21550, .T. ) ;
#2966 = DIRECTION ( 'NONE',  ( -0.9135454576426005335, 0.4067366430758009299, -0.000000000000000000 ) ) ;
#2967 = ADVANCED_FACE ( 'NONE', ( #39846 ), #32, .T. ) ;
#2968 = VERTEX_POINT ( 'NONE', #5923 ) ;
#2969 = DIRECTION ( 'NONE',  ( -0.000000000000000000, -0.000000000000000000, -1.000000000000000000 ) ) ;
#2970 = CARTESIAN_POINT ( 'NONE',  ( 3.399837471815457590, 8.909889435135580626, 7.000000000000000000 ) ) ;
#2971 = CARTESIAN_POINT ( 'NONE',  ( 13.05736835487433289, 16.11602540378438420, 10.50000000000000178 ) ) ;
#2972 = CARTESIAN_POINT ( 'NONE',  ( 1.462604112257996247, 20.70414128060931702, -27.71111028557563927 ) ) ;
#2973 = DIRECTION ( 'NONE',  ( 0.6691306063588671194, 0.7431448254773861395, 0.000000000000000000 ) ) ;
#2974 = CARTESIAN_POINT ( 'NONE',  ( 14.66655470856244037, 20.08105443166835258, 10.49999999999999822 ) ) ;
#2975 = DIRECTION ( 'NONE',  ( 0.000000000000000000, 0.000000000000000000, 1.000000000000000000 ) ) ;
#2976 = AXIS2_PLACEMENT_3D ( 'NONE', #883, #25654, #10221 ) ;
#2977 = LINE ( 'NONE', #12318, #18656 ) ;
#2978 = FACE_OUTER_BOUND ( 'NONE', #5641, .T. ) ;
#2979 = CARTESIAN_POINT ( 'NONE',  ( 6.143904198944455608, -13.77689918168226235, 23.00000000000000000 ) ) ;
#2980 = CARTESIAN_POINT ( 'NONE',  ( 12.39613117785802920, 22.48878480139081759, -17.32547671766618791 ) ) ;
#2982 = CONICAL_SURFACE ( 'NONE', #23746, 1.000000000000007772, 0.7853981633974560506 ) ;
#2981 = DIRECTION ( 'NONE',  ( 0.000000000000000000, 0.000000000000000000, -1.000000000000000000 ) ) ;
#2983 = ORIENTED_EDGE ( 'NONE', *, *, #7165, .F. ) ;
#2986 = VECTOR ( 'NONE', #18239, 1000.000000000000000 ) ;
#2985 = LINE ( 'NONE', #25112, #36943 ) ;
#2984 = CARTESIAN_POINT ( 'NONE',  ( -17.84890069020828562, 18.10929763232169165, -10.32883059554979788 ) ) ;
#2987 = LINE ( 'NONE', #21665, #4283 ) ;
#2988 = VECTOR ( 'NONE', #5876, 1000.000000000000000 ) ;
#2989 = CARTESIAN_POINT ( 'NONE',  ( 12.65230758151554014, -22.55754344927865063, -16.44404600518156201 ) ) ;
#2990 = CARTESIAN_POINT ( 'NONE',  ( -20.38544652068658181, -25.64170277295648859, -10.37427513536433743 ) ) ;
#2991 = CARTESIAN_POINT ( 'NONE',  ( 27.14644468510626396, -3.730463242941437940, 19.99202127657103745 ) ) ;
#2992 = CARTESIAN_POINT ( 'NONE',  ( 11.88256809692872729, 19.39247382671743480, -21.61519272832449445 ) ) ;
#2993 = VERTEX_POINT ( 'NONE', #2487 ) ;
#2994 = DIRECTION ( 'NONE',  ( -0.000000000000000000, -0.000000000000000000, -1.000000000000000000 ) ) ;
#2995 = CARTESIAN_POINT ( 'NONE',  ( -13.64179698895352288, -24.10910305434091327, -13.51635134767616364 ) ) ;
#2996 = CARTESIAN_POINT ( 'NONE',  ( -36.96658581397586119, -12.84323481469905204, 13.92931973827791836 ) ) ;
#2997 = CARTESIAN_POINT ( 'NONE',  ( -25.23528266485080707, -19.79492694554141607, -13.84032828069353194 ) ) ;
#2998 = CARTESIAN_POINT ( 'NONE',  ( -0.2665898626985158115, -20.55074757747597758, -28.29937881637059505 ) ) ;
#2999 = CARTESIAN_POINT ( 'NONE',  ( 15.19726048192972634, 25.40763732123437890, -9.245452804566358651 ) ) ;
#3000 = CARTESIAN_POINT ( 'NONE',  ( 21.60539011535767528, 12.02606291333052368, -6.454038670498706054 ) ) ;
#3001 = CARTESIAN_POINT ( 'NONE',  ( -18.00000000000000000, 22.50000000000000355, 13.00000000000000178 ) ) ;
#3002 = CARTESIAN_POINT ( 'NONE',  ( -4.822863700933563536, 33.73409833160523874, -12.00050471651474204 ) ) ;
#3003 = ORIENTED_EDGE ( 'NONE', *, *, #7870, .T. ) ;
#3004 = CARTESIAN_POINT ( 'NONE',  ( -33.42954140234754590, -6.257036898190599494, -9.426039654913852317 ) ) ;
#3005 = FACE_OUTER_BOUND ( 'NONE', #22440, .T. ) ;
#3006 = ORIENTED_EDGE ( 'NONE', *, *, #32881, .T. ) ;
#3007 = PLANE ( 'NONE',  #27811 ) ;
#3008 = CARTESIAN_POINT ( 'NONE',  ( 20.91702953749078020, -16.07165331220364735, 23.00000000000000355 ) ) ;
#3009 = AXIS2_PLACEMENT_3D ( 'NONE', #40006, #27824, #11788 ) ;
#3010 = CARTESIAN_POINT ( 'NONE',  ( -23.70214251413468531, 1.055375858189379956, -19.56052323388921721 ) ) ;
#3011 = CARTESIAN_POINT ( 'NONE',  ( 28.97475848703913925, -10.63545647045585874, -14.78716727546217946 ) ) ;
#3012 = AXIS2_PLACEMENT_3D ( 'NONE', #23878, #35677, #39314 ) ;
#3013 = AXIS2_PLACEMENT_3D ( 'NONE', #19573, #3337, #15932 ) ;
#3014 = ORIENTED_EDGE ( 'NONE', *, *, #2091, .F. ) ;
#3015 = DIRECTION ( 'NONE',  ( -0.000000000000000000, -0.000000000000000000, -1.000000000000000000 ) ) ;
#3016 = ORIENTED_EDGE ( 'NONE', *, *, #22058, .T. ) ;
#3017 = LINE ( 'NONE', #14810, #33336 ) ;
#3018 = DIRECTION ( 'NONE',  ( 1.000000000000000000, 0.000000000000000000, 0.000000000000000000 ) ) ;
#3019 = DIRECTION ( 'NONE',  ( -0.7431448254773862505, 0.6691306063588672304, -0.000000000000000000 ) ) ;
#3020 = ORIENTED_EDGE ( 'NONE', *, *, #11811, .T. ) ;
#3021 = CARTESIAN_POINT ( 'NONE',  ( -1.624100677291493877, 20.43571491435562493, -30.00000000000000000 ) ) ;
#3022 = CARTESIAN_POINT ( 'NONE',  ( -5.440908595777639079, 35.94977745735568675, 11.00000000000000000 ) ) ;
#3023 = CARTESIAN_POINT ( 'NONE',  ( -9.331903152615899089, 11.35703883385581037, 9.500000000000000000 ) ) ;
#3024 = FACE_OUTER_BOUND ( 'NONE', #8809, .T. ) ;
#3025 = CARTESIAN_POINT ( 'NONE',  ( 20.30746460111456742, -15.60079166006380724, -19.67824267733233157 ) ) ;
#3026 = CARTESIAN_POINT ( 'NONE',  ( 19.69380245318583178, 14.63332033592687687, -9.880714762412520002 ) ) ;
#3027 = CARTESIAN_POINT ( 'NONE',  ( 13.15697686552113588, 29.30913038656967018, -9.982777366939737718 ) ) ;
#3028 = EDGE_LOOP ( 'NONE', ( #38755, #36747, #4844, #7937 ) ) ;
#3029 = CARTESIAN_POINT ( 'NONE',  ( -17.64762046312857180, 10.49585427871703658, -28.86324443608691226 ) ) ;
#3030 = CARTESIAN_POINT ( 'NONE',  ( 3.456468065140020141, 26.15323006594238464, 23.00000000000000000 ) ) ;
#3031 = CARTESIAN_POINT ( 'NONE',  ( 15.62075852780784047, -26.70067611967377985, -6.413895762741850248 ) ) ;
#3032 = DIRECTION ( 'NONE',  ( 0.1045284632676422437, -0.9945218953682746221, 0.000000000000000000 ) ) ;
#3033 = CARTESIAN_POINT ( 'NONE',  ( 20.55563217186196212, -29.52600041847795254, -5.000000000000015987 ) ) ;
#3034 = CARTESIAN_POINT ( 'NONE',  ( 19.48557158514975285, -11.24999999999995737, 10.00000000000000000 ) ) ;
#3035 = AXIS2_PLACEMENT_3D ( 'NONE', #2562, #14545, #36686 ) ;
#3036 = CARTESIAN_POINT ( 'NONE',  ( -15.22219195120841739, 26.44100515191062328, -7.826622911995333887 ) ) ;
#3037 = VECTOR ( 'NONE', #17147, 1000.000000000000000 ) ;
#3038 = CARTESIAN_POINT ( 'NONE',  ( -22.43675667947073293, -25.13256344364474160, -10.31126045143009051 ) ) ;
#3039 = CARTESIAN_POINT ( 'NONE',  ( 10.20831112218712278, -21.62331746727261361, -18.60984041202089401 ) ) ;
#3040 = EDGE_CURVE ( 'NONE', #33978, #6629, #20971, .T. ) ;
#3041 = CARTESIAN_POINT ( 'NONE',  ( 11.47910261372047636, 31.49019768869741753, 10.49999999999999822 ) ) ;
#3042 = ORIENTED_EDGE ( 'NONE', *, *, #18589, .T. ) ;
#3043 = CARTESIAN_POINT ( 'NONE',  ( -9.862325270099388419, 33.04988333219784380, -9.830511281312073635 ) ) ;
#3044 = DIRECTION ( 'NONE',  ( 1.000000000000000000, 0.000000000000000000, 0.000000000000000000 ) ) ;
#3045 = DIRECTION ( 'NONE',  ( -0.6691306063588570163, 0.7431448254773952433, 0.000000000000000000 ) ) ;
#3046 = CARTESIAN_POINT ( 'NONE',  ( -9.296885549838707519, 10.71356306745948217, 10.49999999999999822 ) ) ;
#3047 = ORIENTED_EDGE ( 'NONE', *, *, #16636, .T. ) ;
#3048 = CARTESIAN_POINT ( 'NONE',  ( 24.55482339067931719, 0.4410777889133716823, -18.45331033963499223 ) ) ;
#3049 = ADVANCED_FACE ( 'NONE', ( #18322 ), #18365, .T. ) ;
#3050 = DIRECTION ( 'NONE',  ( -0.000000000000000000, -0.000000000000000000, -1.000000000000000000 ) ) ;
#3051 = DIRECTION ( 'NONE',  ( 0.000000000000000000, 0.000000000000000000, -1.000000000000000000 ) ) ;
#3052 = EDGE_CURVE ( 'NONE', #17743, #37305, #11845, .T. ) ;
#3053 = ORIENTED_EDGE ( 'NONE', *, *, #36357, .F. ) ;
#3054 = CARTESIAN_POINT ( 'NONE',  ( -27.12366736632709774, 0.2592640696602764305, -14.47817184671785817 ) ) ;
#3055 = CARTESIAN_POINT ( 'NONE',  ( 8.927394655428274817, 11.06314620770945290, 7.500000000000000888 ) ) ;
#3056 = ORIENTED_EDGE ( 'NONE', *, *, #6591, .T. ) ;
#3057 = CARTESIAN_POINT ( 'NONE',  ( 20.52978982471044489, -3.550452485816113946, -27.17543462584250236 ) ) ;
#3058 = ORIENTED_EDGE ( 'NONE', *, *, #20232, .F. ) ;
#3059 = CARTESIAN_POINT ( 'NONE',  ( -14.61820604905143384, 32.41591307681827061, 13.32518128616608699 ) ) ;
#3060 = CARTESIAN_POINT ( 'NONE',  ( 11.59681349796545824, -18.61320969074927945, 20.50957957745985993 ) ) ;
#3061 = DIRECTION ( 'NONE',  ( -0.4999999999999920064, 0.8660254037844432595, 0.000000000000000000 ) ) ;
#3062 = CARTESIAN_POINT ( 'NONE',  ( 11.11100267139549658, 25.58833710557466290, 19.66345542862528362 ) ) ;
#3063 = AXIS2_PLACEMENT_3D ( 'NONE', #17957, #34184, #40067 ) ;
#3064 = VECTOR ( 'NONE', #29426, 1000.000000000000000 ) ;
#3065 = CARTESIAN_POINT ( 'NONE',  ( 2.476901250629512941, 26.36149378532653031, 13.00000000000000178 ) ) ;
#3066 = ORIENTED_EDGE ( 'NONE', *, *, #593, .T. ) ;
#3067 = LINE ( 'NONE', #6306, #19643 ) ;
#3068 = CARTESIAN_POINT ( 'NONE',  ( -15.87271491999997863, 26.91186955879524945, 15.72805884748939498 ) ) ;
#3069 = EDGE_CURVE ( 'NONE', #3204, #802, #39650, .T. ) ;
#3070 = DIRECTION ( 'NONE',  ( 1.000000000000000000, 0.000000000000000000, 0.000000000000000000 ) ) ;
#3071 = EDGE_CURVE ( 'NONE', #25412, #38194, #24810, .T. ) ;
#3072 = VECTOR ( 'NONE', #12547, 1000.000000000000114 ) ;
#3073 = CARTESIAN_POINT ( 'NONE',  ( 13.63581098909226519, 27.45627467658428600, 7.000000000000000000 ) ) ;
#3074 = VECTOR ( 'NONE', #35458, 1000.000000000000114 ) ;
#3075 = CARTESIAN_POINT ( 'NONE',  ( 6.270378422840378718, 27.73110307447709744, -16.74549866864413517 ) ) ;
#3076 = DIRECTION ( 'NONE',  ( -0.000000000000000000, -0.000000000000000000, 1.000000000000000000 ) ) ;
#3077 = CARTESIAN_POINT ( 'NONE',  ( 11.37404163648363387, -17.38721229013356862, -27.31762905785370776 ) ) ;
#3078 = FACE_OUTER_BOUND ( 'NONE', #33550, .T. ) ;
#3079 = DIRECTION ( 'NONE',  ( 1.000000000000000000, 0.000000000000000000, 0.000000000000000000 ) ) ;
#3080 = CARTESIAN_POINT ( 'NONE',  ( 0.6108529249775871417, 37.48755679569043053, 7.500000000000000888 ) ) ;
#3081 = ORIENTED_EDGE ( 'NONE', *, *, #21958, .F. ) ;
#3082 = CARTESIAN_POINT ( 'NONE',  ( -14.04545270995350670, 23.89835750463747743, -13.51489203531869521 ) ) ;
#3083 = CARTESIAN_POINT ( 'NONE',  ( -27.81120771500161837, -23.04947625254830967, 17.92354375535251876 ) ) ;
#3084 = CARTESIAN_POINT ( 'NONE',  ( 10.06203327364132427, -19.22105317348337650, -23.87374111627889306 ) ) ;
#3085 = CARTESIAN_POINT ( 'NONE',  ( -3.574287532905768394, 8.089166425130688509, 10.87262190629277470 ) ) ;
#3086 = EDGE_LOOP ( 'NONE', ( #11914, #38778, #23491 ) ) ;
#3087 = ORIENTED_EDGE ( 'NONE', *, *, #18215, .T. ) ;
#3088 = CARTESIAN_POINT ( 'NONE',  ( -12.81438437627916294, 24.11148518490756842, -15.30534549235409614 ) ) ;
#3089 = CARTESIAN_POINT ( 'NONE',  ( -20.01115666102352009, -26.54103525232406824, -8.595240658381658960 ) ) ;
#3090 = EDGE_CURVE ( 'NONE', #6733, #17177, #24615, .T. ) ;
#3091 = FACE_BOUND ( 'NONE', #37232, .T. ) ;
#3092 = VECTOR ( 'NONE', #32291, 1000.000000000000000 ) ;
#3093 = VECTOR ( 'NONE', #2365, 1000.000000000000000 ) ;
#3094 = ORIENTED_EDGE ( 'NONE', *, *, #38872, .T. ) ;
#3095 = CARTESIAN_POINT ( 'NONE',  ( -34.28623899043527956, -10.66410740567661897, -8.897208059971323024 ) ) ;
#3096 = CARTESIAN_POINT ( 'NONE',  ( -15.07568792015453063, -26.56401150065150674, -6.417385571140632905 ) ) ;
#3097 = CARTESIAN_POINT ( 'NONE',  ( 35.72300736400885057, -23.12593624637960588, 11.00000000000000000 ) ) ;
#3098 = ORIENTED_EDGE ( 'NONE', *, *, #3139, .F. ) ;
#3099 = CARTESIAN_POINT ( 'NONE',  ( 22.16878676813625049, 0.8754114111470541193, -22.76043277781719709 ) ) ;
#3100 = DIRECTION ( 'NONE',  ( -0.000000000000000000, -0.000000000000000000, -1.000000000000000000 ) ) ;
#3101 = DIRECTION ( 'NONE',  ( -0.9945218953682740670, -0.1045284632676460046, 6.938893903907226800E-15 ) ) ;
#3102 = AXIS2_PLACEMENT_3D ( 'NONE', #15352, #6002, #15953 ) ;
#3103 = EDGE_LOOP ( 'NONE', ( #12291, #25656, #14279, #8995 ) ) ;
#3104 = CARTESIAN_POINT ( 'NONE',  ( -20.52801489595192308, 0.8352239444486609932, -28.70617517559551501 ) ) ;
#3105 = ORIENTED_EDGE ( 'NONE', *, *, #4020, .F. ) ;
#3106 = CARTESIAN_POINT ( 'NONE',  ( 32.44839610264516239, -1.855716912065746627, -5.000000000000000000 ) ) ;
#3107 = AXIS2_PLACEMENT_3D ( 'NONE', #35785, #1453, #25282 ) ;
#3108 = CARTESIAN_POINT ( 'NONE',  ( -10.99858019813223642, -17.35606952494162769, -30.00000000000001421 ) ) ;
#3109 = CARTESIAN_POINT ( 'NONE',  ( 31.91928157790820109, -18.42860581134451792, 17.92354375535250810 ) ) ;
#3110 = ORIENTED_EDGE ( 'NONE', *, *, #19798, .F. ) ;
#3111 = CARTESIAN_POINT ( 'NONE',  ( -23.58591353912177624, 4.323729375759905125, -16.75487901750983966 ) ) ;
#3112 = CARTESIAN_POINT ( 'NONE',  ( -14.49226701858006727, 26.37020042452770596, 7.438752290525425082 ) ) ;
#3113 = CARTESIAN_POINT ( 'NONE',  ( 19.48557158514982746, -11.25000000000009415, -5.000000000000000000 ) ) ;
#3114 = DIRECTION ( 'NONE',  ( -0.8660254037844431485, -0.4999999999999921729, 0.000000000000000000 ) ) ;
#3115 = DIRECTION ( 'NONE',  ( -0.9781476007338042455, 0.2079116908177664480, 0.000000000000000000 ) ) ;
#3116 = EDGE_CURVE ( 'NONE', #36749, #20981, #14877, .T. ) ;
#3117 = AXIS2_PLACEMENT_3D ( 'NONE', #23943, #17260, #7895 ) ;
#3118 = CIRCLE ( 'NONE', #1181, 0.5000000000000004441 ) ;
#3119 = FACE_BOUND ( 'NONE', #12939, .T. ) ;
#3120 = CARTESIAN_POINT ( 'NONE',  ( -4.908204406342476567, 36.67476118479555680, 7.102474990965863100 ) ) ;
#3121 = CARTESIAN_POINT ( 'NONE',  ( -19.69137326279327027, 5.702251777040514114, -29.41124866415784567 ) ) ;
#3122 = CARTESIAN_POINT ( 'NONE',  ( 10.10646936306337729, 32.94553861768082470, 10.49999999999999822 ) ) ;
#3123 = CARTESIAN_POINT ( 'NONE',  ( -0.8712085880691411433, 13.69667159339610762, 6.000000000000000000 ) ) ;
#3124 = CARTESIAN_POINT ( 'NONE',  ( 22.74023349794498827, -25.07456572998067656, -10.30111323015509761 ) ) ;
#3125 = CIRCLE ( 'NONE', #8325, 0.5000000000000004441 ) ;
#3126 = LINE ( 'NONE', #36660, #34547 ) ;
#3127 = CARTESIAN_POINT ( 'NONE',  ( 10.91336093707554333, 17.75825062284819467, -26.81050411434687675 ) ) ;
#3128 = VERTEX_POINT ( 'NONE', #36807 ) ;
#3129 = CARTESIAN_POINT ( 'NONE',  ( -15.43817069320426860, 22.63450057941196647, -11.66983478573951061 ) ) ;
#3130 = CARTESIAN_POINT ( 'NONE',  ( -27.09004689510899766, -14.60731774717074138, 20.69868183039799803 ) ) ;
#3131 = CARTESIAN_POINT ( 'NONE',  ( -7.577547685840081648, 11.84256962714647798, 6.000000000000000000 ) ) ;
#3132 = CARTESIAN_POINT ( 'NONE',  ( 15.42533216934834250, 26.65747446338114557, -5.946092576581627931 ) ) ;
#3133 = ORIENTED_EDGE ( 'NONE', *, *, #4115, .F. ) ;
#3134 = CARTESIAN_POINT ( 'NONE',  ( 1.853166178176219203, 23.42705098312512746, 12.00000000000000000 ) ) ;
#3135 = ORIENTED_EDGE ( 'NONE', *, *, #33825, .F. ) ;
#3137 = LINE ( 'NONE', #30584, #28955 ) ;
#3136 = CARTESIAN_POINT ( 'NONE',  ( -15.00041699303972287, 26.46481294341050372, -8.753260597601569160 ) ) ;
#3138 = CARTESIAN_POINT ( 'NONE',  ( -11.28598964761482470, -20.45078756188820535, -20.52814714296091836 ) ) ;
#3139 = EDGE_CURVE ( 'NONE', #19314, #19744, #37007, .T. ) ;
#3140 = DIRECTION ( 'NONE',  ( -0.8660254037844431485, -0.4999999999999921174, 0.000000000000000000 ) ) ;
#3141 = ORIENTED_EDGE ( 'NONE', *, *, #7856, .F. ) ;
#3142 = CARTESIAN_POINT ( 'NONE',  ( -33.84242992198449684, -16.42796269968979317, -7.975450335500420707 ) ) ;
#3143 = CARTESIAN_POINT ( 'NONE',  ( -9.612297877367879551, -19.83582942224187207, -22.84230155296175369 ) ) ;
#3144 = LINE ( 'NONE', #27924, #11195 ) ;
#3145 = CARTESIAN_POINT ( 'NONE',  ( 13.63576238296606036, 20.52424253562647039, -17.54980119926154813 ) ) ;
#3147 = EDGE_CURVE ( 'NONE', #28465, #13430, #9177, .T. ) ;
#3146 = EDGE_LOOP ( 'NONE', ( #766, #12726, #19900 ) ) ;
#3148 = CARTESIAN_POINT ( 'NONE',  ( 26.35199392063378099, 4.663862263929487995, -8.352515954957800304 ) ) ;
#3149 = CARTESIAN_POINT ( 'NONE',  ( -2.317734025672944842, 9.191051544684764707, 9.500000000000000000 ) ) ;
#3150 = ADVANCED_FACE ( 'NONE', ( #6119 ), #24828, .T. ) ;
#3151 = CARTESIAN_POINT ( 'NONE',  ( 10.81260707898150386, 32.90853150812155548, 10.49999999999999822 ) ) ;
#3152 = CARTESIAN_POINT ( 'NONE',  ( -5.082607396026893376, 23.58034083595207875, 12.00000000000000000 ) ) ;
#3153 = ORIENTED_EDGE ( 'NONE', *, *, #22580, .F. ) ;
#3154 = CARTESIAN_POINT ( 'NONE',  ( -30.06454056556724197, -0.2461126078811654294, -9.689261385093018930 ) ) ;
#3156 = CARTESIAN_POINT ( 'NONE',  ( 27.92911499328061709, -0.05970110741965063694, -13.48672115538755278 ) ) ;
#3155 = AXIS2_PLACEMENT_3D ( 'NONE', #35519, #19669, #14180 ) ;
#3157 = CIRCLE ( 'NONE', #1886, 0.9999999999999974465 ) ;
#3158 = EDGE_CURVE ( 'NONE', #10973, #10557, #6006, .T. ) ;
#3159 = CARTESIAN_POINT ( 'NONE',  ( -5.092030333742499693, 36.31140934042896617, 10.49999999999999822 ) ) ;
#3160 = CARTESIAN_POINT ( 'NONE',  ( 20.97602320185162839, -19.42790811720868049, 20.69868183039782750 ) ) ;
#3161 = ORIENTED_EDGE ( 'NONE', *, *, #35362, .F. ) ;
#3162 = VECTOR ( 'NONE', #14714, 1000.000000000000000 ) ;
#3163 = CARTESIAN_POINT ( 'NONE',  ( 13.47223693944937750, 18.09844039693851769, -21.24786896499729139 ) ) ;
#3164 = DIRECTION ( 'NONE',  ( 1.000000000000000000, 0.000000000000000000, 0.000000000000000000 ) ) ;
#3165 = ORIENTED_EDGE ( 'NONE', *, *, #15617, .T. ) ;
#3166 = EDGE_CURVE ( 'NONE', #34935, #18367, #30408, .T. ) ;
#3167 = DIRECTION ( 'NONE',  ( 1.000000000000000000, 0.000000000000000000, 0.000000000000000000 ) ) ;
#3168 = EDGE_CURVE ( 'NONE', #2652, #10797, #32654, .T. ) ;
#3169 = EDGE_CURVE ( 'NONE', #18534, #39411, #33263, .T. ) ;
#3170 = CARTESIAN_POINT ( 'NONE',  ( -27.36225479880417311, 10.16098284219050107, 11.00000000000000000 ) ) ;
#3171 = CARTESIAN_POINT ( 'NONE',  ( 12.80736835487432934, 15.68301270189215835, 11.00000000000000000 ) ) ;
#3172 = CARTESIAN_POINT ( 'NONE',  ( 3.789724143065339224, 37.00233177767923110, -8.414891994916880336 ) ) ;
#3173 = CARTESIAN_POINT ( 'NONE',  ( -1.853172919594719970, 21.57294901687549427, 6.000000000000000000 ) ) ;
#3174 = DIRECTION ( 'NONE',  ( -0.000000000000000000, -0.000000000000000000, 1.000000000000000000 ) ) ;
#3175 = CARTESIAN_POINT ( 'NONE',  ( -10.44103466624267362, 32.57396620494226624, 9.500000000000000000 ) ) ;
#3176 = DIRECTION ( 'NONE',  ( -0.4999999999999920064, 0.8660254037844432595, -0.000000000000000000 ) ) ;
#3177 = LINE ( 'NONE', #30617, #16414 ) ;
#3178 = CARTESIAN_POINT ( 'NONE',  ( -2.256323172317921788, 14.28970123917155277, 9.000000000000001776 ) ) ;
#3179 = CARTESIAN_POINT ( 'NONE',  ( 14.18938711277078291, 25.87820699252437961, -11.53243986395856702 ) ) ;
#3180 = LINE ( 'NONE', #31015, #19762 ) ;
#3181 = AXIS2_PLACEMENT_3D ( 'NONE', #2783, #24712, #37112 ) ;
#3182 = ORIENTED_EDGE ( 'NONE', *, *, #14027, .F. ) ;
#3184 = CARTESIAN_POINT ( 'NONE',  ( 12.30736835487432934, 14.81698729810772797, 11.00000000000000000 ) ) ;
#3183 = CARTESIAN_POINT ( 'NONE',  ( -15.00437050688289986, 14.15087644790256682, -27.67883097521226787 ) ) ;
#3185 = CARTESIAN_POINT ( 'NONE',  ( -7.294006203984644721, 33.46401007850805343, 6.000000000000000000 ) ) ;
#3186 = CARTESIAN_POINT ( 'NONE',  ( 12.66509161227769553, -22.55792390413381554, -16.44263127660910939 ) ) ;
#3187 = CARTESIAN_POINT ( 'NONE',  ( -13.08565055680642786, -16.70549789365643178, -25.90368761856597146 ) ) ;
#3188 = CARTESIAN_POINT ( 'NONE',  ( -6.953812613386785912, 14.77701242934787906, 13.00000000000000178 ) ) ;
#3189 = CARTESIAN_POINT ( 'NONE',  ( 11.02121864814410657, 17.43735474281069386, -28.07628969929118412 ) ) ;
#3190 = PRODUCT ( 'Dual-Edge Stainless Steel Rotary Blade', 'Dual-Edge Stainless Steel Rotary Blade', '', ( #10158 ) ) ;
#3191 = ORIENTED_EDGE ( 'NONE', *, *, #10347, .T. ) ;
#3192 = CARTESIAN_POINT ( 'NONE',  ( -3.503793317224517700, 8.420815634768727520, 7.000000000000000000 ) ) ;
#3193 = CARTESIAN_POINT ( 'NONE',  ( -9.901882729520171011, -18.83983749962000687, -25.02192390785083731 ) ) ;
#3194 = ADVANCED_FACE ( 'NONE', ( #18408 ), #33464, .T. ) ;
#3195 = CARTESIAN_POINT ( 'NONE',  ( -34.92340065173439712, -3.770459477548423699, 14.53008259254011136 ) ) ;
#3196 = ADVANCED_FACE ( 'NONE', ( #6001 ), #22998, .T. ) ;
#3197 = CARTESIAN_POINT ( 'NONE',  ( -30.78128484184130187, -22.64136542128004592, -5.000000000000004441 ) ) ;
#3198 = CARTESIAN_POINT ( 'NONE',  ( -0.3522767274228070788, -23.48013668842627766, -13.90457325883725659 ) ) ;
#3199 = CARTESIAN_POINT ( 'NONE',  ( 15.53783880108225190, 26.09496515834549868, -6.417711193549261672 ) ) ;
#3200 = EDGE_CURVE ( 'NONE', #40105, #37972, #26479, .T. ) ;
#3201 = CARTESIAN_POINT ( 'NONE',  ( 22.35343170176878402, 10.00543086905888934, -9.882773338075907077 ) ) ;
#3202 = CARTESIAN_POINT ( 'NONE',  ( 9.892954722048896699, 20.95745441963929423, 10.50000000000000533 ) ) ;
#3203 = CARTESIAN_POINT ( 'NONE',  ( -2.860784471046919020, 20.39385230774454882, -28.46275780569326130 ) ) ;
#3204 = VERTEX_POINT ( 'NONE', #33998 ) ;
#3205 = CARTESIAN_POINT ( 'NONE',  ( -33.57168893143874300, -5.326829507069609448, -8.556972795487428840 ) ) ;
#3206 = EDGE_CURVE ( 'NONE', #860, #31932, #12254, .T. ) ;
#3207 = CARTESIAN_POINT ( 'NONE',  ( -12.60925743039346969, 20.19802119783879490, 19.66345542862530493 ) ) ;
#3208 = ORIENTED_EDGE ( 'NONE', *, *, #11173, .T. ) ;
#3209 = DIRECTION ( 'NONE',  ( 0.5000000000000038858, 0.8660254037844363761, -0.000000000000000000 ) ) ;
#3210 = CYLINDRICAL_SURFACE ( 'NONE', #21939, 0.5000000000000002220 ) ;
#3211 = CARTESIAN_POINT ( 'NONE',  ( -28.80707638399428916, 0.7099290160774374137, -10.67124776689043841 ) ) ;
#3212 = CARTESIAN_POINT ( 'NONE',  ( 28.79193172513320675, -11.56792772201013086, -14.76806894771908674 ) ) ;
#3213 = ORIENTED_EDGE ( 'NONE', *, *, #35941, .F. ) ;
#3214 = LINE ( 'NONE', #15006, #29724 ) ;
#3215 = ORIENTED_EDGE ( 'NONE', *, *, #25268, .F. ) ;
#3216 = CIRCLE ( 'NONE', #25910, 58.00000000000007816 ) ;
#3217 = FACE_OUTER_BOUND ( 'NONE', #14654, .T. ) ;
#3218 = CARTESIAN_POINT ( 'NONE',  ( 8.859192577249610068, 12.20922670554003631, 23.00000000000000000 ) ) ;
#3219 = EDGE_CURVE ( 'NONE', #24567, #35217, #30355, .T. ) ;
#3220 = DIRECTION ( 'NONE',  ( 0.000000000000000000, 0.000000000000000000, 1.000000000000000000 ) ) ;
#3221 = ORIENTED_EDGE ( 'NONE', *, *, #14900, .F. ) ;
#3222 = CARTESIAN_POINT ( 'NONE',  ( -3.069715041284517110, 27.64360125249429601, -17.62585475904647225 ) ) ;
#3223 = CARTESIAN_POINT ( 'NONE',  ( -33.51290647813895163, -3.280245463522580174, -4.999999999999997335 ) ) ;
#3224 = LINE ( 'NONE', #37747, #33206 ) ;
#3225 = ADVANCED_BREP_SHAPE_REPRESENTATION ( '', ( #34952, #24238 ), #27483 ) ;
#3226 = LINE ( 'NONE', #15615, #15655 ) ;
#3227 = CARTESIAN_POINT ( 'NONE',  ( 16.93876653066008586, 13.26377307663926963, -22.20805623995693168 ) ) ;
#3228 = CARTESIAN_POINT ( 'NONE',  ( 9.509799170644791744, 22.48628651136178647, -20.11318651558298143 ) ) ;
#3229 = EDGE_LOOP ( 'NONE', ( #22499, #24075, #23450 ) ) ;
#3230 = CARTESIAN_POINT ( 'NONE',  ( -21.24184681333255753, 12.71378638656511484, -5.967672426067079705 ) ) ;
#3231 = CARTESIAN_POINT ( 'NONE',  ( -4.441848239913464447, 24.85865334748893929, 23.00000000000000000 ) ) ;
#3232 = CARTESIAN_POINT ( 'NONE',  ( 9.633777947662931496, -18.14705080549017424, -28.70249247701261197 ) ) ;
#3233 = CARTESIAN_POINT ( 'NONE',  ( 12.62284334487383397, 42.89764170712515323, 9.500000000000000000 ) ) ;
#3234 = CARTESIAN_POINT ( 'NONE',  ( 10.99485921934411081, 17.45463166253034260, -28.07471671999386942 ) ) ;
#3235 = CARTESIAN_POINT ( 'NONE',  ( -8.937590682902627037, -20.71651963383551731, -30.00000000000000000 ) ) ;
#3236 = CARTESIAN_POINT ( 'NONE',  ( -10.10646936306323518, 32.94553861768095970, 10.49999999999999822 ) ) ;
#3238 = AXIS2_PLACEMENT_3D ( 'NONE', #10375, #27700, #19716 ) ;
#3237 = CARTESIAN_POINT ( 'NONE',  ( -10.96701088540842761, 17.31978028264472513, -29.34797854174667364 ) ) ;
#3239 = CARTESIAN_POINT ( 'NONE',  ( -23.78701751404137354, -26.53361121414976509, -6.322536473355526709 ) ) ;
#3240 = CARTESIAN_POINT ( 'NONE',  ( 10.44141302741376798, -25.11139197116317590, -9.299239282066768197 ) ) ;
#3241 = CARTESIAN_POINT ( 'NONE',  ( 11.19141198691837502, 17.56663717187159790, -26.83658983900039985 ) ) ;
#3242 = EDGE_CURVE ( 'NONE', #7627, #12011, #36253, .T. ) ;
#3243 = CARTESIAN_POINT ( 'NONE',  ( 29.12903154260688154, -21.06488189102506681, -10.18399402962615596 ) ) ;
#3244 = CARTESIAN_POINT ( 'NONE',  ( 5.632984386902417206, 36.38118674759823534, 10.68306085400105587 ) ) ;
#3245 = EDGE_LOOP ( 'NONE', ( #18238, #565, #19994, #26314 ) ) ;
#3246 = CIRCLE ( 'NONE', #34393, 1.000000000000000888 ) ;
#3247 = CARTESIAN_POINT ( 'NONE',  ( -11.11602857932560262, 33.89154083561517439, -6.322138485960394405 ) ) ;
#3248 = CARTESIAN_POINT ( 'NONE',  ( -14.85188145504476687, 20.30462949162108544, 10.49999999999999822 ) ) ;
#3249 = CARTESIAN_POINT ( 'NONE',  ( 8.633502029282041690, 11.46765470489692795, 7.500000000000000888 ) ) ;
#3250 = CARTESIAN_POINT ( 'NONE',  ( 11.62435565298210882, 14.63397459621550922, 10.50000000000000000 ) ) ;
#3251 = EDGE_LOOP ( 'NONE', ( #15723, #19590, #5631, #7044 ) ) ;
#3252 = CARTESIAN_POINT ( 'NONE',  ( 22.21294924997172515, 0.6970241196614612722, -22.73910473975576707 ) ) ;
#3253 = CARTESIAN_POINT ( 'NONE',  ( 11.77929587896052155, 31.08767655398733254, 7.000000000000000000 ) ) ;
#3254 = LINE ( 'NONE', #28033, #7645 ) ;
#3255 = EDGE_LOOP ( 'NONE', ( #22229, #30777, #5734, #23474 ) ) ;
#3256 = CARTESIAN_POINT ( 'NONE',  ( -30.43251338895703739, 0.04316722816340590879, -7.828164403897452495 ) ) ;
#3257 = DIRECTION ( 'NONE',  ( 1.000000000000000000, 0.000000000000000000, 0.000000000000000000 ) ) ;
#3258 = ORIENTED_EDGE ( 'NONE', *, *, #944, .T. ) ;
#3259 = CARTESIAN_POINT ( 'NONE',  ( 23.50560939881936662, -4.852381968592491823, -21.00978952430008562 ) ) ;
#3260 = VERTEX_POINT ( 'NONE', #14712 ) ;
#3261 = CARTESIAN_POINT ( 'NONE',  ( -1.435176708165770409E-13, 40.16401087634232425, 13.32518128616608699 ) ) ;
#3262 = LINE ( 'NONE', #34348, #39780 ) ;
#3263 = DIRECTION ( 'NONE',  ( 1.000000000000000000, 0.000000000000000000, 0.000000000000000000 ) ) ;
#3264 = CARTESIAN_POINT ( 'NONE',  ( -1.073573824165845014, 32.41755745572908154, 20.25080042701565830 ) ) ;
#3265 = CARTESIAN_POINT ( 'NONE',  ( 5.440908595777819379, 35.94977745735560859, 11.00000000000000000 ) ) ;
#3266 = ORIENTED_EDGE ( 'NONE', *, *, #34375, .F. ) ;
#3267 = CARTESIAN_POINT ( 'NONE',  ( 0.000000000000000000, 22.50000000000000355, 7.000000000000000000 ) ) ;
#3268 = EDGE_CURVE ( 'NONE', #14685, #23635, #12540, .T. ) ;
#3269 = DIRECTION ( 'NONE',  ( 1.000000000000000000, 0.000000000000000000, 0.000000000000000000 ) ) ;
#3270 = CARTESIAN_POINT ( 'NONE',  ( 12.67417846324118358, 14.47720745114811436, 7.499999999999997335 ) ) ;
#3271 = AXIS2_PLACEMENT_3D ( 'NONE', #29550, #14107, #2127 ) ;
#3272 = DIRECTION ( 'NONE',  ( 0.000000000000000000, 0.000000000000000000, 1.000000000000000000 ) ) ;
#3273 = CARTESIAN_POINT ( 'NONE',  ( 9.798388895788875175, 34.03070998536941261, -8.489266934394210651 ) ) ;
#3274 = EDGE_CURVE ( 'NONE', #30348, #6928, #15106, .T. ) ;
#3275 = CARTESIAN_POINT ( 'NONE',  ( 17.12764558049190100, -26.53140043480064492, -8.684859237404365828 ) ) ;
#3276 = DIRECTION ( 'NONE',  ( 0.000000000000000000, 0.000000000000000000, 1.000000000000000000 ) ) ;
#3277 = CYLINDRICAL_SURFACE ( 'NONE', #19321, 6.000000000000003553 ) ;
#3278 = ORIENTED_EDGE ( 'NONE', *, *, #32069, .T. ) ;
#3279 = CARTESIAN_POINT ( 'NONE',  ( -13.61578127026913698, 22.57276738262792648, -15.46832451228934069 ) ) ;
#3280 = AXIS2_PLACEMENT_3D ( 'NONE', #25842, #3512, #37644 ) ;
#3281 = CARTESIAN_POINT ( 'NONE',  ( -32.73577250672335026, -2.961872765701405008, 16.87380292611397081 ) ) ;
#3282 = CARTESIAN_POINT ( 'NONE',  ( 10.35736673620512782, -19.62758828036890435, -22.75676071015052315 ) ) ;
#3283 = AXIS2_PLACEMENT_3D ( 'NONE', #15758, #28149, #25101 ) ;
#3284 = CARTESIAN_POINT ( 'NONE',  ( -3.853172919594720192, 21.57294901687549427, 13.00000000000000178 ) ) ;
#3285 = ORIENTED_EDGE ( 'NONE', *, *, #8355, .T. ) ;
#3286 = ORIENTED_EDGE ( 'NONE', *, *, #35387, .F. ) ;
#3287 = CARTESIAN_POINT ( 'NONE',  ( -9.436104724621630524, 18.21145219648997227, -29.99999999999999289 ) ) ;
#3288 = CARTESIAN_POINT ( 'NONE',  ( -19.44481637110248684, -27.25456932391892906, -5.912071530470661251 ) ) ;
#3289 = FACE_BOUND ( 'NONE', #32379, .T. ) ;
#3290 = VERTEX_POINT ( 'NONE', #18358 ) ;
#3291 = CARTESIAN_POINT ( 'NONE',  ( -29.17235460288958393, -8.104917298035191564, -14.85913705212063718 ) ) ;
#3292 = CARTESIAN_POINT ( 'NONE',  ( -9.537820998814829920, -18.38128399093912790, -27.45372482522294888 ) ) ;
#3293 = CARTESIAN_POINT ( 'NONE',  ( 13.81820544359399427, 28.33708565239886212, 7.102637441331454582 ) ) ;
#3294 = VERTEX_POINT ( 'NONE', #2124 ) ;
#3295 = CARTESIAN_POINT ( 'NONE',  ( 20.79851487167647406, 1.023505283316706205, -26.84526378395030832 ) ) ;
#3296 = CARTESIAN_POINT ( 'NONE',  ( 6.330070799514983193, 27.28854476845134513, 6.000000000000000000 ) ) ;
#3297 = CARTESIAN_POINT ( 'NONE',  ( -0.6237384431625470071, 19.56555719779890978, 13.00000000000000178 ) ) ;
#3298 = ADVANCED_FACE ( 'NONE', ( #9211 ), #27690, .F. ) ;
#3299 = VECTOR ( 'NONE', #34752, 1000.000000000000000 ) ;
#3300 = ORIENTED_EDGE ( 'NONE', *, *, #38411, .F. ) ;
#3301 = CARTESIAN_POINT ( 'NONE',  ( -20.61300406095988791, 0.8049965435648878120, -28.07524117914642403 ) ) ;
#3302 = EDGE_LOOP ( 'NONE', ( #37285, #21030, #2107, #38367 ) ) ;
#3303 = CARTESIAN_POINT ( 'NONE',  ( 32.71205163220476919, -2.303786481711429968, -5.920339140041507520 ) ) ;
#3304 = CARTESIAN_POINT ( 'NONE',  ( 1.082866184310819824, -20.47455923100120856, -30.00000000000001066 ) ) ;
#3305 = CARTESIAN_POINT ( 'NONE',  ( 32.69618749603090890, -17.08296528845530560, 17.92354375535250810 ) ) ;
#3306 = ORIENTED_EDGE ( 'NONE', *, *, #37334, .T. ) ;
#3307 = CARTESIAN_POINT ( 'NONE',  ( -24.01388090513056994, 4.332455551302775376, -15.73336986319053388 ) ) ;
#3308 = CARTESIAN_POINT ( 'NONE',  ( -14.47475276859717219, 26.43532618598166906, 7.470075214869918767 ) ) ;
#3309 = CARTESIAN_POINT ( 'NONE',  ( -13.49038105676663868, 15.86602540378456361, 10.49999999999999822 ) ) ;
#3310 = DIRECTION ( 'NONE',  ( 1.000000000000000000, 0.000000000000000000, 0.000000000000000000 ) ) ;
#3311 = VECTOR ( 'NONE', #22188, 1000.000000000000000 ) ;
#3312 = ADVANCED_FACE ( 'NONE', ( #39286 ), #27493, .F. ) ;
#3313 = DIRECTION ( 'NONE',  ( 0.5877852522924796874, 0.8090169943749426773, 0.000000000000000000 ) ) ;
#3314 = PRODUCT_DEFINITION ( 'UNKNOWN', '', #28786, #48 ) ;
#3315 = CARTESIAN_POINT ( 'NONE',  ( -11.54666566735211752, 32.07468077621347646, 7.500000000000004441 ) ) ;
#3316 = EDGE_CURVE ( 'NONE', #7248, #23537, #33415, .T. ) ;
#3317 = CARTESIAN_POINT ( 'NONE',  ( 25.26292323896833381, 8.700328014641888430, 13.92931973827844416 ) ) ;
#3318 = CARTESIAN_POINT ( 'NONE',  ( -19.51080979133228510, 6.405414381276935742, -28.83855153441879438 ) ) ;
#3319 = CYLINDRICAL_SURFACE ( 'NONE', #23539, 1.000000000000000000 ) ;
#3320 = EDGE_CURVE ( 'NONE', #16453, #32987, #8581, .T. ) ;
#3321 = DIRECTION ( 'NONE',  ( -0.3090169943749457304, 0.9510565162951540863, 0.000000000000000000 ) ) ;
#3322 = CARTESIAN_POINT ( 'NONE',  ( 13.88564487354877031, -15.37443428294943537, -27.83446942326135343 ) ) ;
#3323 = AXIS2_PLACEMENT_3D ( 'NONE', #13559, #4218, #19252 ) ;
#3324 = FACE_OUTER_BOUND ( 'NONE', #17500, .T. ) ;
#3325 = CARTESIAN_POINT ( 'NONE',  ( 15.30622479779250256, 27.07165865151032591, -5.942729527624186936 ) ) ;
#3326 = ORIENTED_EDGE ( 'NONE', *, *, #2667, .F. ) ;
#3327 = CARTESIAN_POINT ( 'NONE',  ( -16.22408403259154852, 24.10865257618694102, -5.474343353774658638 ) ) ;
#3328 = CARTESIAN_POINT ( 'NONE',  ( -27.24589624691908440, -6.395450141004457301, 20.50957957746007665 ) ) ;
#3329 = CARTESIAN_POINT ( 'NONE',  ( -0.5000000000000004441, 33.00000000000000000, 10.00000000000000000 ) ) ;
#3330 = CARTESIAN_POINT ( 'NONE',  ( 15.42009615191692085, 26.67611678986924062, -5.946089587727700021 ) ) ;
#3331 = ORIENTED_EDGE ( 'NONE', *, *, #20332, .T. ) ;
#3332 = CARTESIAN_POINT ( 'NONE',  ( -36.48557158514989140, -11.24999999999987743, 6.000000000000000000 ) ) ;
#3333 = ORIENTED_EDGE ( 'NONE', *, *, #32867, .F. ) ;
#3335 = DIRECTION ( 'NONE',  ( -1.000000000000000000, 0.000000000000000000, 0.000000000000000000 ) ) ;
#3334 = CARTESIAN_POINT ( 'NONE',  ( -10.83390719878747355, 17.40340976726015398, -29.34510724894995093 ) ) ;
#3336 = CARTESIAN_POINT ( 'NONE',  ( -12.82118876533016838, -22.56181011573424300, -16.42547678194880945 ) ) ;
#3337 = DIRECTION ( 'NONE',  ( 0.000000000000000000, 0.000000000000000000, 1.000000000000000000 ) ) ;
#3338 = VERTEX_POINT ( 'NONE', #39488 ) ;
#3339 = CARTESIAN_POINT ( 'NONE',  ( -18.15436357158603897, -9.522238560471441460, -29.21298683338178037 ) ) ;
#3340 = CARTESIAN_POINT ( 'NONE',  ( -10.98011883110523712, -24.81730312888366186, -10.73332943874482659 ) ) ;
#3341 = DIRECTION ( 'NONE',  ( 1.000000000000000000, 0.000000000000000000, 0.000000000000000000 ) ) ;
#3342 = CARTESIAN_POINT ( 'NONE',  ( 12.73900707961357170, 16.26579194631107228, -27.56360065120206571 ) ) ;
#3343 = ORIENTED_EDGE ( 'NONE', *, *, #21458, .T. ) ;
#3344 = CARTESIAN_POINT ( 'NONE',  ( 22.23426282729013792, 5.324047925142390447, -18.87963228197226329 ) ) ;
#3345 = AXIS2_PLACEMENT_3D ( 'NONE', #22944, #32300, #38189 ) ;
#3346 = DIRECTION ( 'NONE',  ( 0.000000000000000000, 0.000000000000000000, 1.000000000000000000 ) ) ;
#3347 = EDGE_CURVE ( 'NONE', #42, #35381, #31292, .T. ) ;
#3348 = EDGE_CURVE ( 'NONE', #3653, #11472, #24447, .T. ) ;
#3349 = CARTESIAN_POINT ( 'NONE',  ( -9.363324537585851814, 32.27640801132209702, 10.50000000000000000 ) ) ;
#3350 = EDGE_LOOP ( 'NONE', ( #14030, #15005, #33607, #23429 ) ) ;
#3351 = CARTESIAN_POINT ( 'NONE',  ( -30.99844456375071289, -0.3171783591690320869, -6.879640249969712684 ) ) ;
#3352 = CARTESIAN_POINT ( 'NONE',  ( 21.75224751592035588, 0.4974273606728234487, -23.82583798890098592 ) ) ;
#3353 = CARTESIAN_POINT ( 'NONE',  ( 26.96432039561798533, -11.11241571815020279, 20.82122704794079837 ) ) ;
#3354 = ORIENTED_EDGE ( 'NONE', *, *, #31722, .F. ) ;
#3355 = AXIS2_PLACEMENT_3D ( 'NONE', #20751, #26629, #32334 ) ;
#3356 = CARTESIAN_POINT ( 'NONE',  ( -35.36940577612494963, -20.42053594592269761, -4.999999999999990230 ) ) ;
#3357 = CYLINDRICAL_SURFACE ( 'NONE', #22545, 0.5000000000000004441 ) ;
#3358 = ORIENTED_EDGE ( 'NONE', *, *, #16307, .T. ) ;
#3359 = LINE ( 'NONE', #15557, #917 ) ;
#3360 = ADVANCED_FACE ( 'NONE', ( #40080 ), #8612, .T. ) ;
#3361 = APPLICATION_CONTEXT ( 'automotive_design' ) ;
#3362 = FACE_OUTER_BOUND ( 'NONE', #18698, .T. ) ;
#3363 = CARTESIAN_POINT ( 'NONE',  ( -1.871208588069141143, 13.69667159339610762, 12.00000000000000000 ) ) ;
#3364 = CARTESIAN_POINT ( 'NONE',  ( 3.871220829879935099, 38.02450267464935507, -5.000000000000000000 ) ) ;
#3365 = CARTESIAN_POINT ( 'NONE',  ( -7.330077540933487512, 17.71145523154927659, 12.00000000000000000 ) ) ;
#3366 = DIRECTION ( 'NONE',  ( 0.000000000000000000, 0.000000000000000000, 1.000000000000000000 ) ) ;
#3367 = DIRECTION ( 'NONE',  ( 0.000000000000000000, -0.000000000000000000, 1.000000000000000000 ) ) ;
#3369 = EDGE_CURVE ( 'NONE', #35589, #19392, #32362, .T. ) ;
#3368 = CARTESIAN_POINT ( 'NONE',  ( 7.014595103779618590, 35.79644522156321784, 11.00000000000000000 ) ) ;
#3370 = LINE ( 'NONE', #28153, #21600 ) ;
#3371 = DIRECTION ( 'NONE',  ( -0.9510565162951504226, 0.3090169943749573322, 0.000000000000000000 ) ) ;
#3372 = CARTESIAN_POINT ( 'NONE',  ( 14.92380366935343972, 27.88910720575894686, -6.861436071230456513 ) ) ;
#3373 = CARTESIAN_POINT ( 'NONE',  ( 13.30736791475921699, 15.68301270237638967, 10.49999999999999822 ) ) ;
#3374 = ORIENTED_EDGE ( 'NONE', *, *, #24516, .F. ) ;
#3376 = CARTESIAN_POINT ( 'NONE',  ( -0.7344975573282397363, 36.24516302788250499, 12.00000000000000000 ) ) ;
#3375 = CARTESIAN_POINT ( 'NONE',  ( -15.08898831634408744, 14.27233443605820540, -26.54181874479749226 ) ) ;
#3377 = CARTESIAN_POINT ( 'NONE',  ( 13.20348688925205316, 15.99217894729783929, 10.49999999999999822 ) ) ;
#3378 = AXIS2_PLACEMENT_3D ( 'NONE', #30403, #18012, #40124 ) ;
#3379 = CARTESIAN_POINT ( 'NONE',  ( 11.51930939957287059, -20.97998600509406586, -19.49970475651661417 ) ) ;
#3380 = CARTESIAN_POINT ( 'NONE',  ( -17.40676172239622588, -21.99313558790002787, -16.01693467188644959 ) ) ;
#3381 = CARTESIAN_POINT ( 'NONE',  ( 15.10367708458470126, 26.13036639895321045, -8.767987560003460246 ) ) ;
#3382 = CARTESIAN_POINT ( 'NONE',  ( 11.02561053197542407, 17.43447018294412487, -28.07655181465922567 ) ) ;
#3383 = ORIENTED_EDGE ( 'NONE', *, *, #17215, .T. ) ;
#3384 = CARTESIAN_POINT ( 'NONE',  ( 3.724371395536106188, 32.23037938972932892, 12.00000000000000000 ) ) ;
#3385 = CARTESIAN_POINT ( 'NONE',  ( -10.48080051920513611, -19.59187828654420116, -22.74178688489114819 ) ) ;
#3386 = CARTESIAN_POINT ( 'NONE',  ( -15.03860650580583780, -28.48662463501947428, 12.73282698324853257 ) ) ;
#3387 = CIRCLE ( 'NONE', #9278, 1.000000000000000444 ) ;
#3388 = CARTESIAN_POINT ( 'NONE',  ( -29.96597079672651631, -20.69995294692298415, -9.731940980083196635 ) ) ;
#3389 = CARTESIAN_POINT ( 'NONE',  ( 1.364045841937116643, -21.42539740769312928, -22.25265589050333404 ) ) ;
#3390 = CARTESIAN_POINT ( 'NONE',  ( 11.35751580965241914, 17.11731054519655970, -28.72129911532366364 ) ) ;
#3391 = CARTESIAN_POINT ( 'NONE',  ( 22.79531528405124163, 10.15988774222570434, -5.482352800657483094 ) ) ;
#3392 = CARTESIAN_POINT ( 'NONE',  ( 11.54200800595913456, 31.54683795827724424, 10.49999999999999822 ) ) ;
#3393 = ORIENTED_EDGE ( 'NONE', *, *, #31603, .T. ) ;
#3394 = CARTESIAN_POINT ( 'NONE',  ( -26.51515768098519743, -2.574357228626084293, -17.10477876855104284 ) ) ;
#3395 = EDGE_CURVE ( 'NONE', #31091, #11163, #21401, .T. ) ;
#3396 = CARTESIAN_POINT ( 'NONE',  ( -16.89748511972594258, 9.755767582500416424, 19.99202127657103389 ) ) ;
#3397 = VECTOR ( 'NONE', #19157, 1000.000000000000000 ) ;
#3398 = VERTEX_POINT ( 'NONE', #10205 ) ;
#3399 = CARTESIAN_POINT ( 'NONE',  ( 2.441045247299091336, 7.699747138389255063, 7.485699520496970294 ) ) ;
#3400 = CARTESIAN_POINT ( 'NONE',  ( 9.559505275947156377, 25.28115294937476065, 12.00000000000000000 ) ) ;
#3401 = CARTESIAN_POINT ( 'NONE',  ( -20.45512865215935960, 1.365572444264179452, -29.35734819944713081 ) ) ;
#3402 = CARTESIAN_POINT ( 'NONE',  ( 35.06506416243693280, -12.90429163527686285, -7.138145798991673452 ) ) ;
#3403 = CARTESIAN_POINT ( 'NONE',  ( 36.80210562958740184, -14.73639196410467100, 13.32518128616608877 ) ) ;
#3404 = ORIENTED_EDGE ( 'NONE', *, *, #16213, .F. ) ;
#3405 = CONICAL_SURFACE ( 'NONE', #18355, 0.4999999999999961142, 0.7853981633974473908 ) ;
#3406 = FACE_OUTER_BOUND ( 'NONE', #29927, .T. ) ;
#3407 = EDGE_LOOP ( 'NONE', ( #26062, #32980, #28248, #27448 ) ) ;
#3408 = CYLINDRICAL_SURFACE ( 'NONE', #27489, 6.000000000000010658 ) ;
#3409 = DIRECTION ( 'NONE',  ( -1.000000000000000000, 0.000000000000000000, 0.000000000000000000 ) ) ;
#3410 = ADVANCED_FACE ( 'NONE', ( #863 ), #12452, .F. ) ;
#3411 = AXIS2_PLACEMENT_3D ( 'NONE', #22976, #22368, #31323 ) ;
#3412 = DIRECTION ( 'NONE',  ( -1.000000000000000000, 0.000000000000000000, 0.000000000000000000 ) ) ;
#3413 = EDGE_LOOP ( 'NONE', ( #16065, #8742, #17773, #425 ) ) ;
#3414 = EDGE_CURVE ( 'NONE', #9720, #37780, #26131, .T. ) ;
#3415 = CARTESIAN_POINT ( 'NONE',  ( -2.404449847303043786, 21.86890924017041016, -24.25077898173865520 ) ) ;
#3416 = CARTESIAN_POINT ( 'NONE',  ( -35.48557158208988938, -9.180432008922831955, -4.999999999999999112 ) ) ;
#3417 = DIRECTION ( 'NONE',  ( -0.4156269377774573504, -0.5720614028176800314, -0.7071067811865487940 ) ) ;
#3418 = DIRECTION ( 'NONE',  ( -0.000000000000000000, -0.000000000000000000, -1.000000000000000000 ) ) ;
#3419 = DIRECTION ( 'NONE',  ( 1.000000000000000000, 0.000000000000000000, 0.000000000000000000 ) ) ;
#3420 = CARTESIAN_POINT ( 'NONE',  ( 19.48557158514975285, -11.24999999999995737, 10.00000000000000000 ) ) ;
#3421 = CARTESIAN_POINT ( 'NONE',  ( 9.798481364371980362, 21.31715715824844892, -21.26624317740214209 ) ) ;
#3422 = ORIENTED_EDGE ( 'NONE', *, *, #639, .T. ) ;
#3423 = EDGE_CURVE ( 'NONE', #8840, #36419, #20204, .T. ) ;
#3424 = CARTESIAN_POINT ( 'NONE',  ( -20.53340956023616215, 13.54976128206928188, -8.407384701756129175 ) ) ;
#3425 = CARTESIAN_POINT ( 'NONE',  ( 8.437494165184368455, 40.76200631401353291, 22.99999999999999645 ) ) ;
#3426 = CARTESIAN_POINT ( 'NONE',  ( 9.684276948513423022, -18.21592224580517794, -28.07104506456108695 ) ) ;
#3427 = CARTESIAN_POINT ( 'NONE',  ( 15.00099999999999945, 32.50000000000000000, 10.00000000000000000 ) ) ;
#3428 = CARTESIAN_POINT ( 'NONE',  ( 14.00096064495863857, 24.00543594118468249, -13.50663270117560266 ) ) ;
#3429 = CARTESIAN_POINT ( 'NONE',  ( 15.72991998290128990, -16.18894361744929000, -29.99999999999998579 ) ) ;
#3430 = DIRECTION ( 'NONE',  ( 0.7431448254773953543, 0.6691306063588570163, -0.000000000000000000 ) ) ;
#3431 = AXIS2_PLACEMENT_3D ( 'NONE', #20422, #36457, #11077 ) ;
#3432 = CARTESIAN_POINT ( 'NONE',  ( -25.47853931120452131, -25.38973540270632512, -8.036541765355776690 ) ) ;
#3433 = CARTESIAN_POINT ( 'NONE',  ( 12.61343103759603324, -25.39092838429157695, -9.744532428759812959 ) ) ;
#3434 = CARTESIAN_POINT ( 'NONE',  ( 11.05718465110185988, 17.26235906992462787, -29.34992143215759697 ) ) ;
#3435 = CARTESIAN_POINT ( 'NONE',  ( 30.70013347194538511, -22.17214586171431989, -7.124165660199366812 ) ) ;
#3436 = VECTOR ( 'NONE', #12673, 1000.000000000000000 ) ;
#3437 = CARTESIAN_POINT ( 'NONE',  ( 8.317671217785902016, 10.20105690706387591, 10.87262190629280489 ) ) ;
#3438 = CARTESIAN_POINT ( 'NONE',  ( -35.48105285891828231, 0.8254987174888869239, 11.00000000000000355 ) ) ;
#3439 = ORIENTED_EDGE ( 'NONE', *, *, #18782, .F. ) ;
#3440 = CARTESIAN_POINT ( 'NONE',  ( -10.57541166117252729, 32.01915677600736387, -10.30941365822858202 ) ) ;
#3441 = EDGE_CURVE ( 'NONE', #19220, #4159, #8599, .T. ) ;
#3442 = DIRECTION ( 'NONE',  ( 0.1470157664651934593, -0.6916548014802230693, -0.7071067811865510144 ) ) ;
#3443 = DIRECTION ( 'NONE',  ( 1.000000000000000000, 0.000000000000000000, 0.000000000000000000 ) ) ;
#3444 = EDGE_CURVE ( 'NONE', #8510, #20949, #25043, .T. ) ;
#3445 = AXIS2_PLACEMENT_3D ( 'NONE', #16456, #420, #37988 ) ;
#3446 = DIRECTION ( 'NONE',  ( 0.000000000000000000, 0.000000000000000000, 1.000000000000000000 ) ) ;
#3447 = EDGE_LOOP ( 'NONE', ( #937, #35537, #39151, #28477 ) ) ;
#3448 = CARTESIAN_POINT ( 'NONE',  ( 30.58188266183778836, 0.01734648026565401360, -7.358011334378191215 ) ) ;
#3449 = CARTESIAN_POINT ( 'NONE',  ( 14.58225150643707835, 26.01772713467079612, 7.202682876670051471 ) ) ;
#3450 = CARTESIAN_POINT ( 'NONE',  ( -5.440908595777636414, 35.94977745735568675, 7.000000000000000000 ) ) ;
#3451 = VERTEX_POINT ( 'NONE', #6941 ) ;
#3452 = CARTESIAN_POINT ( 'NONE',  ( -29.56002673421212634, 0.09025702458776063697, -10.18136869063499894 ) ) ;
#3453 = DIRECTION ( 'NONE',  ( 1.000000000000000000, 0.000000000000000000, 0.000000000000000000 ) ) ;
#3454 = VECTOR ( 'NONE', #9475, 1000.000000000000114 ) ;
#3455 = VERTEX_POINT ( 'NONE', #25431 ) ;
#3456 = CARTESIAN_POINT ( 'NONE',  ( 33.58038907436841214, -6.003017191285483278, -8.986547828497519319 ) ) ;
#3457 = VECTOR ( 'NONE', #37884, 1000.000000000000000 ) ;
#3458 = EDGE_LOOP ( 'NONE', ( #36985, #9159, #21688, #29766 ) ) ;
#3459 = CARTESIAN_POINT ( 'NONE',  ( 5.638963013753452991, 39.23975437003361577, 13.32518128616608877 ) ) ;
#3460 = DIRECTION ( 'NONE',  ( 1.000000000000000000, 0.000000000000000000, 0.000000000000000000 ) ) ;
#3461 = DIRECTION ( 'NONE',  ( 1.000000000000000000, 0.000000000000000000, -0.000000000000000000 ) ) ;
#3462 = EDGE_CURVE ( 'NONE', #16093, #27294, #30947, .T. ) ;
#3463 = CARTESIAN_POINT ( 'NONE',  ( 12.17657648715484164, 27.34841683166593640, 18.87996532025935892 ) ) ;
#3464 = CIRCLE ( 'NONE', #4098, 0.5000000000000000000 ) ;
#3465 = DIRECTION ( 'NONE',  ( 1.000000000000000000, 0.000000000000000000, 0.000000000000000000 ) ) ;
#3466 = ORIENTED_EDGE ( 'NONE', *, *, #25058, .F. ) ;
#3467 = EDGE_CURVE ( 'NONE', #18499, #8101, #28942, .T. ) ;
#3468 = CARTESIAN_POINT ( 'NONE',  ( 3.523049899833284648, 8.330220536420911870, 10.99387789255784220 ) ) ;
#3469 = CARTESIAN_POINT ( 'NONE',  ( -6.675012889388576731, 19.39409273962604985, -29.99999999999996803 ) ) ;
#3470 = CARTESIAN_POINT ( 'NONE',  ( 1.853166178176219203, 23.42705098312512746, 6.000000000000000000 ) ) ;
#3471 = LINE ( 'NONE', #6703, #38331 ) ;
#3472 = CARTESIAN_POINT ( 'NONE',  ( 16.23240241217962065, 17.80559144519626003, -15.77666076426317154 ) ) ;
#3473 = CARTESIAN_POINT ( 'NONE',  ( 9.133087869482302779, 35.68701272469542829, -5.442357614005382871 ) ) ;
#3474 = AXIS2_PLACEMENT_3D ( 'NONE', #37342, #34893, #9717 ) ;
#3475 = CARTESIAN_POINT ( 'NONE',  ( 16.53758848021426076, -26.97586464850826005, -5.000000000000002665 ) ) ;
#3476 = CARTESIAN_POINT ( 'NONE',  ( 30.90412082983250741, -0.04211290444289771118, -5.000000000000000000 ) ) ;
#3477 = LINE ( 'NONE', #3675, #20655 ) ;
#3478 = ORIENTED_EDGE ( 'NONE', *, *, #25524, .T. ) ;
#3479 = CARTESIAN_POINT ( 'NONE',  ( -14.30582960071693321, 24.43380170945625096, -12.55177947368377467 ) ) ;
#3480 = AXIS2_PLACEMENT_3D ( 'NONE', #37247, #6163, #18566 ) ;
#3481 = CARTESIAN_POINT ( 'NONE',  ( -35.04992612853192924, -12.66836002548420304, 16.87380292611438648 ) ) ;
#3482 = CARTESIAN_POINT ( 'NONE',  ( 14.34480155068720286, -25.40677281950577537, -10.65920629769117411 ) ) ;
#3483 = CARTESIAN_POINT ( 'NONE',  ( -6.151085731882352192, 35.08626808545859888, 9.500000000000000000 ) ) ;
#3484 = ORIENTED_EDGE ( 'NONE', *, *, #36732, .T. ) ;
#3485 = ORIENTED_EDGE ( 'NONE', *, *, #35941, .T. ) ;
#3486 = CARTESIAN_POINT ( 'NONE',  ( -11.60722801024130746, 21.49292312996424315, -19.33865458767208168 ) ) ;
#3487 = CARTESIAN_POINT ( 'NONE',  ( -11.95652123975070324, -18.48273786211390401, -23.63287802302393814 ) ) ;
#3488 = FACE_BOUND ( 'NONE', #33804, .T. ) ;
#3489 = CIRCLE ( 'NONE', #12567, 1.000000000000000000 ) ;
#3490 = EDGE_LOOP ( 'NONE', ( #23406, #39452, #6688, #13183 ) ) ;
#3491 = CARTESIAN_POINT ( 'NONE',  ( -35.33786424633182577, -8.799366064169335644, -5.000000000000002665 ) ) ;
#3492 = CARTESIAN_POINT ( 'NONE',  ( -15.22285490720163459, -26.55223875496663055, -6.888230830752624101 ) ) ;
#3493 = DIRECTION ( 'NONE',  ( 0.000000000000000000, 0.000000000000000000, 1.000000000000000000 ) ) ;
#3494 = ORIENTED_EDGE ( 'NONE', *, *, #25374, .F. ) ;
#3495 = CARTESIAN_POINT ( 'NONE',  ( 20.73556080916292998, 1.704149916198021142, -26.89632919872368788 ) ) ;
#3496 = CARTESIAN_POINT ( 'NONE',  ( -14.31603901957233660, 19.98981538725089990, 7.000000000000000000 ) ) ;
#3497 = DIRECTION ( 'NONE',  ( 1.000000000000000000, 0.000000000000000000, 0.000000000000000000 ) ) ;
#3498 = ADVANCED_FACE ( 'NONE', ( #28088 ), #12850, .F. ) ;
#3499 = ORIENTED_EDGE ( 'NONE', *, *, #23517, .F. ) ;
#3500 = CARTESIAN_POINT ( 'NONE',  ( -22.22587217777541468, 0.6446291972866406983, -22.73257526237749104 ) ) ;
#3501 = VERTEX_POINT ( 'NONE', #25633 ) ;
#3502 = CARTESIAN_POINT ( 'NONE',  ( 21.94068861260580405, -0.7738519978160267598, -23.67308330514575943 ) ) ;
#3503 = CIRCLE ( 'NONE', #4813, 1.000000000000000888 ) ;
#3504 = CARTESIAN_POINT ( 'NONE',  ( 0.7366931383309426318, -20.49029098293467754, -30.00000000000001066 ) ) ;
#3505 = CARTESIAN_POINT ( 'NONE',  ( 33.89025995733786090, -4.271010277521167353, 16.30093088680190760 ) ) ;
#3506 = EDGE_LOOP ( 'NONE', ( #34875, #4502, #3644, #36933 ) ) ;
#3507 = CARTESIAN_POINT ( 'NONE',  ( -21.18796512248286490, 4.297847109112478137, -23.09674402144054994 ) ) ;
#3508 = CARTESIAN_POINT ( 'NONE',  ( -14.58494835919645993, 26.00628811930699413, 7.192820069705969210 ) ) ;
#3509 = CARTESIAN_POINT ( 'NONE',  ( -2.109373541296185373, 27.06550157850340810, 20.99999999999999645 ) ) ;
#3510 = AXIS2_PLACEMENT_3D ( 'NONE', #20574, #32969, #2281 ) ;
#3511 = CARTESIAN_POINT ( 'NONE',  ( -20.57924982997939622, -27.21273881503329051, -4.999999999999998224 ) ) ;
#3512 = DIRECTION ( 'NONE',  ( 0.000000000000000000, 0.000000000000000000, 1.000000000000000000 ) ) ;
#3513 = PRODUCT_DEFINITION_SHAPE ( 'NONE', 'NONE',  #40200 ) ;
#3514 = AXIS2_PLACEMENT_3D ( 'NONE', #35158, #1237, #35364 ) ;
#3515 = FACE_BOUND ( 'NONE', #19319, .T. ) ;
#3516 = DIRECTION ( 'NONE',  ( -0.000000000000000000, -0.000000000000000000, -1.000000000000000000 ) ) ;
#3517 = CARTESIAN_POINT ( 'NONE',  ( -24.28809745169647627, 7.043314632023327526, -9.848050643796884884 ) ) ;
#3518 = FACE_OUTER_BOUND ( 'NONE', #37865, .T. ) ;
#3519 = CARTESIAN_POINT ( 'NONE',  ( 22.96737774831856882, -25.31542735044140358, -9.848476247948095619 ) ) ;
#3520 = CARTESIAN_POINT ( 'NONE',  ( 1.547498115756713588, 8.004992253133169200, 7.000000000000000000 ) ) ;
#3521 = CARTESIAN_POINT ( 'NONE',  ( 14.63926748296054292, 25.68772099636430895, -10.63428425608140593 ) ) ;
#3522 = ORIENTED_EDGE ( 'NONE', *, *, #9208, .F. ) ;
#3523 = AXIS2_PLACEMENT_3D ( 'NONE', #30511, #31105, #18515 ) ;
#3524 = CARTESIAN_POINT ( 'NONE',  ( -12.71522534069617372, 17.33000003956545498, -24.02735807176059168 ) ) ;
#3525 = CARTESIAN_POINT ( 'NONE',  ( -26.67038870798852557, -5.578326634890662383, 20.50957957746030402 ) ) ;
#3526 = CARTESIAN_POINT ( 'NONE',  ( 7.577540944421576441, 33.15743037285414374, 6.000000000000000000 ) ) ;
#3527 = CARTESIAN_POINT ( 'NONE',  ( 11.09886981330870626, 17.48507009481504682, -27.44980206485566399 ) ) ;
#3528 = ORIENTED_EDGE ( 'NONE', *, *, #32151, .T. ) ;
#3529 = CYLINDRICAL_SURFACE ( 'NONE', #15126, 1.000000000000000000 ) ;
#3530 = ORIENTED_EDGE ( 'NONE', *, *, #33606, .F. ) ;
#3532 = LINE ( 'NONE', #6182, #24406 ) ;
#3531 = CARTESIAN_POINT ( 'NONE',  ( -11.16200477833207039, 18.15270254736048372, -24.99421180247795604 ) ) ;
#3533 = CARTESIAN_POINT ( 'NONE',  ( -15.01611103430922256, -25.86512146738518680, -9.701370320124519608 ) ) ;
#3534 = LINE ( 'NONE', #12876, #36110 ) ;
#3535 = ORIENTED_EDGE ( 'NONE', *, *, #21959, .T. ) ;
#3536 = CARTESIAN_POINT ( 'NONE',  ( -21.85483727830508016, -11.45635712499663050, -20.69655747118709854 ) ) ;
#3537 = CARTESIAN_POINT ( 'NONE',  ( -14.53723555501347064, -26.50432973120043911, -5.474040766214040232 ) ) ;
#3538 = CARTESIAN_POINT ( 'NONE',  ( -8.505700342264141511, 22.10876900990917804, 7.000000000000000000 ) ) ;
#3539 = CARTESIAN_POINT ( 'NONE',  ( 13.63685500492499436, 18.84978013948070341, -19.69852935831276852 ) ) ;
#3540 = ORIENTED_EDGE ( 'NONE', *, *, #2825, .F. ) ;
#3541 = CARTESIAN_POINT ( 'NONE',  ( 20.84739969530572878, 5.252202929258718456, -23.16050360519607665 ) ) ;
#3542 = EDGE_CURVE ( 'NONE', #34288, #2054, #34996, .T. ) ;
#3543 = LINE ( 'NONE', #9246, #21905 ) ;
#3544 = DIRECTION ( 'NONE',  ( 0.000000000000000000, 0.000000000000000000, 1.000000000000000000 ) ) ;
#3545 = CARTESIAN_POINT ( 'NONE',  ( 5.706335727061685681, 24.35410196624994583, 6.000000000000000000 ) ) ;
#3546 = ORIENTED_EDGE ( 'NONE', *, *, #1183, .T. ) ;
#3547 = CARTESIAN_POINT ( 'NONE',  ( -20.54032332987920029, 0.5213581391517280172, -28.69511755839404543 ) ) ;
#3548 = CONICAL_SURFACE ( 'NONE', #31446, 0.4999999999999997780, 0.7853981633974511656 ) ;
#3549 = CARTESIAN_POINT ( 'NONE',  ( 20.49022872340270851, 0.6388713974194965006, -30.00000000000000355 ) ) ;
#3550 = EDGE_CURVE ( 'NONE', #31065, #4676, #34394, .T. ) ;
#3551 = CARTESIAN_POINT ( 'NONE',  ( 27.53764137321996586, -17.13852093243014352, 20.25080042701566541 ) ) ;
#3552 = ORIENTED_EDGE ( 'NONE', *, *, #16350, .F. ) ;
#3553 = EDGE_CURVE ( 'NONE', #1139, #29890, #9808, .T. ) ;
#3554 = AXIS2_PLACEMENT_3D ( 'NONE', #28350, #31207, #25109 ) ;
#3555 = CARTESIAN_POINT ( 'NONE',  ( 20.55563217186196212, -29.52600041847795254, -5.000000000000015987 ) ) ;
#3556 = DIRECTION ( 'NONE',  ( 1.000000000000000000, 0.000000000000000000, 0.000000000000000000 ) ) ;
#3557 = VECTOR ( 'NONE', #10312, 1000.000000000000114 ) ;
#3558 = ORIENTED_EDGE ( 'NONE', *, *, #17104, .T. ) ;
#3559 = CARTESIAN_POINT ( 'NONE',  ( -7.611215932167763043, 18.68301270189229513, 9.000000000000001776 ) ) ;
#3560 = CARTESIAN_POINT ( 'NONE',  ( -11.14453731054088514, 31.86177010143615007, 11.00000000000000000 ) ) ;
#3561 = CARTESIAN_POINT ( 'NONE',  ( 14.96930490892014731, 21.54088032874976832, 7.000000000000000000 ) ) ;
#3562 = CARTESIAN_POINT ( 'NONE',  ( 5.356590097018567143, 32.51922113974988804, -12.93011007245527466 ) ) ;
#3563 = CARTESIAN_POINT ( 'NONE',  ( -6.577547685840081648, 11.84256962714647798, 13.00000000000000178 ) ) ;
#3564 = EDGE_CURVE ( 'NONE', #25343, #26836, #31339, .T. ) ;
#3565 = PLANE ( 'NONE',  #14979 ) ;
#3566 = EDGE_CURVE ( 'NONE', #2935, #11482, #34195, .T. ) ;
#3567 = DIRECTION ( 'NONE',  ( 0.000000000000000000, 0.000000000000000000, 1.000000000000000000 ) ) ;
#3568 = DIRECTION ( 'NONE',  ( 1.000000000000000000, 0.000000000000000000, 0.000000000000000000 ) ) ;
#3569 = FACE_OUTER_BOUND ( 'NONE', #12983, .T. ) ;
#3570 = FACE_OUTER_BOUND ( 'NONE', #7499, .T. ) ;
#3571 = CIRCLE ( 'NONE', #23681, 1.000000000000000000 ) ;
#3572 = CARTESIAN_POINT ( 'NONE',  ( 10.13018406787138304, 17.82246755199521360, -30.00000000000000000 ) ) ;
#3573 = DIRECTION ( 'NONE',  ( 0.2079116908177533751, -0.9781476007338069101, 0.000000000000000000 ) ) ;
#3574 = ORIENTED_EDGE ( 'NONE', *, *, #36374, .F. ) ;
#3576 = LINE ( 'NONE', #8882, #31744 ) ;
#3575 = CARTESIAN_POINT ( 'NONE',  ( -18.24281883325805609, 17.05300135009716556, -10.83830628367119253 ) ) ;
#3577 = LINE ( 'NONE', #37510, #24409 ) ;
#3578 = CARTESIAN_POINT ( 'NONE',  ( 15.17886553297244845, -26.37689987109310152, -7.828163835162226469 ) ) ;
#3579 = CARTESIAN_POINT ( 'NONE',  ( -12.82987974443481960, -16.39774487402648973, -27.21081390613418449 ) ) ;
#3580 = CARTESIAN_POINT ( 'NONE',  ( 11.03878455726499652, 17.42581041319601809, -28.07733810068035041 ) ) ;
#3581 = CARTESIAN_POINT ( 'NONE',  ( 11.16609885640999345, 17.76953549359777895, -26.22290328359227018 ) ) ;
#3582 = ORIENTED_EDGE ( 'NONE', *, *, #16560, .F. ) ;
#3583 = AXIS2_PLACEMENT_3D ( 'NONE', #28961, #3775, #736 ) ;
#3584 = CARTESIAN_POINT ( 'NONE',  ( 13.05736835487433289, 16.11602540378438420, 7.499999999999997335 ) ) ;
#3585 = CARTESIAN_POINT ( 'NONE',  ( -10.45876699675547705, -19.59826614722239313, -22.74446902591430586 ) ) ;
#3586 = CARTESIAN_POINT ( 'NONE',  ( -32.59722377598335896, -23.23978988006665958, 13.32518128616595909 ) ) ;
#3587 = VECTOR ( 'NONE', #19397, 999.9999999999998863 ) ;
#3588 = CIRCLE ( 'NONE', #30223, 1.000000000000000000 ) ;
#3589 = CARTESIAN_POINT ( 'NONE',  ( -16.22333673333531578, -12.66904231271439052, -28.46359972832643237 ) ) ;
#3590 = CARTESIAN_POINT ( 'NONE',  ( -2.045961664570402849, -21.89947875929911447, -20.11636488654603028 ) ) ;
#3591 = CARTESIAN_POINT ( 'NONE',  ( 15.67016653301135243, 25.89419373281741343, -5.474054512165222874 ) ) ;
#3592 = ORIENTED_EDGE ( 'NONE', *, *, #38567, .F. ) ;
#3593 = CARTESIAN_POINT ( 'NONE',  ( 18.66638796832185676, 8.717581921939480338, -27.73010582896804976 ) ) ;
#3594 = CARTESIAN_POINT ( 'NONE',  ( 18.23649648353767461, -16.09146789626181118, 23.00000000000000000 ) ) ;
#3595 = CARTESIAN_POINT ( 'NONE',  ( -9.401525468405969477, 34.87112330957656070, 16.87380292611441845 ) ) ;
#3596 = ORIENTED_EDGE ( 'NONE', *, *, #6124, .F. ) ;
#3597 = CARTESIAN_POINT ( 'NONE',  ( -32.09187415237648366, -4.172230308094091455, -10.40323351268730612 ) ) ;
#3598 = EDGE_CURVE ( 'NONE', #36223, #5248, #34588, .T. ) ;
#3599 = CARTESIAN_POINT ( 'NONE',  ( -25.49469310293981295, 2.228649397504699703, 18.42518152272610266 ) ) ;
#3600 = VERTEX_POINT ( 'NONE', #16103 ) ;
#3601 = DIRECTION ( 'NONE',  ( 0.000000000000000000, 0.000000000000000000, 1.000000000000000000 ) ) ;
#3602 = CARTESIAN_POINT ( 'NONE',  ( 23.54266556773325192, -14.22277663958715266, 23.00000000000000355 ) ) ;
#3603 = CARTESIAN_POINT ( 'NONE',  ( -29.38781521346863101, 0.8835198419403300640, -8.779238543596127542 ) ) ;
#3604 = CARTESIAN_POINT ( 'NONE',  ( 34.82234124989187052, -15.26616710914089303, -6.281458105108273848 ) ) ;
#3605 = CARTESIAN_POINT ( 'NONE',  ( 26.23899120466339951, -27.34191102820725661, 13.92931973827808356 ) ) ;
#3606 = VERTEX_POINT ( 'NONE', #28486 ) ;
#3607 = ORIENTED_EDGE ( 'NONE', *, *, #12440, .T. ) ;
#3608 = DIRECTION ( 'NONE',  ( 1.000000000000000000, 0.000000000000000000, 0.000000000000000000 ) ) ;
#3609 = AXIS2_PLACEMENT_3D ( 'NONE', #18185, #34412, #28506 ) ;
#3610 = CARTESIAN_POINT ( 'NONE',  ( 12.14716901145161643, 12.46304090461738667, 12.00000000000000000 ) ) ;
#3611 = VECTOR ( 'NONE', #27554, 999.9999999999998863 ) ;
#3612 = CIRCLE ( 'NONE', #39951, 0.5000000000000004441 ) ;
#3613 = DIRECTION ( 'NONE',  ( 0.9510565162951543083, 0.3090169943749450088, -0.000000000000000000 ) ) ;
#3614 = VERTEX_POINT ( 'NONE', #22382 ) ;
#3615 = CARTESIAN_POINT ( 'NONE',  ( -2.850469738011612186, 35.13561800352367470, -11.07553433454840608 ) ) ;
#3616 = DIRECTION ( 'NONE',  ( 0.000000000000000000, 0.000000000000000000, 1.000000000000000000 ) ) ;
#3617 = DIRECTION ( 'NONE',  ( 0.000000000000000000, 0.000000000000000000, 1.000000000000000000 ) ) ;
#3618 = EDGE_CURVE ( 'NONE', #29941, #18778, #13042, .T. ) ;
#3619 = CARTESIAN_POINT ( 'NONE',  ( 9.541469607472739867, 17.40487552589537401, 13.00000000000000178 ) ) ;
#3620 = CARTESIAN_POINT ( 'NONE',  ( 14.36830325120613594, 20.48707633493483371, 7.500000000000010658 ) ) ;
#3621 = LINE ( 'NONE', #16016, #879 ) ;
#3622 = CARTESIAN_POINT ( 'NONE',  ( 12.66562804284446919, 30.43173330721926462, -9.488869335771161317 ) ) ;
#3623 = ORIENTED_EDGE ( 'NONE', *, *, #31240, .F. ) ;
#3624 = CARTESIAN_POINT ( 'NONE',  ( -17.99203688690355207, 9.826896140120286560, -29.42929808537602554 ) ) ;
#3625 = CARTESIAN_POINT ( 'NONE',  ( -17.76739295965290211, 31.93461338995447107, 11.00000000000000000 ) ) ;
#3626 = CARTESIAN_POINT ( 'NONE',  ( 14.66907916930347255, -25.47038735071629034, -10.65037209538542662 ) ) ;
#3627 = PLANE ( 'NONE',  #17221 ) ;
#3628 = CARTESIAN_POINT ( 'NONE',  ( 14.99026664428914835, 26.05970091075412043, -9.233774695591788984 ) ) ;
#3629 = CARTESIAN_POINT ( 'NONE',  ( -17.81784622497958281, -13.85677843414106292, -19.80438750953545579 ) ) ;
#3630 = FACE_OUTER_BOUND ( 'NONE', #10587, .T. ) ;
#3631 = CARTESIAN_POINT ( 'NONE',  ( -14.12328112852335593, -14.97420427305475599, -28.52411008509453438 ) ) ;
#3632 = CARTESIAN_POINT ( 'NONE',  ( 6.600279139084632263, -21.58199846485096529, -19.93465999699473912 ) ) ;
#3633 = CARTESIAN_POINT ( 'NONE',  ( 11.14430626115242795, 17.35594636426317550, -28.08358351451018109 ) ) ;
#3634 = CARTESIAN_POINT ( 'NONE',  ( 30.37984583882173339, -21.95053059032868958, -7.980260795864960066 ) ) ;
#3635 = LINE ( 'NONE', #9939, #36136 ) ;
#3636 = DIRECTION ( 'NONE',  ( 1.000000000000000000, 0.000000000000000000, 0.000000000000000000 ) ) ;
#3637 = ORIENTED_EDGE ( 'NONE', *, *, #8355, .F. ) ;
#3638 = CARTESIAN_POINT ( 'NONE',  ( -9.111610322594222211, 34.24256388952155561, -8.919200168974919407 ) ) ;
#3639 = AXIS2_PLACEMENT_3D ( 'NONE', #25018, #13422, #37808 ) ;
#3640 = EDGE_CURVE ( 'NONE', #29758, #32296, #10003, .T. ) ;
#3641 = DIRECTION ( 'NONE',  ( -0.000000000000000000, -0.000000000000000000, -1.000000000000000000 ) ) ;
#3642 = AXIS2_PLACEMENT_3D ( 'NONE', #20643, #32636, #17602 ) ;
#3643 = CARTESIAN_POINT ( 'NONE',  ( 0.000000000000000000, 22.50000000000000355, 7.000000000000000000 ) ) ;
#3644 = ORIENTED_EDGE ( 'NONE', *, *, #7479, .T. ) ;
#3645 = CARTESIAN_POINT ( 'NONE',  ( 20.52762855279893373, 0.8436669142239806574, -28.70647179655530579 ) ) ;
#3646 = ADVANCED_FACE ( 'NONE', ( #16711 ), #33172, .T. ) ;
#3647 = CARTESIAN_POINT ( 'NONE',  ( -14.95151364724921628, 28.45442998384966415, -4.999999999999998224 ) ) ;
#3648 = VECTOR ( 'NONE', #29010, 1000.000000000000000 ) ;
#3649 = CARTESIAN_POINT ( 'NONE',  ( 13.13581098909226696, 27.45627467658428955, 7.000000000000000000 ) ) ;
#3650 = EDGE_LOOP ( 'NONE', ( #30966, #12947, #37821, #18333 ) ) ;
#3651 = CARTESIAN_POINT ( 'NONE',  ( -30.29894305497524698, 0.05251066091225892185, -8.298239616989643963 ) ) ;
#3652 = CARTESIAN_POINT ( 'NONE',  ( -18.07439750081194418, -24.11643431694279727, -13.20271803662888743 ) ) ;
#3653 = VERTEX_POINT ( 'NONE', #1879 ) ;
#3654 = CARTESIAN_POINT ( 'NONE',  ( 34.73099849614892065, -6.268898363069737911, -5.449674842175516787 ) ) ;
#3655 = ADVANCED_FACE ( 'NONE', ( #25839, #32145 ), #4309, .F. ) ;
#3656 = ORIENTED_EDGE ( 'NONE', *, *, #6896, .F. ) ;
#3657 = CARTESIAN_POINT ( 'NONE',  ( -12.20958131808417235, 35.40723086407943754, 13.32518128616661812 ) ) ;
#3658 = CARTESIAN_POINT ( 'NONE',  ( 10.73859285986296541, 31.49625607628530588, 7.499999999999996447 ) ) ;
#3659 = CARTESIAN_POINT ( 'NONE',  ( -4.817371740575545402, 23.83900317890010001, 23.00000000000000000 ) ) ;
#3660 = CARTESIAN_POINT ( 'NONE',  ( 6.761248272851016594, 33.72770196150386823, 18.87996532025785257 ) ) ;
#3661 = DIRECTION ( 'NONE',  ( -1.000000000000000000, 0.000000000000000000, 0.000000000000000000 ) ) ;
#3662 = ORIENTED_EDGE ( 'NONE', *, *, #3423, .T. ) ;
#3663 = FACE_OUTER_BOUND ( 'NONE', #34352, .T. ) ;
#3664 = CARTESIAN_POINT ( 'NONE',  ( 10.43479426945577693, 17.65763441714259940, -30.00000000000000711 ) ) ;
#3665 = DIRECTION ( 'NONE',  ( 1.000000000000000000, 0.000000000000000000, 0.000000000000000000 ) ) ;
#3666 = EDGE_CURVE ( 'NONE', #36832, #9748, #30594, .T. ) ;
#3667 = EDGE_CURVE ( 'NONE', #34816, #23702, #26244, .T. ) ;
#3668 = LINE ( 'NONE', #21750, #3299 ) ;
#3669 = ADVANCED_FACE ( 'NONE', ( #28891 ), #14255, .F. ) ;
#3670 = CARTESIAN_POINT ( 'NONE',  ( 13.75357712579410574, 15.21937127477098350, -29.39846290653906280 ) ) ;
#3671 = CARTESIAN_POINT ( 'NONE',  ( 5.439076474902442726, 21.17935537869283991, -24.39656225441747495 ) ) ;
#3672 = CIRCLE ( 'NONE', #12114, 1.000000000000008660 ) ;
#3673 = VERTEX_POINT ( 'NONE', #38440 ) ;
#3674 = CARTESIAN_POINT ( 'NONE',  ( 15.98625244049591743, -26.19102206502670072, -9.191584109855959639 ) ) ;
#3675 = CARTESIAN_POINT ( 'NONE',  ( 4.591666147298500533, 15.32946292166668556, 9.000000000000001776 ) ) ;
#3676 = ORIENTED_EDGE ( 'NONE', *, *, #9427, .T. ) ;
#3677 = CARTESIAN_POINT ( 'NONE',  ( -15.40280205795104074, 26.73783614089730420, -5.946216223248560695 ) ) ;
#3678 = CARTESIAN_POINT ( 'NONE',  ( -34.35058160602017097, -9.363338975649535101, 17.42190598798392998 ) ) ;
#3679 = CARTESIAN_POINT ( 'NONE',  ( 9.545480319410255987, -18.37756454525665362, -27.45318142481432844 ) ) ;
#3680 = CARTESIAN_POINT ( 'NONE',  ( 6.688300058587269170, 16.47782454277055564, 6.000000000000000000 ) ) ;
#3681 = ORIENTED_EDGE ( 'NONE', *, *, #6738, .T. ) ;
#3682 = ORIENTED_EDGE ( 'NONE', *, *, #11565, .T. ) ;
#3683 = CARTESIAN_POINT ( 'NONE',  ( -9.682888305682462615, 22.34984673401176991, -20.13486359021646521 ) ) ;
#3684 = CARTESIAN_POINT ( 'NONE',  ( -3.100643064501314328, 15.70406341247269211, 12.00000000000000000 ) ) ;
#3685 = ADVANCED_FACE ( 'NONE', ( #10611 ), #22992, .T. ) ;
#3686 = FACE_BOUND ( 'NONE', #15604, .T. ) ;
#3687 = CARTESIAN_POINT ( 'NONE',  ( -19.75415558344636580, -5.512529345569482153, -30.00000000000000711 ) ) ;
#3688 = CARTESIAN_POINT ( 'NONE',  ( -9.420974396635585890, -18.25674641473842286, -28.71086228043621347 ) ) ;
#3689 = CARTESIAN_POINT ( 'NONE',  ( 2.421689871081641687, 8.701977744317826335, 7.499999999999991118 ) ) ;
#3690 = ORIENTED_EDGE ( 'NONE', *, *, #16352, .F. ) ;
#3691 = CARTESIAN_POINT ( 'NONE',  ( 29.62904701965947396, 0.2356813439005103483, -9.712952148242360195 ) ) ;
#3692 = EDGE_CURVE ( 'NONE', #28502, #6243, #37076, .T. ) ;
#3693 = CARTESIAN_POINT ( 'NONE',  ( 0.000000000000000000, 22.50000000000000355, 7.000000000000000000 ) ) ;
#3694 = DIRECTION ( 'NONE',  ( 0.000000000000000000, 0.000000000000000000, 1.000000000000000000 ) ) ;
#3695 = ORIENTED_EDGE ( 'NONE', *, *, #16640, .T. ) ;
#3696 = CARTESIAN_POINT ( 'NONE',  ( -20.97191788603130647, 0.7853576264891806158, -26.22290328094025824 ) ) ;
#3697 = EDGE_LOOP ( 'NONE', ( #33973, #7904, #9994, #33355 ) ) ;
#3698 = CARTESIAN_POINT ( 'NONE',  ( 32.44839610264516239, -1.855716912065746182, -5.464228481487916511 ) ) ;
#3699 = CIRCLE ( 'NONE', #26403, 57.00000000000006395 ) ;
#3700 = VECTOR ( 'NONE', #36527, 1000.000000000000000 ) ;
#3701 = CARTESIAN_POINT ( 'NONE',  ( -11.54666566735214772, 32.07468077621344094, 7.000000000000000000 ) ) ;
#3702 = CARTESIAN_POINT ( 'NONE',  ( 18.91633830555523943, -27.33967421372791406, 16.30093088680201419 ) ) ;
#3703 = ORIENTED_EDGE ( 'NONE', *, *, #1825, .T. ) ;
#3704 = DIRECTION ( 'NONE',  ( -0.000000000000000000, -0.000000000000000000, -1.000000000000000000 ) ) ;
#3705 = CARTESIAN_POINT ( 'NONE',  ( -3.833852081710641624, 25.75497152300895820, 20.99999999999999645 ) ) ;
#3706 = AXIS2_PLACEMENT_3D ( 'NONE', #24506, #30616, #6601 ) ;
#3707 = DIRECTION ( 'NONE',  ( 0.9510565162951503115, -0.3090169943749574988, 0.000000000000000000 ) ) ;
#3708 = DIRECTION ( 'NONE',  ( 0.8090169943749426773, -0.5877852522924797984, -0.000000000000000000 ) ) ;
#3709 = CARTESIAN_POINT ( 'NONE',  ( 0.000000000000000000, 22.50000000000000355, 12.00000000000000000 ) ) ;
#3710 = CARTESIAN_POINT ( 'NONE',  ( 25.66376117785140565, 8.978964872295907895, 12.14047268033175797 ) ) ;
#3711 = CARTESIAN_POINT ( 'NONE',  ( -23.40191561818073396, 8.913894316990450761, -7.907414655062425801 ) ) ;
#3712 = CARTESIAN_POINT ( 'NONE',  ( 15.07134127176065164, -16.65659448856922609, -23.27637504703555038 ) ) ;
#3713 = LINE ( 'NONE', #673, #3397 ) ;
#3714 = CARTESIAN_POINT ( 'NONE',  ( 15.36998952511977912, 26.94570423236723755, -5.473408146588083056 ) ) ;
#3715 = CIRCLE ( 'NONE', #40028, 1.000000000000000000 ) ;
#3716 = ORIENTED_EDGE ( 'NONE', *, *, #31912, .F. ) ;
#3718 = VECTOR ( 'NONE', #2605, 1000.000000000000000 ) ;
#3717 = CARTESIAN_POINT ( 'NONE',  ( -12.82656864439730171, 18.37706610567507326, -21.77094397810654769 ) ) ;
#3719 = CARTESIAN_POINT ( 'NONE',  ( -27.41073561697751515, -13.75826678483051424, 20.69868183039780618 ) ) ;
#3720 = CARTESIAN_POINT ( 'NONE',  ( -14.64211604268330902, 20.79918788657763429, 6.000000000000000000 ) ) ;
#3721 = CARTESIAN_POINT ( 'NONE',  ( 11.14778535039169505, 17.59710828856957932, -26.83253580513521186 ) ) ;
#3722 = EDGE_LOOP ( 'NONE', ( #3530, #35691, #702, #21001, #24401 ) ) ;
#3723 = CARTESIAN_POINT ( 'NONE',  ( -0.2474735156158440752, 16.63111439559750693, 12.00000000000000000 ) ) ;
#3724 = ORIENTED_EDGE ( 'NONE', *, *, #3369, .T. ) ;
#3725 = AXIS2_PLACEMENT_3D ( 'NONE', #5165, #36255, #39287 ) ;
#3727 = CYLINDRICAL_SURFACE ( 'NONE', #28337, 0.5000000000000004441 ) ;
#3726 = CARTESIAN_POINT ( 'NONE',  ( -14.19928107862582323, 24.71232503731138763, -12.53013223596171244 ) ) ;
#3728 = CARTESIAN_POINT ( 'NONE',  ( -9.913802546424228979, -17.94660116923212456, -30.00000000000000000 ) ) ;
#3729 = FACE_OUTER_BOUND ( 'NONE', #38613, .T. ) ;
#3730 = AXIS2_PLACEMENT_3D ( 'NONE', #3545, #34433, #11005 ) ;
#3731 = ORIENTED_EDGE ( 'NONE', *, *, #16535, .T. ) ;
#3732 = CARTESIAN_POINT ( 'NONE',  ( -33.10183492075854161, -16.06006169670122929, -9.286424115536252799 ) ) ;
#3733 = CARTESIAN_POINT ( 'NONE',  ( -8.865215912320328684, -18.48469441140770542, -29.99999999999999645 ) ) ;
#3734 = CARTESIAN_POINT ( 'NONE',  ( -7.935776944912362296, 22.65328985282726393, 12.00000000000000000 ) ) ;
#3735 = CARTESIAN_POINT ( 'NONE',  ( 15.07825382683082971, 21.60216847466018208, -13.62695226071541121 ) ) ;
#3736 = VERTEX_POINT ( 'NONE', #36002 ) ;
#3737 = CARTESIAN_POINT ( 'NONE',  ( 23.00984832986303985, 5.371918940450665758, -16.81477143931289220 ) ) ;
#3738 = DIRECTION ( 'NONE',  ( 0.000000000000000000, 0.000000000000000000, 1.000000000000000000 ) ) ;
#3739 = FACE_OUTER_BOUND ( 'NONE', #16500, .T. ) ;
#3740 = CARTESIAN_POINT ( 'NONE',  ( -13.64211604268330724, 20.79918788657763429, 12.00000000000000000 ) ) ;
#3741 = EDGE_LOOP ( 'NONE', ( #14548, #10987 ) ) ;
#3742 = CARTESIAN_POINT ( 'NONE',  ( -31.14387024364657108, -0.3288088905222038560, -5.942067004542767705 ) ) ;
#3743 = CARTESIAN_POINT ( 'NONE',  ( 27.99670244976675804, -0.1511120543668041383, -13.47709887780296611 ) ) ;
#3744 = CARTESIAN_POINT ( 'NONE',  ( 16.60464863832688565, -22.41657912773190375, 19.66345542862528362 ) ) ;
#3745 = ORIENTED_EDGE ( 'NONE', *, *, #30869, .T. ) ;
#3746 = AXIS2_PLACEMENT_3D ( 'NONE', #38003, #7725, #1035 ) ;
#3747 = CARTESIAN_POINT ( 'NONE',  ( -15.72991998290134141, -16.18894361744923316, -30.00000000000001421 ) ) ;
#3748 = DIRECTION ( 'NONE',  ( 1.000000000000000000, 0.000000000000000000, 0.000000000000000000 ) ) ;
#3749 = CIRCLE ( 'NONE', #11542, 0.5000000000000004441 ) ;
#3750 = AXIS2_PLACEMENT_3D ( 'NONE', #2561, #27138, #20450 ) ;
#3751 = VERTEX_POINT ( 'NONE', #7554 ) ;
#3752 = DIRECTION ( 'NONE',  ( 0.000000000000000000, 0.000000000000000000, -1.000000000000000000 ) ) ;
#3753 = CIRCLE ( 'NONE', #1839, 1.000000000000000000 ) ;
#3754 = DIRECTION ( 'NONE',  ( 0.6691306063588670083, 0.7431448254773862505, -0.000000000000000000 ) ) ;
#3755 = CYLINDRICAL_SURFACE ( 'NONE', #35944, 1.000000000000000888 ) ;
#3756 = CARTESIAN_POINT ( 'NONE',  ( 6.063463481279891987, 37.09571784679343409, -6.711698804117649075 ) ) ;
#3757 = CARTESIAN_POINT ( 'NONE',  ( 14.73239529508889767, 21.45431699865973840, 10.94611345180490503 ) ) ;
#3758 = EDGE_CURVE ( 'NONE', #35978, #17743, #14367, .T. ) ;
#3759 = ORIENTED_EDGE ( 'NONE', *, *, #15975, .T. ) ;
#3760 = CARTESIAN_POINT ( 'NONE',  ( 14.40879062396295041, 19.98622263052302017, 10.49999999999999822 ) ) ;
#3761 = CARTESIAN_POINT ( 'NONE',  ( -5.724378136954611840, 12.76962061027129458, 13.00000000000000178 ) ) ;
#3762 = CARTESIAN_POINT ( 'NONE',  ( 25.46646149454646491, -19.62346392400056772, -13.83418298888276965 ) ) ;
#3763 = DIRECTION ( 'NONE',  ( -0.000000000000000000, -0.000000000000000000, -1.000000000000000000 ) ) ;
#3764 = DIRECTION ( 'NONE',  ( 0.000000000000000000, 0.000000000000000000, 1.000000000000000000 ) ) ;
#3765 = CARTESIAN_POINT ( 'NONE',  ( 9.806975420853749625, 31.15003855377755571, 12.00000000000000000 ) ) ;
#3766 = CARTESIAN_POINT ( 'NONE',  ( 15.16389459841380116, 27.51912694620480337, -5.938229366125038489 ) ) ;
#3767 = DIRECTION ( 'NONE',  ( -0.8090169943749505599, -0.5877852522924689183, 0.000000000000000000 ) ) ;
#3768 = ORIENTED_EDGE ( 'NONE', *, *, #11787, .T. ) ;
#3770 = LINE ( 'NONE', #22453, #25243 ) ;
#3769 = CARTESIAN_POINT ( 'NONE',  ( -17.11581301909970421, 15.65337108435191027, -16.89279340584462119 ) ) ;
#3771 = EDGE_CURVE ( 'NONE', #10321, #2610, #32557, .T. ) ;
#3772 = CARTESIAN_POINT ( 'NONE',  ( 12.80736835487433112, 15.68301270189216545, 11.00000000000000000 ) ) ;
#3773 = CARTESIAN_POINT ( 'NONE',  ( 15.21573614595498647, -26.38579844286377707, -7.827967313425957308 ) ) ;
#3774 = ADVANCED_FACE ( 'NONE', ( #26445 ), #32353, .T. ) ;
#3775 = DIRECTION ( 'NONE',  ( -0.000000000000000000, -0.000000000000000000, -1.000000000000000000 ) ) ;
#3776 = CARTESIAN_POINT ( 'NONE',  ( 14.03396390992467779, 23.92513025192832998, -13.51357501533718697 ) ) ;
#3777 = ORIENTED_EDGE ( 'NONE', *, *, #13619, .F. ) ;
#3778 = CARTESIAN_POINT ( 'NONE',  ( 15.41110799979362511, 26.80090896191098793, -5.474125546455649527 ) ) ;
#3779 = VERTEX_POINT ( 'NONE', #1468 ) ;
#3780 = CARTESIAN_POINT ( 'NONE',  ( 7.312035131040564906, 19.41226734497195849, 13.00000000000000178 ) ) ;
#3781 = CARTESIAN_POINT ( 'NONE',  ( -11.10104332229198221, -20.48357726655720157, -20.55124491515338647 ) ) ;
#3782 = CARTESIAN_POINT ( 'NONE',  ( -36.34524575547219882, -5.221887369237684595, 12.73282698324894824 ) ) ;
#3783 = AXIS2_PLACEMENT_3D ( 'NONE', #559, #31831, #13137 ) ;
#3784 = CARTESIAN_POINT ( 'NONE',  ( -17.73645540159148482, -13.01725682536783424, -24.25077156562453240 ) ) ;
#3785 = CARTESIAN_POINT ( 'NONE',  ( -1.783775571689018902, -20.56493600434025026, -27.73431482934296355 ) ) ;
#3786 = CARTESIAN_POINT ( 'NONE',  ( 15.75662360411219787, 25.59993261007102561, -5.474038466411062842 ) ) ;
#3787 = ORIENTED_EDGE ( 'NONE', *, *, #1941, .T. ) ;
#3788 = CARTESIAN_POINT ( 'NONE',  ( 21.98254353505891601, 9.874900589700915887, -11.87314829681821138 ) ) ;
#3789 = DIRECTION ( 'NONE',  ( -0.000000000000000000, -0.000000000000000000, -1.000000000000000000 ) ) ;
#3790 = CARTESIAN_POINT ( 'NONE',  ( 3.366772934462163747, 37.76190412503621729, 16.87380292611444688 ) ) ;
#3791 = AXIS2_PLACEMENT_3D ( 'NONE', #4563, #25886, #7397 ) ;
#3792 = ORIENTED_EDGE ( 'NONE', *, *, #23020, .T. ) ;
#3793 = CARTESIAN_POINT ( 'NONE',  ( -25.68856216064254383, -2.472509833716490579, -18.10827930001592634 ) ) ;
#3794 = CIRCLE ( 'NONE', #15488, 6.000000000000003553 ) ;
#3795 = CARTESIAN_POINT ( 'NONE',  ( -11.83264664767723318, 25.78892025137227151, 19.27171037444156809 ) ) ;
#3796 = ORIENTED_EDGE ( 'NONE', *, *, #12269, .F. ) ;
#3797 = DIRECTION ( 'NONE',  ( 0.8660254037844364872, -0.5000000000000038858, 0.000000000000000000 ) ) ;
#3798 = ADVANCED_FACE ( 'NONE', ( #20160 ), #4716, .F. ) ;
#3799 = FACE_BOUND ( 'NONE', #26332, .T. ) ;
#3800 = EDGE_CURVE ( 'NONE', #11948, #35485, #26012, .T. ) ;
#3801 = CARTESIAN_POINT ( 'NONE',  ( -27.13564390634777368, 1.007537100714265277, -13.55923196749210291 ) ) ;
#3802 = CARTESIAN_POINT ( 'NONE',  ( 34.02878622761630822, -14.89681383196699294, -8.416776523781875241 ) ) ;
#3803 = CARTESIAN_POINT ( 'NONE',  ( 34.83525826321752561, -1.648928274806286565, 11.55979286843933984 ) ) ;
#3804 = ORIENTED_EDGE ( 'NONE', *, *, #21784, .F. ) ;
#3805 = ORIENTED_EDGE ( 'NONE', *, *, #28700, .T. ) ;
#3806 = CARTESIAN_POINT ( 'NONE',  ( 7.929471891321336230, 25.60217271033461373, 9.000000000000001776 ) ) ;
#3807 = CARTESIAN_POINT ( 'NONE',  ( -16.42808373348810846, 23.48417063542603955, -5.000000000000001776 ) ) ;
#3808 = CIRCLE ( 'NONE', #18724, 0.9999999999999974465 ) ;
#3809 = VECTOR ( 'NONE', #7940, 1000.000000000000000 ) ;
#3810 = CARTESIAN_POINT ( 'NONE',  ( -13.94482798346716201, 26.50521816028930999, 11.00000000000000000 ) ) ;
#3811 = VERTEX_POINT ( 'NONE', #35798 ) ;
#3812 = CARTESIAN_POINT ( 'NONE',  ( -0.7453837511599995524, 37.93422878730011405, -7.543976147524814380 ) ) ;
#3813 = DIRECTION ( 'NONE',  ( 1.000000000000000000, 0.000000000000000000, 0.000000000000000000 ) ) ;
#3814 = DIRECTION ( 'NONE',  ( -0.7431448254773953543, -0.6691306063588570163, -0.000000000000000000 ) ) ;
#3815 = CIRCLE ( 'NONE', #29141, 0.5000000000000004441 ) ;
#3816 = LINE ( 'NONE', #10930, #2036 ) ;
#3818 = EDGE_CURVE ( 'NONE', #25818, #342, #29272, .T. ) ;
#3817 = CARTESIAN_POINT ( 'NONE',  ( -8.927394655428429360, 11.06314620770957013, 11.00000000000000000 ) ) ;
#3819 = CARTESIAN_POINT ( 'NONE',  ( -10.77256156952734223, 32.87247436945333590, 10.76099332938164288 ) ) ;
#3820 = CARTESIAN_POINT ( 'NONE',  ( 9.818323868757666162, 23.26050863160002535, -19.07506069204259092 ) ) ;
#3821 = DIRECTION ( 'NONE',  ( 0.000000000000000000, 0.000000000000000000, 1.000000000000000000 ) ) ;
#3822 = ORIENTED_EDGE ( 'NONE', *, *, #10861, .F. ) ;
#3824 = PLANE ( 'NONE',  #11599 ) ;
#3823 = CARTESIAN_POINT ( 'NONE',  ( -18.05228600792142046, 10.74605824565360201, -24.41647870628840877 ) ) ;
#3825 = FACE_OUTER_BOUND ( 'NONE', #8701, .T. ) ;
#3826 = CARTESIAN_POINT ( 'NONE',  ( 9.863624987970052160, -18.52888242359477289, -26.21732557761542282 ) ) ;
#3827 = EDGE_CURVE ( 'NONE', #7027, #7392, #4915, .T. ) ;
#3828 = CARTESIAN_POINT ( 'NONE',  ( 9.331903152615748098, 11.35703883385568780, 7.000000000000000000 ) ) ;
#3829 = CARTESIAN_POINT ( 'NONE',  ( 14.99499369208347233, 26.04445448530989182, -9.234529751571013634 ) ) ;
#3830 = CARTESIAN_POINT ( 'NONE',  ( -7.289639608743041066, -27.06962010326280321, -5.000000000000000000 ) ) ;
#3831 = DIRECTION ( 'NONE',  ( 1.000000000000000000, 0.000000000000000000, 0.000000000000000000 ) ) ;
#3832 = CARTESIAN_POINT ( 'NONE',  ( -25.99994897708846864, -25.85974776871800884, -5.874774900483986428 ) ) ;
#3833 = CARTESIAN_POINT ( 'NONE',  ( 6.264040290701674785, -20.94110484306758124, -22.06492468031074239 ) ) ;
#3834 = CARTESIAN_POINT ( 'NONE',  ( 13.01827371381056864, 21.50808331926381101, -17.45255298520018172 ) ) ;
#3835 = CARTESIAN_POINT ( 'NONE',  ( 31.44183620580527716, -21.28341506558783180, -7.121041165608909651 ) ) ;
#3836 = DIRECTION ( 'NONE',  ( -0.000000000000000000, -0.000000000000000000, -1.000000000000000000 ) ) ;
#3837 = CARTESIAN_POINT ( 'NONE',  ( -36.90323640188874066, -1.335463057344152604, 10.99999999999999822 ) ) ;
#3838 = EDGE_LOOP ( 'NONE', ( #19364, #23269 ) ) ;
#3839 = CARTESIAN_POINT ( 'NONE',  ( -6.015615027858057573, 25.61324666952316420, -18.76221355029760929 ) ) ;
#3840 = AXIS2_PLACEMENT_3D ( 'NONE', #1687, #19213, #38098 ) ;
#3841 = CIRCLE ( 'NONE', #29781, 1.000000000000000000 ) ;
#3842 = CARTESIAN_POINT ( 'NONE',  ( 5.440829913680675034, 10.60893893836775348, 12.00000000000000000 ) ) ;
#3843 = VERTEX_POINT ( 'NONE', #31934 ) ;
#3844 = CARTESIAN_POINT ( 'NONE',  ( 30.73988743330639295, -0.04538756457274935319, -6.887853167781535113 ) ) ;
#3845 = CARTESIAN_POINT ( 'NONE',  ( -6.557822374958138134, 35.99981354310120452, 10.49999999999999822 ) ) ;
#3846 = EDGE_CURVE ( 'NONE', #9898, #22045, #4103, .T. ) ;
#3847 = CARTESIAN_POINT ( 'NONE',  ( -32.33143948541797386, 1.358872982501903248, 11.00000000000000000 ) ) ;
#3848 = ADVANCED_FACE ( 'NONE', ( #12207 ), #24601, .T. ) ;
#3849 = AXIS2_PLACEMENT_3D ( 'NONE', #32304, #31893, #25591 ) ;
#3850 = B_SPLINE_SURFACE_WITH_KNOTS ( 'NONE', 3, 3, ( 
 ( #8903, #24540, #12344, #36532, #34087, #33503, #30644 ),
 ( #33300, #39575, #11951, #39772, #2609, #36936, #11751 ),
 ( #39971, #5645, #18055, #30447, #2803, #15196, #12150 ),
 ( #27586, #9101, #24732, #24135, #21095, #37132, #21488 ),
 ( #17860, #27188, #23939, #14995, #24340, #36738, #30241 ),
 ( #33893, #6046, #6245, #14600, #21295, #15395, #18450 ),
 ( #33700, #5851, #18253, #30839, #9304, #27788, #40172 ),
 ( #21687, #30038, #2213, #26988, #36337, #39376, #11554 ),
 ( #8500, #2410, #14801, #25329, #6832, #31232, #19234 ),
 ( #34485, #22476, #35081, #6631, #31042, #37925, #28782 ),
 ( #37729, #9706, #10097, #25132, #28376, #18649, #27981 ),
 ( #9503, #556, #13132, #153, #22678, #19041, #31432 ),
 ( #37531, #15790, #25729, #28181, #7036, #34681, #22085 ),
 ( #10297, #3599, #21880, #15594, #13335, #34883, #358 ),
 ( #3993, #15995, #19434, #12938, #16195, #9896, #12545 ),
 ( #22276, #31827, #12737, #6440, #31628, #16394, #3795 ),
 ( #28579, #753, #38123, #25525, #958, #3207, #24936 ),
 ( #37329, #34287, #18845, #3396, #16805, #29385, #17006 ),
 ( #1765, #29189, #7235, #17212, #23088, #35488, #7648 ),
 ( #20253, #29587, #10912, #7846, #14149, #29793, #1357 ),
 ( #1975, #32651, #39129, #22878, #4400, #1159, #38527 ),
 ( #7441, #5005, #38934, #26547, #23696, #32031, #20051 ),
 ( #11109, #1561, #13945, #10702, #26130, #4605, #14352 ),
 ( #17418, #35690, #19635, #26339, #4199, #4807, #32446 ),
 ( #38733, #38327, #23493, #23297, #35283, #20458, #35889 ) ),
 .UNSPECIFIED., .F., .F., .F.,
 ( 4, 3, 3, 3, 3, 3, 3, 3, 4 ),
 ( 4, 3, 4 ),
 ( 0.000000000000000000, 0.1250000000000000000, 0.2500000000000000000, 0.3750000000000000000, 0.5000000000000000000, 0.6250000000000000000, 0.7500000000000000000, 0.8750000000000000000, 1.000000000000000000 ),
 ( 5.507097317918141499, 5.759586531581287971, 6.012075745244433556 ),
 .UNSPECIFIED. ) ;
#3851 = ORIENTED_EDGE ( 'NONE', *, *, #18911, .T. ) ;
#3852 = CARTESIAN_POINT ( 'NONE',  ( -20.52497589132623546, 0.8981380531211777818, -28.70837990097334114 ) ) ;
#3853 = CARTESIAN_POINT ( 'NONE',  ( 34.47241746879583957, 3.460351812918713854, 0.000000000000000000 ) ) ;
#3854 = ORIENTED_EDGE ( 'NONE', *, *, #25042, .F. ) ;
#3855 = CARTESIAN_POINT ( 'NONE',  ( 22.67047725821499427, -5.391315940321618427, -22.09846031373282926 ) ) ;
#3856 = VERTEX_POINT ( 'NONE', #17919 ) ;
#3857 = APPLICATION_PROTOCOL_DEFINITION ( 'draft international standard', 'automotive_design', 1998, #15056 ) ;
#3858 = CARTESIAN_POINT ( 'NONE',  ( -15.98961535660690636, 30.99268274074326257, 10.99999999999966249 ) ) ;
#3859 = CARTESIAN_POINT ( 'NONE',  ( 0.6056960332696259552, 17.55816537872232530, 12.00000000000000000 ) ) ;
#3860 = DIRECTION ( 'NONE',  ( 1.000000000000000000, 1.224646799147353947E-16, 0.000000000000000000 ) ) ;
#3861 = CARTESIAN_POINT ( 'NONE',  ( -5.983876423895868157, 32.43697950591384682, 19.66345542862462281 ) ) ;
#3862 = DIRECTION ( 'NONE',  ( 1.000000000000000000, 0.000000000000000000, 0.000000000000000000 ) ) ;
#3863 = ORIENTED_EDGE ( 'NONE', *, *, #1692, .T. ) ;
#3864 = DIRECTION ( 'NONE',  ( -1.000000000000000000, 0.000000000000000000, 0.000000000000000000 ) ) ;
#3865 = DIRECTION ( 'NONE',  ( -0.5000000000000041078, -0.8660254037844362651, 0.000000000000000000 ) ) ;
#3866 = CYLINDRICAL_SURFACE ( 'NONE', #31832, 0.5000000000000004441 ) ;
#3867 = EDGE_CURVE ( 'NONE', #4036, #31246, #36203, .T. ) ;
#3868 = CARTESIAN_POINT ( 'NONE',  ( 14.42591706986332944, 14.96404800320749473, -26.50133422042014786 ) ) ;
#3870 = AXIS2_PLACEMENT_3D ( 'NONE', #10063, #3367, #34258 ) ;
#3869 = CARTESIAN_POINT ( 'NONE',  ( 10.00952708242434319, 34.92643930758972459, -5.878487041382220113 ) ) ;
#3871 = ORIENTED_EDGE ( 'NONE', *, *, #26288, .T. ) ;
#3872 = CARTESIAN_POINT ( 'NONE',  ( 15.61960274502122736, -25.98614172846138004, -9.670060679591365727 ) ) ;
#3873 = DIRECTION ( 'NONE',  ( 1.000000000000000000, 0.000000000000000000, 0.000000000000000000 ) ) ;
#3874 = CIRCLE ( 'NONE', #15565, 1.000000000000000888 ) ;
#3875 = CARTESIAN_POINT ( 'NONE',  ( -9.917741276437942233, 30.52956727630665057, 13.00000000000000178 ) ) ;
#3876 = ORIENTED_EDGE ( 'NONE', *, *, #6864, .T. ) ;
#3877 = CARTESIAN_POINT ( 'NONE',  ( -15.23583419380056014, 26.39386630455032545, -7.828192486749263601 ) ) ;
#3878 = CARTESIAN_POINT ( 'NONE',  ( -34.49513285232489324, -12.61775564956212570, 17.42190598798391576 ) ) ;
#3879 = CARTESIAN_POINT ( 'NONE',  ( 13.81758775394617444, -24.97846941233739670, -11.61434847950435234 ) ) ;
#3880 = CARTESIAN_POINT ( 'NONE',  ( 3.992867117591230919, 8.524771480177550487, 10.49999999999999822 ) ) ;
#3881 = VERTEX_POINT ( 'NONE', #2076 ) ;
#3882 = ORIENTED_EDGE ( 'NONE', *, *, #16004, .F. ) ;
#3883 = CARTESIAN_POINT ( 'NONE',  ( -11.26877388990210704, 26.23917836842477769, -15.09852949179583348 ) ) ;
#3884 = CARTESIAN_POINT ( 'NONE',  ( -15.01668848176030480, -20.19012063094625020, -19.09890700315882128 ) ) ;
#3885 = FACE_BOUND ( 'NONE', #13805, .T. ) ;
#3886 = CARTESIAN_POINT ( 'NONE',  ( -30.95311370318828281, -7.619573582569746151, -13.02312855672049707 ) ) ;
#3887 = DIRECTION ( 'NONE',  ( 1.000000000000000000, 0.000000000000000000, 0.000000000000000000 ) ) ;
#3888 = ORIENTED_EDGE ( 'NONE', *, *, #8164, .T. ) ;
#3889 = CARTESIAN_POINT ( 'NONE',  ( 30.81169820973430973, 0.05224243800113870240, -4.999999999999999112 ) ) ;
#3890 = LINE ( 'NONE', #38226, #27801 ) ;
#3891 = DIRECTION ( 'NONE',  ( 0.9945218953682730678, -0.1045284632676564962, 0.000000000000000000 ) ) ;
#3892 = ORIENTED_EDGE ( 'NONE', *, *, #18834, .F. ) ;
#3893 = CARTESIAN_POINT ( 'NONE',  ( -23.94792893277753265, 0.4690917673518810727, -19.49405232091567441 ) ) ;
#3894 = B_SPLINE_CURVE_WITH_KNOTS ( 'NONE', 3,
 ( #26383, #17863, #30244, #4850, #7698, #14804 ),
 .UNSPECIFIED., .F., .F.,
 ( 4, 2, 4 ),
 ( 0.000000000000000000, 0.5000000000000000000, 1.000000000000000000 ),
 .UNSPECIFIED. ) ;
#3895 = CARTESIAN_POINT ( 'NONE',  ( -32.93563651212921428, -26.12966208807736379, 11.00000000000000533 ) ) ;
#3897 = ADVANCED_FACE ( 'NONE', ( #14861 ), #21152, .F. ) ;
#3896 = EDGE_LOOP ( 'NONE', ( #11240, #32138, #1348, #19088, #151 ) ) ;
#3898 = CARTESIAN_POINT ( 'NONE',  ( 24.84710857777880832, -2.152420164953839254, -19.17158435834083718 ) ) ;
#3899 = CARTESIAN_POINT ( 'NONE',  ( 13.71288650290049560, 15.24265236820024683, -30.00000000000001066 ) ) ;
#3900 = CARTESIAN_POINT ( 'NONE',  ( 34.64551053920951063, -5.829853277351126017, 16.30093088680154167 ) ) ;
#3901 = ORIENTED_EDGE ( 'NONE', *, *, #36880, .T. ) ;
#3902 = CARTESIAN_POINT ( 'NONE',  ( 16.24129362380267239, 27.01431713449539629, 15.13084544680213561 ) ) ;
#3903 = VECTOR ( 'NONE', #16356, 1000.000000000000000 ) ;
#3904 = CARTESIAN_POINT ( 'NONE',  ( -18.71275814301062823, -29.33771053242124793, -4.999999999999998224 ) ) ;
#3905 = CARTESIAN_POINT ( 'NONE',  ( -3.503066876656364403, 27.10955750621961258, 20.99999999999998934 ) ) ;
#3906 = CARTESIAN_POINT ( 'NONE',  ( 8.472151273871505239, 28.78272654129060371, 11.00000000000000000 ) ) ;
#3907 = FACE_OUTER_BOUND ( 'NONE', #11561, .T. ) ;
#3908 = EDGE_CURVE ( 'NONE', #5670, #38309, #5312, .T. ) ;
#3909 = AXIS2_PLACEMENT_3D ( 'NONE', #38539, #28793, #10712 ) ;
#3910 = FACE_BOUND ( 'NONE', #38784, .T. ) ;
#3911 = EDGE_CURVE ( 'NONE', #31137, #20501, #8967, .T. ) ;
#3912 = CARTESIAN_POINT ( 'NONE',  ( 22.19961376577536072, 12.81695298357553270, 15.13084544680213561 ) ) ;
#3913 = CARTESIAN_POINT ( 'NONE',  ( -21.66698873614936360, 9.458035595798465422, -13.88965424940386839 ) ) ;
#3914 = CARTESIAN_POINT ( 'NONE',  ( 22.01692992093476775, -27.08823313053303750, -5.000000000000004441 ) ) ;
#3915 = DIRECTION ( 'NONE',  ( -0.4067366430757888840, 0.9135454576426058626, 0.000000000000000000 ) ) ;
#3916 = ORIENTED_EDGE ( 'NONE', *, *, #29266, .F. ) ;
#3917 = CARTESIAN_POINT ( 'NONE',  ( 12.57305715050316408, 21.17289748902732072, -18.43455663015607016 ) ) ;
#3918 = VERTEX_POINT ( 'NONE', #17723 ) ;
#3919 = CARTESIAN_POINT ( 'NONE',  ( -15.30439135265882378, 25.08127062006494157, -9.249767499845980012 ) ) ;
#3920 = ADVANCED_FACE ( 'NONE', ( #18119 ), #2668, .T. ) ;
#3921 = CARTESIAN_POINT ( 'NONE',  ( -28.51362642450540719, -10.10416295265245878, 20.50957957746029336 ) ) ;
#3922 = DIRECTION ( 'NONE',  ( 0.000000000000000000, 0.000000000000000000, 1.000000000000000000 ) ) ;
#3923 = CARTESIAN_POINT ( 'NONE',  ( 11.51364707597612380, 18.41203290593636410, -23.85841619709769645 ) ) ;
#3924 = ORIENTED_EDGE ( 'NONE', *, *, #14241, .F. ) ;
#3925 = CARTESIAN_POINT ( 'NONE',  ( 28.86970498031842780, -14.78348567515910794, -13.80807807713542879 ) ) ;
#3926 = DIRECTION ( 'NONE',  ( 0.7032331762534107522, 0.07391278520356026061, -0.7071067811865416886 ) ) ;
#3927 = VECTOR ( 'NONE', #8213, 1000.000000000000114 ) ;
#3928 = EDGE_LOOP ( 'NONE', ( #39432, #12397, #6346 ) ) ;
#3930 = LINE ( 'NONE', #4333, #23159 ) ;
#3929 = CARTESIAN_POINT ( 'NONE',  ( -13.02858025086399785, 22.56370760927372032, -16.40322947727175062 ) ) ;
#3931 = CARTESIAN_POINT ( 'NONE',  ( -15.94649114141366830, -25.87861724480484327, -10.11375243002179936 ) ) ;
#3932 = DIRECTION ( 'NONE',  ( 1.000000000000000000, 0.000000000000000000, 0.000000000000000000 ) ) ;
#3933 = EDGE_LOOP ( 'NONE', ( #26449, #21740, #1211, #26684, #33240 ) ) ;
#3934 = CARTESIAN_POINT ( 'NONE',  ( -18.43967439804336550, -8.978407292334223300, -29.21425099581027851 ) ) ;
#3935 = CARTESIAN_POINT ( 'NONE',  ( -9.285084774773752159, -18.78246842825664942, -26.27069818453050587 ) ) ;
#3936 = DIRECTION ( 'NONE',  ( 0.4067366430758009299, 0.9135454576426005335, 0.000000000000000000 ) ) ;
#3937 = CARTESIAN_POINT ( 'NONE',  ( 15.52188586741623944, 21.55406148401431210, -12.66412526168250530 ) ) ;
#3938 = EDGE_LOOP ( 'NONE', ( #7219, #21347, #12485, #33491, #39613 ) ) ;
#3939 = CARTESIAN_POINT ( 'NONE',  ( 27.41035584056263374, 3.779750892310774990, -5.951374944377225695 ) ) ;
#3940 = PLANE ( 'NONE',  #31686 ) ;
#3941 = CARTESIAN_POINT ( 'NONE',  ( 12.30736835487432934, 14.81698729810772797, 11.00000000000000000 ) ) ;
#3942 = ORIENTED_EDGE ( 'NONE', *, *, #9008, .T. ) ;
#3943 = EDGE_CURVE ( 'NONE', #26001, #17093, #5260, .T. ) ;
#3944 = CARTESIAN_POINT ( 'NONE',  ( -29.20369560020293065, -0.2713287649291702963, -11.56506784693800327 ) ) ;
#3945 = EDGE_CURVE ( 'NONE', #18383, #7720, #16959, .T. ) ;
#3946 = CARTESIAN_POINT ( 'NONE',  ( 31.24124332302707785, -0.3963250197696455146, -5.471922067842784010 ) ) ;
#3947 = CARTESIAN_POINT ( 'NONE',  ( 28.61121519738619767, -15.27903652329876394, 20.25080042701566541 ) ) ;
#3948 = CIRCLE ( 'NONE', #19520, 1.000000000000000444 ) ;
#3949 = EDGE_LOOP ( 'NONE', ( #4698, #19522, #26894, #1254 ) ) ;
#3950 = CARTESIAN_POINT ( 'NONE',  ( -11.41987377193683528, -19.41918266173334828, -30.00000000000000000 ) ) ;
#3951 = CARTESIAN_POINT ( 'NONE',  ( 18.23649648353767461, -16.09146789626181118, 23.00000000000000000 ) ) ;
#3952 = ORIENTED_EDGE ( 'NONE', *, *, #2916, .T. ) ;
#3953 = CARTESIAN_POINT ( 'NONE',  ( -7.468455364333119739, 29.89744377950679421, 10.50000000000000000 ) ) ;
#3954 = EDGE_CURVE ( 'NONE', #17593, #20190, #12008, .T. ) ;
#3955 = DIRECTION ( 'NONE',  ( 1.000000000000000000, 0.000000000000000000, 0.000000000000000000 ) ) ;
#3956 = DIRECTION ( 'NONE',  ( 0.000000000000000000, 0.000000000000000000, 1.000000000000000000 ) ) ;
#3957 = ADVANCED_FACE ( 'NONE', ( #8764, #5908 ), #5709, .T. ) ;
#3958 = LINE ( 'NONE', #3173, #22390 ) ;
#3959 = ORIENTED_EDGE ( 'NONE', *, *, #15015, .F. ) ;
#3960 = DIRECTION ( 'NONE',  ( -0.000000000000000000, -0.000000000000000000, -1.000000000000000000 ) ) ;
#3961 = LINE ( 'NONE', #28745, #23974 ) ;
#3962 = CARTESIAN_POINT ( 'NONE',  ( 26.39312466668815560, -24.39732993984534914, -8.895862594080151453 ) ) ;
#3963 = CARTESIAN_POINT ( 'NONE',  ( 9.806975420853749625, 31.15003855377755571, 13.00000000000000178 ) ) ;
#3964 = DIRECTION ( 'NONE',  ( 0.6691306063588570163, -0.7431448254773953543, 0.000000000000000000 ) ) ;
#3965 = CARTESIAN_POINT ( 'NONE',  ( 14.82073388239109768, 26.57690641049478586, -9.208629837656934214 ) ) ;
#3966 = DIRECTION ( 'NONE',  ( 1.000000000000000000, 0.000000000000000000, 0.000000000000000000 ) ) ;
#3967 = VERTEX_POINT ( 'NONE', #30098 ) ;
#3968 = CIRCLE ( 'NONE', #4647, 1.000000000000000000 ) ;
#3970 = CARTESIAN_POINT ( 'NONE',  ( 3.712277862705659182, 32.06720926237454705, 10.74999999999998757 ) ) ;
#3969 = CARTESIAN_POINT ( 'NONE',  ( -17.81838900191993247, 19.71268737054005982, -5.955960509222737009 ) ) ;
#3971 = CARTESIAN_POINT ( 'NONE',  ( 13.13451774850152809, 16.06441397984643871, 10.49999999999999822 ) ) ;
#3972 = AXIS2_PLACEMENT_3D ( 'NONE', #5505, #20766, #39635 ) ;
#3973 = CARTESIAN_POINT ( 'NONE',  ( 15.39214080485340475, -26.69224274047939360, -5.946089343969266139 ) ) ;
#3974 = FACE_OUTER_BOUND ( 'NONE', #3490, .T. ) ;
#3975 = CARTESIAN_POINT ( 'NONE',  ( 11.48395950158329804, 18.43760140489433041, -23.85392656665083777 ) ) ;
#3976 = VERTEX_POINT ( 'NONE', #2273 ) ;
#3977 = CARTESIAN_POINT ( 'NONE',  ( 11.88635790708222295, 19.38841407910786785, -21.61592131405399542 ) ) ;
#3978 = VERTEX_POINT ( 'NONE', #30506 ) ;
#3980 = DIRECTION ( 'NONE',  ( 0.000000000000000000, 0.000000000000000000, -1.000000000000000000 ) ) ;
#3979 = CARTESIAN_POINT ( 'NONE',  ( -15.36654411751621119, 26.86631301760015234, -5.944861291199306841 ) ) ;
#3981 = CARTESIAN_POINT ( 'NONE',  ( -15.41413216001110165, -26.64907402180547891, -6.417196768553821151 ) ) ;
#3982 = CARTESIAN_POINT ( 'NONE',  ( -34.66558941538325200, -1.755063786819271554, 12.73282698324811513 ) ) ;
#3983 = CARTESIAN_POINT ( 'NONE',  ( -30.13941039663480126, -22.19442074003340792, -7.981896383023998176 ) ) ;
#3984 = CARTESIAN_POINT ( 'NONE',  ( -3.346448692850797713, -20.50037512799487160, -26.59278566100418928 ) ) ;
#3985 = CARTESIAN_POINT ( 'NONE',  ( 15.28834851042550547, 25.12984405973253388, -9.249120326217479260 ) ) ;
#3986 = VERTEX_POINT ( 'NONE', #20955 ) ;
#3987 = CARTESIAN_POINT ( 'NONE',  ( 19.09019219243798560, 9.727682261722398138, -22.24254973901808796 ) ) ;
#3988 = CARTESIAN_POINT ( 'NONE',  ( -19.26948696230207858, 27.85601271560029701, 11.00000000000000000 ) ) ;
#3989 = VECTOR ( 'NONE', #39816, 1000.000000000000000 ) ;
#3990 = CARTESIAN_POINT ( 'NONE',  ( 14.43694901005322961, 26.51279404187409838, 17.42190598798392642 ) ) ;
#3991 = ORIENTED_EDGE ( 'NONE', *, *, #4938, .T. ) ;
#3992 = CARTESIAN_POINT ( 'NONE',  ( -33.95211651047912937, -4.501248717685172984, -5.902678725086724754 ) ) ;
#3993 = CARTESIAN_POINT ( 'NONE',  ( -28.78471548568728977, -2.122417091760708807, 18.87996532025784902 ) ) ;
#3994 = ORIENTED_EDGE ( 'NONE', *, *, #10162, .T. ) ;
#3995 = FACE_OUTER_BOUND ( 'NONE', #16900, .T. ) ;
#3996 = DIRECTION ( 'NONE',  ( 0.000000000000000000, 0.000000000000000000, 1.000000000000000000 ) ) ;
#3997 = EDGE_CURVE ( 'NONE', #4159, #34227, #38164, .T. ) ;
#3998 = CARTESIAN_POINT ( 'NONE',  ( 18.84397998463681034, -8.285884587795221634, -28.45626337791865623 ) ) ;
#3999 = CARTESIAN_POINT ( 'NONE',  ( 18.84787193029120544, -29.28148226148236688, 12.14047268033136007 ) ) ;
#4000 = AXIS2_PLACEMENT_3D ( 'NONE', #38140, #1578, #16411 ) ;
#4001 = ORIENTED_EDGE ( 'NONE', *, *, #3395, .T. ) ;
#4002 = ORIENTED_EDGE ( 'NONE', *, *, #639, .F. ) ;
#4003 = DIRECTION ( 'NONE',  ( 0.000000000000000000, 0.000000000000000000, 1.000000000000000000 ) ) ;
#4004 = CARTESIAN_POINT ( 'NONE',  ( -15.75423571344012785, 25.60460891297588049, -5.000000000000002665 ) ) ;
#4005 = DIRECTION ( 'NONE',  ( 0.000000000000000000, 0.000000000000000000, 1.000000000000000000 ) ) ;
#4006 = ORIENTED_EDGE ( 'NONE', *, *, #20002, .T. ) ;
#4007 = CARTESIAN_POINT ( 'NONE',  ( -0.6823421560338360781, 34.50290607385087327, -11.97315373814747019 ) ) ;
#4008 = DIRECTION ( 'NONE',  ( 1.000000000000000000, 0.000000000000000000, 0.000000000000000000 ) ) ;
#4009 = DIRECTION ( 'NONE',  ( 0.000000000000000000, 0.000000000000000000, 1.000000000000000000 ) ) ;
#4010 = CIRCLE ( 'NONE', #2086, 0.9999999999999994449 ) ;
#4011 = DIRECTION ( 'NONE',  ( 1.000000000000000000, -2.775557561562887801E-15, 0.000000000000000000 ) ) ;
#4012 = FACE_OUTER_BOUND ( 'NONE', #3938, .T. ) ;
#4013 = CARTESIAN_POINT ( 'NONE',  ( -1.932616070714923806, 8.598021898908978500, 9.500000000000000000 ) ) ;
#4014 = CARTESIAN_POINT ( 'NONE',  ( 9.933663752171780104, 19.02636276575347551, -24.83125579025524132 ) ) ;
#4015 = DIRECTION ( 'NONE',  ( -0.000000000000000000, -0.000000000000000000, -1.000000000000000000 ) ) ;
#4016 = ORIENTED_EDGE ( 'NONE', *, *, #36452, .F. ) ;
#4018 = DIRECTION ( 'NONE',  ( -0.4999999999999912292, 0.8660254037844437036, 0.000000000000000000 ) ) ;
#4017 = CARTESIAN_POINT ( 'NONE',  ( -20.20272705719804307, 13.30714020733546299, -10.88308809810277289 ) ) ;
#4019 = CARTESIAN_POINT ( 'NONE',  ( 3.118671991557230516, 37.17221401100731981, 12.00000000000000000 ) ) ;
#4020 = EDGE_CURVE ( 'NONE', #9166, #36223, #734, .T. ) ;
#4021 = CARTESIAN_POINT ( 'NONE',  ( 15.55330811712816796, -26.75926366330655881, -5.000000000000000888 ) ) ;
#4022 = FACE_OUTER_BOUND ( 'NONE', #2368, .T. ) ;
#4023 = CARTESIAN_POINT ( 'NONE',  ( 10.95101281418289219, 17.32990059288363582, -29.34763338141241462 ) ) ;
#4024 = CARTESIAN_POINT ( 'NONE',  ( 6.023418944065099367, 39.81932404830325112, -4.999999999999995559 ) ) ;
#4025 = CARTESIAN_POINT ( 'NONE',  ( 13.24038105676655164, 15.43301270189216368, 7.000000000000000000 ) ) ;
#4026 = CARTESIAN_POINT ( 'NONE',  ( -25.92870434171245364, -25.79656239075070445, -6.305900231137221645 ) ) ;
#4027 = AXIS2_PLACEMENT_3D ( 'NONE', #27458, #15271, #8978 ) ;
#4028 = CARTESIAN_POINT ( 'NONE',  ( 8.448443376098214941, -25.22526105246425132, -6.914809992635317037 ) ) ;
#4029 = CARTESIAN_POINT ( 'NONE',  ( 11.22630306440229120, 17.54214173034566215, -26.83981274308017007 ) ) ;
#4030 = CARTESIAN_POINT ( 'NONE',  ( 17.75521226434697653, -11.99623302150457071, -25.58889124899400258 ) ) ;
#4031 = CARTESIAN_POINT ( 'NONE',  ( -6.330077540933487512, 17.71145523154927659, 12.00000000000000000 ) ) ;
#4032 = CARTESIAN_POINT ( 'NONE',  ( 1.278175571583998860, 14.08178954835375940, 9.000000000000001776 ) ) ;
#4033 = ORIENTED_EDGE ( 'NONE', *, *, #1071, .T. ) ;
#4034 = CARTESIAN_POINT ( 'NONE',  ( -9.224180078094502022, 34.72823754788878148, -8.037642107661440605 ) ) ;
#4035 = FACE_OUTER_BOUND ( 'NONE', #13688, .T. ) ;
#4036 = VERTEX_POINT ( 'NONE', #32960 ) ;
#4037 = CARTESIAN_POINT ( 'NONE',  ( 29.39456445034288734, 0.02916568486956336997, -10.65018324265741967 ) ) ;
#4038 = CARTESIAN_POINT ( 'NONE',  ( 9.788939752379329562, 23.27376113029817617, 12.00000000000000000 ) ) ;
#4039 = EDGE_CURVE ( 'NONE', #4629, #13902, #5115, .T. ) ;
#4040 = VECTOR ( 'NONE', #7090, 1000.000000000000114 ) ;
#4041 = CARTESIAN_POINT ( 'NONE',  ( -1.000000000000000000, 37.50000000000000711, 10.50000000000000000 ) ) ;
#4042 = ORIENTED_EDGE ( 'NONE', *, *, #17226, .T. ) ;
#4043 = CARTESIAN_POINT ( 'NONE',  ( -27.63060058548921916, 0.3335000238941912554, -13.52159836282129568 ) ) ;
#4044 = EDGE_CURVE ( 'NONE', #13649, #15610, #10536, .T. ) ;
#4045 = CARTESIAN_POINT ( 'NONE',  ( -19.86157371036397024, -26.35897367596445307, -9.048130446679126138 ) ) ;
#4046 = ORIENTED_EDGE ( 'NONE', *, *, #26108, .T. ) ;
#4047 = CARTESIAN_POINT ( 'NONE',  ( 32.53700013911068112, -7.740585582578115798, -11.18790742163261598 ) ) ;
#4048 = VECTOR ( 'NONE', #31176, 1000.000000000000114 ) ;
#4049 = EDGE_CURVE ( 'NONE', #22892, #39914, #33946, .T. ) ;
#4050 = EDGE_LOOP ( 'NONE', ( #8322, #8178, #2265, #11305 ) ) ;
#4051 = CARTESIAN_POINT ( 'NONE',  ( -9.308285395647398985, 37.95628792398468221, 12.14047268033065485 ) ) ;
#4052 = EDGE_CURVE ( 'NONE', #27294, #12629, #813, .T. ) ;
#4053 = LINE ( 'NONE', #13193, #32661 ) ;
#4054 = DIRECTION ( 'NONE',  ( 0.3090169943749560000, 0.9510565162951507556, 0.000000000000000000 ) ) ;
#4055 = CARTESIAN_POINT ( 'NONE',  ( 7.430899969936454852, 32.27804933232965823, 19.27171037444156454 ) ) ;
#4056 = DIRECTION ( 'NONE',  ( -1.000000000000000000, 0.000000000000000000, 0.000000000000000000 ) ) ;
#4057 = VERTEX_POINT ( 'NONE', #12801 ) ;
#4058 = CARTESIAN_POINT ( 'NONE',  ( -11.63102264767868022, 16.88415827355038346, -29.99999999999999289 ) ) ;
#4059 = CARTESIAN_POINT ( 'NONE',  ( -1.358232629781535916, 33.31072022568110924, 12.00000000000000000 ) ) ;
#4060 = AXIS2_PLACEMENT_3D ( 'NONE', #2761, #6205, #39535 ) ;
#4061 = DIRECTION ( 'NONE',  ( -0.6916548014802208488, 0.1470157664652026186, 0.7071067811865512365 ) ) ;
#4062 = CARTESIAN_POINT ( 'NONE',  ( 17.71502384555986964, 18.39420983132613330, -10.32349406737177411 ) ) ;
#4063 = AXIS2_PLACEMENT_3D ( 'NONE', #33026, #24260, #20823 ) ;
#4064 = CARTESIAN_POINT ( 'NONE',  ( 10.89528107728888884, 34.21469084972675034, -5.883532326481708985 ) ) ;
#4065 = VERTEX_POINT ( 'NONE', #6300 ) ;
#4066 = EDGE_CURVE ( 'NONE', #17580, #12323, #28042, .T. ) ;
#4067 = CARTESIAN_POINT ( 'NONE',  ( 8.796116341590819232, 23.42450908139080568, 9.000000000000001776 ) ) ;
#4068 = EDGE_CURVE ( 'NONE', #21075, #29599, #23449, .T. ) ;
#4069 = EDGE_CURVE ( 'NONE', #35744, #38427, #31829, .T. ) ;
#4070 = CARTESIAN_POINT ( 'NONE',  ( 14.39497424806422110, -24.19987066023631073, -13.45455450271301068 ) ) ;
#4071 = CARTESIAN_POINT ( 'NONE',  ( -2.594149110900493937, 26.80855565015070496, 20.99999999999999289 ) ) ;
#4072 = CARTESIAN_POINT ( 'NONE',  ( -1.100969307443859568, 12.51061230184420481, 10.50000000000000533 ) ) ;
#4073 = ORIENTED_EDGE ( 'NONE', *, *, #32797, .T. ) ;
#4074 = CARTESIAN_POINT ( 'NONE',  ( -15.33606198554360489, 26.62522709554853861, -6.887829150642375886 ) ) ;
#4075 = CIRCLE ( 'NONE', #26794, 6.000000000000005329 ) ;
#4076 = CARTESIAN_POINT ( 'NONE',  ( -32.12208287523078099, -1.273987114064245585, 16.30093088680183300 ) ) ;
#4077 = CARTESIAN_POINT ( 'NONE',  ( 14.54843269636342207, -25.89572241968321720, -9.243644732761685745 ) ) ;
#4078 = CYLINDRICAL_SURFACE ( 'NONE', #35400, 1.000000000000000000 ) ;
#4079 = ORIENTED_EDGE ( 'NONE', *, *, #34599, .T. ) ;
#4080 = ORIENTED_EDGE ( 'NONE', *, *, #34551, .F. ) ;
#4081 = CARTESIAN_POINT ( 'NONE',  ( -12.92904967086177592, 30.39550629362422640, -9.046739157839594370 ) ) ;
#4082 = CARTESIAN_POINT ( 'NONE',  ( -12.29725306327712708, -16.76881849169811645, -27.24954791152431355 ) ) ;
#4083 = VECTOR ( 'NONE', #14776, 1000.000000000000000 ) ;
#4084 = CARTESIAN_POINT ( 'NONE',  ( -12.71633695260880970, 14.58086916811587130, 10.68306085400111805 ) ) ;
#4085 = CARTESIAN_POINT ( 'NONE',  ( -20.37871563014435949, -4.364548208266203488, -27.13438481043609585 ) ) ;
#4086 = AXIS2_PLACEMENT_3D ( 'NONE', #11522, #31004, #36900 ) ;
#4087 = CARTESIAN_POINT ( 'NONE',  ( -13.46205012405082435, 15.88307354764209300, 7.318814606722385818 ) ) ;
#4088 = VERTEX_POINT ( 'NONE', #18509 ) ;
#4089 = CARTESIAN_POINT ( 'NONE',  ( 23.86586618233766188, 0.6644085514824049632, -19.51682805881153016 ) ) ;
#4090 = LINE ( 'NONE', #32337, #16147 ) ;
#4091 = DIRECTION ( 'NONE',  ( -0.8660254037844348218, 0.5000000000000066613, 0.000000000000000000 ) ) ;
#4092 = ORIENTED_EDGE ( 'NONE', *, *, #20964, .T. ) ;
#4093 = CARTESIAN_POINT ( 'NONE',  ( -21.27703557833525849, 0.7712986363537081003, -25.01410140241630842 ) ) ;
#4094 = ADVANCED_FACE ( 'NONE', ( #19 ), #9163, .F. ) ;
#4095 = CARTESIAN_POINT ( 'NONE',  ( -0.5000000000000004441, 37.00000000000000711, 9.000000000000001776 ) ) ;
#4096 = VERTEX_POINT ( 'NONE', #617 ) ;
#4097 = CARTESIAN_POINT ( 'NONE',  ( 33.89061681622978028, -4.196143601155450931, -5.000000000000000888 ) ) ;
#4098 = AXIS2_PLACEMENT_3D ( 'NONE', #37555, #12566, #7256 ) ;
#4099 = CARTESIAN_POINT ( 'NONE',  ( 10.98647152928294446, 17.30743895948372213, -29.99999999999999289 ) ) ;
#4100 = CARTESIAN_POINT ( 'NONE',  ( 22.45589477776615084, -27.55224120904853180, 15.72805884748925465 ) ) ;
#4101 = ORIENTED_EDGE ( 'NONE', *, *, #38640, .F. ) ;
#4102 = CARTESIAN_POINT ( 'NONE',  ( -15.42165057838474063, 26.78649484830226157, 16.30093088680190405 ) ) ;
#4103 = LINE ( 'NONE', #2475, #16306 ) ;
#4104 = CARTESIAN_POINT ( 'NONE',  ( 5.870938322429559264, 25.61771427147129998, 20.94377226548379056 ) ) ;
#4105 = CONICAL_SURFACE ( 'NONE', #7997, 0.5000000000000007772, 0.7853981633974519427 ) ;
#4106 = CYLINDRICAL_SURFACE ( 'NONE', #33056, 0.5000000000000004441 ) ;
#4107 = CYLINDRICAL_SURFACE ( 'NONE', #3280, 0.5000000000000004441 ) ;
#4108 = VECTOR ( 'NONE', #32621, 1000.000000000000114 ) ;
#4109 = CARTESIAN_POINT ( 'NONE',  ( -3.326590493086956091, 6.849639119454676184, 13.00000000000000178 ) ) ;
#4110 = CARTESIAN_POINT ( 'NONE',  ( 27.25314217023234775, 3.686469637062584681, 16.30093088681134006 ) ) ;
#4111 = CARTESIAN_POINT ( 'NONE',  ( -21.34187245812352529, 8.386113929568535852, -16.94052806468766548 ) ) ;
#4112 = EDGE_CURVE ( 'NONE', #2130, #28310, #12993, .T. ) ;
#4113 = CARTESIAN_POINT ( 'NONE',  ( 12.90178368060855263, -16.18855991010415352, -27.88622185041034029 ) ) ;
#4114 = CARTESIAN_POINT ( 'NONE',  ( -10.44103466624267185, 32.57396620494226624, 7.500000000000004441 ) ) ;
#4115 = EDGE_CURVE ( 'NONE', #28177, #21498, #9365, .T. ) ;
#4116 = CARTESIAN_POINT ( 'NONE',  ( 15.18601210727193518, 26.56355505085192448, -7.822568326478698708 ) ) ;
#4117 = CIRCLE ( 'NONE', #9328, 6.000000000000010658 ) ;
#4118 = ORIENTED_EDGE ( 'NONE', *, *, #15991, .F. ) ;
#4119 = CARTESIAN_POINT ( 'NONE',  ( -12.11973687156280732, 16.88561127307271548, -26.91797464023488473 ) ) ;
#4120 = CARTESIAN_POINT ( 'NONE',  ( -31.52520841578658306, -13.67397774227592500, 19.27171037444156099 ) ) ;
#4121 = DIRECTION ( 'NONE',  ( -0.1470157664652030627, -0.6916548014802235134, -0.7071067811865485719 ) ) ;
#4122 = CARTESIAN_POINT ( 'NONE',  ( 14.32550604534909944, 24.38408524461923932, -12.55371337434965540 ) ) ;
#4123 = VERTEX_POINT ( 'NONE', #220 ) ;
#4124 = CARTESIAN_POINT ( 'NONE',  ( 18.24555790293216972, -9.366475481951450632, -29.21293379095443754 ) ) ;
#4125 = CYLINDRICAL_SURFACE ( 'NONE', #37167, 6.000000000000015987 ) ;
#4126 = ORIENTED_EDGE ( 'NONE', *, *, #23455, .T. ) ;
#4128 = CARTESIAN_POINT ( 'NONE',  ( 7.645071344821493753, 9.594463043616155318, 7.000000000000000000 ) ) ;
#4127 = CARTESIAN_POINT ( 'NONE',  ( -13.31479659943831528, 23.16958864656041328, -15.41030129701651141 ) ) ;
#4129 = CARTESIAN_POINT ( 'NONE',  ( -10.68831967236590863, -19.00044293756837988, -23.79478829776460458 ) ) ;
#4130 = CARTESIAN_POINT ( 'NONE',  ( 12.09742388243072675, 14.36084852659828215, 10.49999999999999822 ) ) ;
#4131 = AXIS2_PLACEMENT_3D ( 'NONE', #31247, #27797, #6842 ) ;
#4132 = VERTEX_POINT ( 'NONE', #12999 ) ;
#4133 = CARTESIAN_POINT ( 'NONE',  ( -24.40510592067864337, -10.95802276781445350, -18.63885804247661682 ) ) ;
#4134 = CARTESIAN_POINT ( 'NONE',  ( -11.02229136415891375, -21.55589928887741280, -18.53673214569949934 ) ) ;
#4135 = CARTESIAN_POINT ( 'NONE',  ( -0.5000000000000008882, 36.00000000000000711, 10.00000000000000000 ) ) ;
#4136 = CARTESIAN_POINT ( 'NONE',  ( 12.78138401561641757, 16.34997449607922704, -26.96911998264180355 ) ) ;
#4137 = VERTEX_POINT ( 'NONE', #9564 ) ;
#4138 = CARTESIAN_POINT ( 'NONE',  ( 22.55500308376087659, 3.759694506050656138, -19.82441702495482616 ) ) ;
#4139 = DIRECTION ( 'NONE',  ( 0.000000000000000000, 0.000000000000000000, -1.000000000000000000 ) ) ;
#4140 = CARTESIAN_POINT ( 'NONE',  ( -24.49409870380020848, -11.70597971641812407, 23.00000000000000000 ) ) ;
#4141 = ORIENTED_EDGE ( 'NONE', *, *, #19454, .F. ) ;
#4142 = CARTESIAN_POINT ( 'NONE',  ( -30.17172327769580065, -0.1653024818763443871, -9.226241714221277590 ) ) ;
#4143 = EDGE_CURVE ( 'NONE', #10321, #30937, #21947, .T. ) ;
#4144 = CARTESIAN_POINT ( 'NONE',  ( 28.13187736273904349, -0.3339339482611098364, -13.45785432263379278 ) ) ;
#4145 = ADVANCED_FACE ( 'NONE', ( #25197 ), #6498, .F. ) ;
#4146 = CARTESIAN_POINT ( 'NONE',  ( 23.32346807013517775, -20.39486175172845961, 20.25080042701565830 ) ) ;
#4147 = EDGE_LOOP ( 'NONE', ( #30293, #895, #25239, #29580 ) ) ;
#4148 = CARTESIAN_POINT ( 'NONE',  ( -37.49625565938783467, -14.69322820095472792, -14.45070082761207964 ) ) ;
#4149 = CIRCLE ( 'NONE', #8717, 6.000000000000003553 ) ;
#4150 = FACE_OUTER_BOUND ( 'NONE', #30902, .T. ) ;
#4151 = EDGE_CURVE ( 'NONE', #33408, #33800, #28245, .T. ) ;
#4152 = CARTESIAN_POINT ( 'NONE',  ( 19.48557158514997667, 33.74999999999982236, 7.000000000000000000 ) ) ;
#4153 = CIRCLE ( 'NONE', #4063, 1.000000000000000888 ) ;
#4154 = LINE ( 'NONE', #16559, #30802 ) ;
#4155 = CIRCLE ( 'NONE', #11319, 1.000000000000000000 ) ;
#4156 = CARTESIAN_POINT ( 'NONE',  ( -11.40045278936307405, 32.09219743356619858, 10.82238787011334935 ) ) ;
#4157 = CARTESIAN_POINT ( 'NONE',  ( -19.48557158514998022, -11.24999999999982414, 0.000000000000000000 ) ) ;
#4158 = CARTESIAN_POINT ( 'NONE',  ( 13.03339520833710985, 15.55251603720134668, 10.94611345180490680 ) ) ;
#4159 = VERTEX_POINT ( 'NONE', #37786 ) ;
#4160 = CARTESIAN_POINT ( 'NONE',  ( -6.373266493267534472, 35.58529424598371094, 10.99999999999999289 ) ) ;
#4161 = CARTESIAN_POINT ( 'NONE',  ( -8.137585970691985082, 29.15429895402941440, 10.50000000000000000 ) ) ;
#4162 = CARTESIAN_POINT ( 'NONE',  ( 28.31258885558161253, -24.58735582524956342, -5.865897150960025286 ) ) ;
#4163 = EDGE_CURVE ( 'NONE', #14259, #28327, #11470, .T. ) ;
#4164 = EDGE_CURVE ( 'NONE', #20190, #33341, #38375, .T. ) ;
#4165 = CARTESIAN_POINT ( 'NONE',  ( -10.14158519589098795, 20.93132230382252246, 10.74999999999998579 ) ) ;
#4166 = CARTESIAN_POINT ( 'NONE',  ( 3.118671991557230516, 37.17221401100731981, 12.00000000000000000 ) ) ;
#4167 = EDGE_CURVE ( 'NONE', #35366, #36352, #22535, .T. ) ;
#4168 = CARTESIAN_POINT ( 'NONE',  ( 13.53694675301034778, 23.90144292339553189, -14.42396455730128579 ) ) ;
#4169 = CARTESIAN_POINT ( 'NONE',  ( -8.927394655428429360, 11.06314620770957013, 7.000000000000000000 ) ) ;
#4170 = VERTEX_POINT ( 'NONE', #4260 ) ;
#4171 = CARTESIAN_POINT ( 'NONE',  ( -17.39859292866695029, 20.78101578164080010, -5.953700940668370301 ) ) ;
#4172 = AXIS2_PLACEMENT_3D ( 'NONE', #25748, #13358, #13966 ) ;
#4173 = CARTESIAN_POINT ( 'NONE',  ( 18.84567888139521230, -29.34375185562581478, 11.00000000000044764 ) ) ;
#4174 = CARTESIAN_POINT ( 'NONE',  ( 12.63794253860312011, -22.55737441791748310, -16.44513747313600405 ) ) ;
#4175 = FACE_OUTER_BOUND ( 'NONE', #15420, .T. ) ;
#4176 = CARTESIAN_POINT ( 'NONE',  ( 14.74027134064697364, 25.38771306981656650, -10.65372674069893755 ) ) ;
#4177 = EDGE_LOOP ( 'NONE', ( #17371, #16830, #29515, #18095 ) ) ;
#4178 = CARTESIAN_POINT ( 'NONE',  ( 15.17059102029336159, 26.29451859012213077, -8.297644773194724266 ) ) ;
#4179 = B_SPLINE_SURFACE_WITH_KNOTS ( 'NONE', 1, 3, ( 
 ( #12688, #4700, #16142, #37869, #28526, #26229, #701, #13079, #26430, #38625 ),
 ( #23184, #32744, #10044, #17105, #35584, #7742, #4901, #32545, #14242, #23987 ) ),
 .UNSPECIFIED., .F., .F., .F.,
 ( 2, 2 ),
 ( 4, 2, 2, 2, 4 ),
 ( 0.000000000000000000, 1.000000000000000000 ),
 ( -1.003840680322661605, -0.6111415986239409071, -0.2184425169252202648, 0.1742565647735004053, 0.5669556464722210753 ),
 .UNSPECIFIED. ) ;
#4180 = VERTEX_POINT ( 'NONE', #38791 ) ;
#4182 = CARTESIAN_POINT ( 'NONE',  ( -4.348113209407908464, 9.835177808069893501, 6.000000000000000000 ) ) ;
#4181 = CARTESIAN_POINT ( 'NONE',  ( -14.91084233014961669, 25.87661791010822654, -9.704681488575104709 ) ) ;
#4183 = CARTESIAN_POINT ( 'NONE',  ( -14.04223362003087772, -24.61107474274603035, -12.55102269148551208 ) ) ;
#4184 = CARTESIAN_POINT ( 'NONE',  ( -20.74852905477007781, -28.65583854707632128, 13.92931973827808712 ) ) ;
#4185 = AXIS2_PLACEMENT_3D ( 'NONE', #829, #13617, #19116 ) ;
#4186 = CARTESIAN_POINT ( 'NONE',  ( -17.76475877421862748, -11.46159631620098374, -26.26136342777560273 ) ) ;
#4187 = CARTESIAN_POINT ( 'NONE',  ( -7.027774925259491212, -25.12514353486302809, -6.439637200144365359 ) ) ;
#4188 = CARTESIAN_POINT ( 'NONE',  ( 15.01879182178246630, 24.59331309867435067, -10.67126001090663756 ) ) ;
#4189 = ORIENTED_EDGE ( 'NONE', *, *, #8503, .F. ) ;
#4190 = CARTESIAN_POINT ( 'NONE',  ( 23.27440278483144454, 9.195899915927737922, -7.420906811853504870 ) ) ;
#4191 = CARTESIAN_POINT ( 'NONE',  ( 25.06933603554838541, -26.29324009030829146, -4.999999999999998224 ) ) ;
#4192 = CYLINDRICAL_SURFACE ( 'NONE', #462, 0.5000000000000000000 ) ;
#4193 = CARTESIAN_POINT ( 'NONE',  ( -1.257289260074403992E-13, 36.85721162268941242, 17.92354375535250810 ) ) ;
#4194 = AXIS2_PLACEMENT_3D ( 'NONE', #8479, #21659, #36511 ) ;
#4195 = EDGE_LOOP ( 'NONE', ( #38731, #18506, #39505, #34141, #7421 ) ) ;
#4196 = CARTESIAN_POINT ( 'NONE',  ( -30.02427499008684464, -3.855426316731294989, -13.18754434558245592 ) ) ;
#4197 = EDGE_CURVE ( 'NONE', #21746, #4655, #32473, .T. ) ;
#4198 = VECTOR ( 'NONE', #39441, 1000.000000000000000 ) ;
#4199 = CARTESIAN_POINT ( 'NONE',  ( -9.576215452290691488, 12.54651180040780289, 20.99999999999999645 ) ) ;
#4200 = ORIENTED_EDGE ( 'NONE', *, *, #8165, .T. ) ;
#4201 = ADVANCED_FACE ( 'NONE', ( #20112 ), #13716, .T. ) ;
#4202 = CARTESIAN_POINT ( 'NONE',  ( 24.38721429972434152, -12.23686305972968924, 20.99999999999999645 ) ) ;
#4203 = DIRECTION ( 'NONE',  ( 1.000000000000000000, 0.000000000000000000, 0.000000000000000000 ) ) ;
#4204 = CARTESIAN_POINT ( 'NONE',  ( 33.47631770321904554, -15.86963776861158948, -8.848939542670445135 ) ) ;
#4205 = CARTESIAN_POINT ( 'NONE',  ( 31.38526299860049917, -24.75545609243360801, 11.55979286843934872 ) ) ;
#4206 = ORIENTED_EDGE ( 'NONE', *, *, #24248, .T. ) ;
#4207 = ORIENTED_EDGE ( 'NONE', *, *, #35998, .F. ) ;
#4208 = CARTESIAN_POINT ( 'NONE',  ( 40.48557158514985588, -11.25000000000009415, 0.000000000000000000 ) ) ;
#4209 = DIRECTION ( 'NONE',  ( -0.5254827454987561763, 0.4731467892558144928, -0.7071067811865497932 ) ) ;
#4210 = AXIS2_PLACEMENT_3D ( 'NONE', #34070, #8487, #24325 ) ;
#4211 = FACE_OUTER_BOUND ( 'NONE', #19288, .T. ) ;
#4212 = VERTEX_POINT ( 'NONE', #16661 ) ;
#4213 = CARTESIAN_POINT ( 'NONE',  ( -0.4811758688950815710, 24.69766440587928003, -20.68953053046281809 ) ) ;
#4214 = CARTESIAN_POINT ( 'NONE',  ( -11.81630298851966288, 31.79381426990562787, 7.000000000000000000 ) ) ;
#4215 = CARTESIAN_POINT ( 'NONE',  ( 4.940908595777813161, 35.94977745735560859, 7.500000000000000888 ) ) ;
#4216 = B_SPLINE_CURVE_WITH_KNOTS ( 'NONE', 3,
 ( #768, #13151, #25543, #34898, #26147, #23314, #19865, #13556 ),
 .UNSPECIFIED., .F., .F.,
 ( 4, 2, 2, 4 ),
 ( 0.000000000000000000, 0.0002364868538934252319, 0.0004729737077868504638, 0.0009459474155737089508 ),
 .UNSPECIFIED. ) ;
#4217 =( GEOMETRIC_REPRESENTATION_CONTEXT ( 3 ) GLOBAL_UNCERTAINTY_ASSIGNED_CONTEXT ( ( #35587 ) ) GLOBAL_UNIT_ASSIGNED_CONTEXT ( ( #35664, #19821, #20224 ) ) REPRESENTATION_CONTEXT ( 'NONE', 'WORKASPACE' ) );
#4218 = DIRECTION ( 'NONE',  ( 0.2876062384759395796, -0.6459741880212476195, 0.7071067811865551223 ) ) ;
#4219 = LINE ( 'NONE', #29001, #24282 ) ;
#4220 = DIRECTION ( 'NONE',  ( 0.000000000000000000, 0.000000000000000000, 1.000000000000000000 ) ) ;
#4221 = CARTESIAN_POINT ( 'NONE',  ( 14.48331725184759478, 29.32085274443433676, -4.999999999999998224 ) ) ;
#4223 = VECTOR ( 'NONE', #2231, 1000.000000000000000 ) ;
#4222 = LINE ( 'NONE', #10122, #6222 ) ;
#4224 = ORIENTED_EDGE ( 'NONE', *, *, #15317, .T. ) ;
#4227 = PLANE ( 'NONE',  #36256 ) ;
#4226 = CIRCLE ( 'NONE', #1070, 0.5000000000000002220 ) ;
#4225 = CARTESIAN_POINT ( 'NONE',  ( -17.36159938413227266, 12.22522946688932421, -23.31441648596737437 ) ) ;
#4228 = CARTESIAN_POINT ( 'NONE',  ( -19.26948696230206792, 27.85601271560034320, 22.99999999999999289 ) ) ;
#4229 = CARTESIAN_POINT ( 'NONE',  ( 9.646859339673033773, -18.23494634657538427, -28.07314365168607395 ) ) ;
#4230 = CARTESIAN_POINT ( 'NONE',  ( -5.706342468480190000, 20.64589803375067945, 12.00000000000000000 ) ) ;
#4231 = CARTESIAN_POINT ( 'NONE',  ( 11.15752963301387624, 17.77571695416434849, -26.22197368321889144 ) ) ;
#4232 = CARTESIAN_POINT ( 'NONE',  ( -9.163310636333559245, 20.63632441393290762, -20.55760979252981357 ) ) ;
#4233 = DIRECTION ( 'NONE',  ( 0.000000000000000000, 0.000000000000000000, 1.000000000000000000 ) ) ;
#4234 = CARTESIAN_POINT ( 'NONE',  ( -18.52376316179034177, -18.47445435019549720, -18.80462721719711539 ) ) ;
#4235 = CARTESIAN_POINT ( 'NONE',  ( 7.081546805360019903, -19.44107384363185531, -27.60223205082446540 ) ) ;
#4236 = CARTESIAN_POINT ( 'NONE',  ( 15.35505396563912406, 26.30757089143959604, -7.358616479543964140 ) ) ;
#4237 = CARTESIAN_POINT ( 'NONE',  ( 17.50379027647891661, 11.61388887901797062, -24.40646131754820658 ) ) ;
#4238 = LINE ( 'NONE', #7883, #3064 ) ;
#4239 = FACE_OUTER_BOUND ( 'NONE', #9065, .T. ) ;
#4240 = ORIENTED_EDGE ( 'NONE', *, *, #8884, .T. ) ;
#4241 = CARTESIAN_POINT ( 'NONE',  ( -8.515066977056928721, 31.87126067055270795, -12.07705369524776629 ) ) ;
#4242 = ORIENTED_EDGE ( 'NONE', *, *, #38933, .F. ) ;
#4243 = AXIS2_PLACEMENT_3D ( 'NONE', #11596, #17503, #4693 ) ;
#4244 = DIRECTION ( 'NONE',  ( 1.000000000000000000, 0.000000000000000000, 0.000000000000000000 ) ) ;
#4245 = EDGE_LOOP ( 'NONE', ( #5551, #27933, #35489, #36307 ) ) ;
#4246 = CARTESIAN_POINT ( 'NONE',  ( 27.17627001547444721, 0.1857076255850063362, -14.47139429581891434 ) ) ;
#4247 = CARTESIAN_POINT ( 'NONE',  ( 14.61015742389396976, 25.89965074521812127, 7.102474990965866652 ) ) ;
#4248 = PLANE ( 'NONE',  #28435 ) ;
#4249 = ORIENTED_EDGE ( 'NONE', *, *, #14847, .F. ) ;
#4250 = AXIS2_PLACEMENT_3D ( 'NONE', #22655, #1137, #22256 ) ;
#4251 = CARTESIAN_POINT ( 'NONE',  ( -20.52288541691031298, 0.9400963243053366281, -28.70984508064821839 ) ) ;
#4252 = EDGE_LOOP ( 'NONE', ( #4224, #2607, #33309, #12390 ) ) ;
#4253 = CARTESIAN_POINT ( 'NONE',  ( 34.53482489673403677, -8.269556898348005447, -8.054871878447405820 ) ) ;
#4254 = AXIS2_PLACEMENT_3D ( 'NONE', #38085, #28741, #23458 ) ;
#4255 = CIRCLE ( 'NONE', #30856, 1.000000000000004441 ) ;
#4256 = ORIENTED_EDGE ( 'NONE', *, *, #10056, .T. ) ;
#4257 = APPLICATION_PROTOCOL_DEFINITION ( 'draft international standard', 'automotive_design', 1998, #4675 ) ;
#4258 = CARTESIAN_POINT ( 'NONE',  ( 5.746222359017512993, 39.55816310746057241, 11.00000000000000533 ) ) ;
#4259 = CARTESIAN_POINT ( 'NONE',  ( 23.05386822411318803, -7.747535282638377652, 20.99999999999999645 ) ) ;
#4260 = CARTESIAN_POINT ( 'NONE',  ( 6.576253646258392038, 14.29921418520926046, 10.00000000000000000 ) ) ;
#4261 = CARTESIAN_POINT ( 'NONE',  ( 5.180310612586525920, 33.71427074068280660, 19.27171037444157164 ) ) ;
#4262 = CARTESIAN_POINT ( 'NONE',  ( -1.829593030691901284E-15, 22.50000000000001066, 0.000000000000000000 ) ) ;
#4263 = ORIENTED_EDGE ( 'NONE', *, *, #24570, .F. ) ;
#4264 = CARTESIAN_POINT ( 'NONE',  ( -2.841037392928961403, 20.34467916404557286, -29.99999999999997158 ) ) ;
#4265 = CARTESIAN_POINT ( 'NONE',  ( 9.541469607472739867, 17.40487552589537401, 12.00000000000000000 ) ) ;
#4266 = CYLINDRICAL_SURFACE ( 'NONE', #34444, 1.000000000000000888 ) ;
#4267 = CARTESIAN_POINT ( 'NONE',  ( 14.14988989334844938, 15.91125535861774232, -24.19556275385872368 ) ) ;
#4268 = CARTESIAN_POINT ( 'NONE',  ( 5.706445963761894724, 19.68930810918331531, -30.00000000000000000 ) ) ;
#4269 = ORIENTED_EDGE ( 'NONE', *, *, #29165, .T. ) ;
#4270 = CARTESIAN_POINT ( 'NONE',  ( 2.317734025672766318, 9.191051544684723851, 7.000000000000000000 ) ) ;
#4271 = CARTESIAN_POINT ( 'NONE',  ( 6.082600654608392610, 21.41965916404854298, 12.00000000000000000 ) ) ;
#4272 = EDGE_CURVE ( 'NONE', #2217, #40031, #17634, .T. ) ;
#4273 = CARTESIAN_POINT ( 'NONE',  ( 14.26185647276075663, -23.69475499396387264, -14.39420442332849603 ) ) ;
#4274 = CARTESIAN_POINT ( 'NONE',  ( 15.60391421430543701, -26.29546805949240351, 16.87380292611441490 ) ) ;
#4275 = DIRECTION ( 'NONE',  ( -0.000000000000000000, -0.000000000000000000, 1.000000000000000000 ) ) ;
#4276 = ORIENTED_EDGE ( 'NONE', *, *, #33558, .F. ) ;
#4277 = VECTOR ( 'NONE', #17643, 1000.000000000000000 ) ;
#4278 = CARTESIAN_POINT ( 'NONE',  ( -15.17696341410569971, 26.27296005008451374, -8.298199770649093310 ) ) ;
#4279 = CIRCLE ( 'NONE', #26998, 1.000000000000000000 ) ;
#4280 = CARTESIAN_POINT ( 'NONE',  ( -34.31157940325302746, -4.066883398345795264, 15.72805884748939498 ) ) ;
#4281 = CARTESIAN_POINT ( 'NONE',  ( 12.66313389477882190, -23.07460945457045653, -15.47333642705567947 ) ) ;
#4282 = EDGE_CURVE ( 'NONE', #34166, #35530, #18744, .T. ) ;
#4283 = VECTOR ( 'NONE', #18036, 1000.000000000000000 ) ;
#4284 = DIRECTION ( 'NONE',  ( 1.000000000000000000, 0.000000000000000000, 0.000000000000000000 ) ) ;
#4285 = ADVANCED_FACE ( 'NONE', ( #23148 ), #31890, .T. ) ;
#4286 = ORIENTED_EDGE ( 'NONE', *, *, #30344, .F. ) ;
#4287 = VERTEX_POINT ( 'NONE', #19496 ) ;
#4288 = CARTESIAN_POINT ( 'NONE',  ( -13.38346974784127674, 29.27610552289402079, -9.538682096344105688 ) ) ;
#4289 = LINE ( 'NONE', #34975, #19147 ) ;
#4290 = CARTESIAN_POINT ( 'NONE',  ( -12.34742388243084577, 14.79386122849067142, 11.00000000000000000 ) ) ;
#4291 = CARTESIAN_POINT ( 'NONE',  ( -27.20639438528821330, -6.708910503866349906, -16.82195059597296805 ) ) ;
#4292 = DIRECTION ( 'NONE',  ( 0.000000000000000000, 0.000000000000000000, 1.000000000000000000 ) ) ;
#4293 = EDGE_LOOP ( 'NONE', ( #26428, #20714, #33713, #2407 ) ) ;
#4294 = CARTESIAN_POINT ( 'NONE',  ( 30.63300256406853350, 0.06511367122978951871, -6.888153787381024351 ) ) ;
#4295 = LINE ( 'NONE', #35176, #38851 ) ;
#4296 = CARTESIAN_POINT ( 'NONE',  ( -0.9819677022348329842, 30.37627742347970283, 6.000000000000000000 ) ) ;
#4297 = VERTEX_POINT ( 'NONE', #1222 ) ;
#4298 = CARTESIAN_POINT ( 'NONE',  ( -20.48235837767022716, 0.8503560580662928858, -30.00000000000000000 ) ) ;
#4299 = CARTESIAN_POINT ( 'NONE',  ( -35.94977730715254438, -22.70593821294886183, 10.99999999999999822 ) ) ;
#4300 = VERTEX_POINT ( 'NONE', #10970 ) ;
#4301 = CARTESIAN_POINT ( 'NONE',  ( 29.81191106377080047, -1.966456811352005563, -12.36848069294839725 ) ) ;
#4302 = CARTESIAN_POINT ( 'NONE',  ( 3.724371395536106188, 32.23037938972932892, 6.000000000000000000 ) ) ;
#4303 = CARTESIAN_POINT ( 'NONE',  ( 22.37152845209730501, -27.08896763657755002, 16.30093088680180102 ) ) ;
#4304 = EDGE_CURVE ( 'NONE', #14016, #20580, #14005, .T. ) ;
#4305 = ORIENTED_EDGE ( 'NONE', *, *, #34579, .T. ) ;
#4306 = CARTESIAN_POINT ( 'NONE',  ( 15.87271491999989159, 26.91186955879558695, 15.72805884748939143 ) ) ;
#4307 = EDGE_CURVE ( 'NONE', #36822, #7885, #24107, .T. ) ;
#4308 = CARTESIAN_POINT ( 'NONE',  ( 16.60464863833278670, -22.41657912773326444, 19.66345542862528362 ) ) ;
#4309 = PLANE ( 'NONE',  #9174 ) ;
#4310 = CARTESIAN_POINT ( 'NONE',  ( 5.410216727984865415, 24.65457866814638876, 21.00000000000019540 ) ) ;
#4311 = AXIS2_PLACEMENT_3D ( 'NONE', #33641, #493, #21229 ) ;
#4312 = DIRECTION ( 'NONE',  ( 0.000000000000000000, -0.000000000000000000, 1.000000000000000000 ) ) ;
#4313 = VECTOR ( 'NONE', #4743, 999.9999999999998863 ) ;
#4314 = FACE_OUTER_BOUND ( 'NONE', #23220, .T. ) ;
#4315 = FACE_BOUND ( 'NONE', #17062, .T. ) ;
#4316 = CARTESIAN_POINT ( 'NONE',  ( 21.86831431663940961, 12.62567715743453967, 15.72805884748939498 ) ) ;
#4317 = CARTESIAN_POINT ( 'NONE',  ( -23.18566882249501049, 8.858897760092389717, -9.378430886998033955 ) ) ;
#4318 = CARTESIAN_POINT ( 'NONE',  ( 20.90254793926122900, -27.22588555765620555, -5.454512999748705404 ) ) ;
#4319 = CARTESIAN_POINT ( 'NONE',  ( -29.81236060003349664, -23.63427143558772414, -4.999999999999999112 ) ) ;
#4320 = ADVANCED_FACE ( 'NONE', ( #23357 ), #7906, .F. ) ;
#4321 = VERTEX_POINT ( 'NONE', #4465 ) ;
#4322 = CARTESIAN_POINT ( 'NONE',  ( 14.76369794107131561, 25.84371132707958907, -10.16615331278799239 ) ) ;
#4323 = ORIENTED_EDGE ( 'NONE', *, *, #11912, .T. ) ;
#4324 = CARTESIAN_POINT ( 'NONE',  ( -15.48761799580068477, 24.52726732821879807, -9.257161483001100422 ) ) ;
#4325 = CARTESIAN_POINT ( 'NONE',  ( -25.09931006221018635, -21.40067874915750323, 19.66345542862498164 ) ) ;
#4326 = CARTESIAN_POINT ( 'NONE',  ( -6.654030453887870067, 35.94335816374513115, 7.000000000000000000 ) ) ;
#4327 = CARTESIAN_POINT ( 'NONE',  ( 11.94259084243876856, 19.32869477811282977, -21.62580263860968444 ) ) ;
#4328 = VERTEX_POINT ( 'NONE', #1828 ) ;
#4329 = CARTESIAN_POINT ( 'NONE',  ( 33.06617957498816907, -16.93606499636205598, -8.844916697856577414 ) ) ;
#4330 = DIRECTION ( 'NONE',  ( 0.000000000000000000, 0.000000000000000000, 1.000000000000000000 ) ) ;
#4331 = ORIENTED_EDGE ( 'NONE', *, *, #5599, .T. ) ;
#4333 = CARTESIAN_POINT ( 'NONE',  ( -6.811226782241547539, 35.33967249274200384, 7.000000000000000000 ) ) ;
#4332 = CARTESIAN_POINT ( 'NONE',  ( -10.72725030361012521, 17.46952664121795351, -29.34280788466693579 ) ) ;
#4334 = CARTESIAN_POINT ( 'NONE',  ( -9.913527807423552218, -18.50616620477535790, -26.21249535246115414 ) ) ;
#4335 = CARTESIAN_POINT ( 'NONE',  ( 4.211395437248501850, 12.61633075744433796, 13.00000000000000178 ) ) ;
#4336 = VECTOR ( 'NONE', #25281, 1000.000000000000000 ) ;
#4337 = AXIS2_PLACEMENT_3D ( 'NONE', #26273, #37966, #2694 ) ;
#4338 = VERTEX_POINT ( 'NONE', #25588 ) ;
#4339 = CARTESIAN_POINT ( 'NONE',  ( -19.27950440941545551, -8.679414676085837499, -26.27594640052829433 ) ) ;
#4340 = CARTESIAN_POINT ( 'NONE',  ( -13.28943834162129711, -24.06829275115873656, -13.53237098977819386 ) ) ;
#4341 = CARTESIAN_POINT ( 'NONE',  ( 0.9819609608163288872, 14.62372257652092422, 6.000000000000000000 ) ) ;
#4342 = CARTESIAN_POINT ( 'NONE',  ( 17.28126569830730475, 21.10767333569910065, -5.000000000000001776 ) ) ;
#4343 = ORIENTED_EDGE ( 'NONE', *, *, #13774, .T. ) ;
#4344 = CARTESIAN_POINT ( 'NONE',  ( 27.51428991693143189, 2.898098800209003123, -9.288493378121359001 ) ) ;
#4345 = CARTESIAN_POINT ( 'NONE',  ( 0.000000000000000000, 22.50000000000000355, 10.00000000000000000 ) ) ;
#4346 = CARTESIAN_POINT ( 'NONE',  ( -19.30730118283917562, -16.27608008926387839, 23.00000000000000000 ) ) ;
#4347 = ORIENTED_EDGE ( 'NONE', *, *, #14214, .T. ) ;
#4348 = CARTESIAN_POINT ( 'NONE',  ( -30.27520739190695309, -0.08482538932227430550, -8.762168245153070245 ) ) ;
#4349 = CARTESIAN_POINT ( 'NONE',  ( 22.33442608700813281, 0.1860125554426316219, -22.67341905481720232 ) ) ;
#4350 = CARTESIAN_POINT ( 'NONE',  ( 29.18902924043364422, -8.936254945821255902, 20.25080042701565475 ) ) ;
#4351 = EDGE_LOOP ( 'NONE', ( #33099, #8110 ) ) ;
#4352 = EDGE_CURVE ( 'NONE', #32176, #27843, #9842, .T. ) ;
#4353 = CARTESIAN_POINT ( 'NONE',  ( -35.84808252048276955, -3.038699442442197807, -13.99876745781545218 ) ) ;
#4354 = FACE_OUTER_BOUND ( 'NONE', #13393, .T. ) ;
#4355 = CARTESIAN_POINT ( 'NONE',  ( 8.293999462566144842, 11.53598992149257008, 13.00000000000000178 ) ) ;
#4356 = DIRECTION ( 'NONE',  ( 0.000000000000000000, 0.000000000000000000, -1.000000000000000000 ) ) ;
#4357 = VECTOR ( 'NONE', #1257, 999.9999999999998863 ) ;
#4358 = AXIS2_PLACEMENT_3D ( 'NONE', #37526, #21482, #25126 ) ;
#4359 = DIRECTION ( 'NONE',  ( 0.4067366430758009299, 0.9135454576426005335, 0.000000000000000000 ) ) ;
#4360 = DIRECTION ( 'NONE',  ( 1.000000000000000000, 0.000000000000000000, 0.000000000000000000 ) ) ;
#4361 = LINE ( 'NONE', #29552, #10756 ) ;
#4362 = EDGE_LOOP ( 'NONE', ( #29197, #32537 ) ) ;
#4363 = CARTESIAN_POINT ( 'NONE',  ( -6.557822374958135470, 35.99981354310119741, 10.49999999999999289 ) ) ;
#4364 = DIRECTION ( 'NONE',  ( 0.3090169943749573878, 0.9510565162951503115, 0.000000000000000000 ) ) ;
#4365 = CARTESIAN_POINT ( 'NONE',  ( 25.15787673397105451, -23.28870960197653162, -11.13244146939240764 ) ) ;
#4366 = AXIS2_PLACEMENT_3D ( 'NONE', #26553, #29797, #38939 ) ;
#4367 = CARTESIAN_POINT ( 'NONE',  ( -0.4999999999999998890, 37.00000000000000711, 7.000000000000000000 ) ) ;
#4368 = CARTESIAN_POINT ( 'NONE',  ( 9.625795778761983001, 10.95253033666821274, 7.000000000000000000 ) ) ;
#4369 = EDGE_CURVE ( 'NONE', #13430, #13564, #28842, .T. ) ;
#4370 = CARTESIAN_POINT ( 'NONE',  ( 14.86216115821774331, 26.87648892286942726, -8.735628851188740995 ) ) ;
#4371 = PLANE ( 'NONE',  #20454 ) ;
#4372 = ORIENTED_EDGE ( 'NONE', *, *, #14614, .F. ) ;
#4373 = CARTESIAN_POINT ( 'NONE',  ( -14.47038813004304991, 14.64214536189450122, -28.23916130782108880 ) ) ;
#4374 = CARTESIAN_POINT ( 'NONE',  ( -0.3582326297815359162, 33.31072022568110924, 6.000000000000000000 ) ) ;
#4375 = ADVANCED_FACE ( 'NONE', ( #7295 ), #10360, .F. ) ;
#4376 = EDGE_CURVE ( 'NONE', #6805, #16537, #19701, .T. ) ;
#4377 = CARTESIAN_POINT ( 'NONE',  ( 13.29078025355574155, -23.61538305050886422, -14.48073411885799544 ) ) ;
#4378 = CARTESIAN_POINT ( 'NONE',  ( 13.01837422881150452, 21.26636931122159169, 6.000000000000000000 ) ) ;
#4379 = CARTESIAN_POINT ( 'NONE',  ( 11.69518638600979621, 18.90277557641397266, -22.73667561340743859 ) ) ;
#4380 = EDGE_LOOP ( 'NONE', ( #22572, #36401, #21102, #26460, #16646, #25969, #9225 ) ) ;
#4381 = CARTESIAN_POINT ( 'NONE',  ( 11.11294864066589483, 17.62134810521215655, -26.82927740383777504 ) ) ;
#4382 = ORIENTED_EDGE ( 'NONE', *, *, #18265, .F. ) ;
#4384 = CARTESIAN_POINT ( 'NONE',  ( -8.411683849014160330, 19.76687823897114882, 7.000000000000000000 ) ) ;
#4383 = CARTESIAN_POINT ( 'NONE',  ( -14.26202392583869027, 24.54848877817957487, -12.54400935092919944 ) ) ;
#4385 = CARTESIAN_POINT ( 'NONE',  ( -12.24423225742669885, -22.02408646944725845, -17.44156587861991170 ) ) ;
#4386 = CARTESIAN_POINT ( 'NONE',  ( -37.51589702892739098, -12.89337557385636579, 11.55979286843906095 ) ) ;
#4387 = EDGE_CURVE ( 'NONE', #17829, #3843, #26194, .T. ) ;
#4388 = CARTESIAN_POINT ( 'NONE',  ( -17.22654052972206173, -11.11309616262812838, -29.21339801432243988 ) ) ;
#4389 = CARTESIAN_POINT ( 'NONE',  ( -2.347924344150951192, -23.48319297452375309, -13.90098067855863029 ) ) ;
#4390 = CARTESIAN_POINT ( 'NONE',  ( 15.01671707947095769, 23.68701959088559406, -11.63761327091711095 ) ) ;
#4391 = ORIENTED_EDGE ( 'NONE', *, *, #1813, .F. ) ;
#4392 = CARTESIAN_POINT ( 'NONE',  ( 23.39763224849028234, 9.229310415396369649, -5.481604761177553797 ) ) ;
#4393 = CARTESIAN_POINT ( 'NONE',  ( 30.24562352346015714, -23.15372967338634780, -5.000000000000000000 ) ) ;
#4394 = CARTESIAN_POINT ( 'NONE',  ( -15.44574896850336287, -26.73167447641225536, -4.999999999999999112 ) ) ;
#4395 = CARTESIAN_POINT ( 'NONE',  ( -14.00263291006904964, 28.07534605033868402, 17.42190598798347168 ) ) ;
#4396 = EDGE_LOOP ( 'NONE', ( #24911, #28883, #14746, #4899 ) ) ;
#4397 = CARTESIAN_POINT ( 'NONE',  ( -20.48034806427134313, -1.125288817275917008, -29.31181698211635833 ) ) ;
#4398 = AXIS2_PLACEMENT_3D ( 'NONE', #21731, #30690, #6290 ) ;
#4399 = AXIS2_PLACEMENT_3D ( 'NONE', #23486, #14141, #36684 ) ;
#4400 = CARTESIAN_POINT ( 'NONE',  ( -11.82346474097917621, 13.60361205939885565, 20.69868183039782750 ) ) ;
#4401 = ORIENTED_EDGE ( 'NONE', *, *, #29148, .F. ) ;
#4402 = DIRECTION ( 'NONE',  ( 1.000000000000000000, 0.000000000000000000, 0.000000000000000000 ) ) ;
#4403 = DIRECTION ( 'NONE',  ( -0.9781476007338042455, 0.2079116908177663370, 0.000000000000000000 ) ) ;
#4404 = CIRCLE ( 'NONE', #25166, 18.00000000000002842 ) ;
#4405 = EDGE_CURVE ( 'NONE', #29211, #28177, #18267, .T. ) ;
#4406 = DIRECTION ( 'NONE',  ( 1.000000000000000000, 0.000000000000000000, 0.000000000000000000 ) ) ;
#4407 = CARTESIAN_POINT ( 'NONE',  ( 19.23661869638189970, -7.777357332202925022, -27.73122278007569719 ) ) ;
#4408 = EDGE_CURVE ( 'NONE', #26227, #38309, #30527, .T. ) ;
#4410 = AXIS2_PLACEMENT_3D ( 'NONE', #12099, #39527, #18796 ) ;
#4409 = CARTESIAN_POINT ( 'NONE',  ( 37.51589702892718492, -12.89337557385771049, 11.55979286843950860 ) ) ;
#4411 = ORIENTED_EDGE ( 'NONE', *, *, #30649, .F. ) ;
#4412 = CARTESIAN_POINT ( 'NONE',  ( 14.11133924723984379, 27.61078317377175750, 11.00000000000000000 ) ) ;
#4413 = CARTESIAN_POINT ( 'NONE',  ( 0.6237317017440463518, 25.43444280220171194, 6.000000000000000000 ) ) ;
#4414 = DIRECTION ( 'NONE',  ( -0.000000000000000000, -0.000000000000000000, -1.000000000000000000 ) ) ;
#4415 = EDGE_LOOP ( 'NONE', ( #2780, #2800, #21972 ) ) ;
#4416 = CARTESIAN_POINT ( 'NONE',  ( -1.011306241801401606, 20.48440008317826511, -29.21294264354560966 ) ) ;
#4417 = CARTESIAN_POINT ( 'NONE',  ( 19.48557158514988075, -11.24999999999998224, 3.000000000000000000 ) ) ;
#4418 = DIRECTION ( 'NONE',  ( 0.000000000000000000, 0.000000000000000000, 1.000000000000000000 ) ) ;
#4419 = CARTESIAN_POINT ( 'NONE',  ( 5.100636323082810009, 29.29593658752792962, 12.00000000000000000 ) ) ;
#4420 = DIRECTION ( 'NONE',  ( 0.000000000000000000, 0.000000000000000000, 1.000000000000000000 ) ) ;
#4421 = ADVANCED_FACE ( 'NONE', ( #14411 ), #36545, .T. ) ;
#4422 = CARTESIAN_POINT ( 'NONE',  ( 6.811226782241711852, 35.33967249274190436, 7.500000000000000888 ) ) ;
#4423 = CARTESIAN_POINT ( 'NONE',  ( 14.43593167022227952, 29.20741364694840314, -6.379814831040929946 ) ) ;
#4424 = CARTESIAN_POINT ( 'NONE',  ( 35.07906678349414165, -7.111640533860041913, -4.999999999999997335 ) ) ;
#4425 = AXIS2_PLACEMENT_3D ( 'NONE', #25467, #19788, #13895 ) ;
#4426 = VERTEX_POINT ( 'NONE', #38991 ) ;
#4428 = CARTESIAN_POINT ( 'NONE',  ( -2.247473515615844075, 16.63111439559750693, 12.00000000000000000 ) ) ;
#4427 = CARTESIAN_POINT ( 'NONE',  ( -20.20456973212974106, 14.66708349146731827, -4.999999999999997335 ) ) ;
#4429 = CARTESIAN_POINT ( 'NONE',  ( -0.4999999999999998890, 37.33905845026563952, 10.87262190629436098 ) ) ;
#4430 = ADVANCED_FACE ( 'NONE', ( #39189 ), #2621, .T. ) ;
#4431 = CARTESIAN_POINT ( 'NONE',  ( 14.81584271249959883, -25.66902196032313554, -10.17682674198090709 ) ) ;
#4432 = DIRECTION ( 'NONE',  ( 0.7431448254773953543, 0.6691306063588570163, 0.000000000000000000 ) ) ;
#4433 = CARTESIAN_POINT ( 'NONE',  ( 13.46442396743949210, 22.87082214237680944, -15.44440089725282839 ) ) ;
#4434 = CIRCLE ( 'NONE', #14819, 1.000000000000000000 ) ;
#4435 = CARTESIAN_POINT ( 'NONE',  ( -35.36940577612494963, -20.42053594592269761, -4.999999999999990230 ) ) ;
#4436 = FACE_OUTER_BOUND ( 'NONE', #39055, .T. ) ;
#4437 = EDGE_CURVE ( 'NONE', #2950, #7051, #18916, .T. ) ;
#4438 = CARTESIAN_POINT ( 'NONE',  ( -19.80406076264881321, -17.52161466429418724, -18.72497143683012411 ) ) ;
#4439 = CARTESIAN_POINT ( 'NONE',  ( 8.142828335362517933, -24.61856252981078441, -10.30834616846729546 ) ) ;
#4440 = CARTESIAN_POINT ( 'NONE',  ( 14.62685016563947116, 24.71383867966243386, -11.60661454720508345 ) ) ;
#4441 = CARTESIAN_POINT ( 'NONE',  ( 17.36173719094433210, 11.50338824233619661, -25.50370862539636363 ) ) ;
#4442 = FACE_OUTER_BOUND ( 'NONE', #7359, .T. ) ;
#4443 = CARTESIAN_POINT ( 'NONE',  ( -20.92112759555556067, -16.07000418475134040, 21.00000000000000355 ) ) ;
#4444 = VERTEX_POINT ( 'NONE', #5463 ) ;
#4445 = CARTESIAN_POINT ( 'NONE',  ( -5.424629926632633214, 20.35751203620437266, -26.39731167115077781 ) ) ;
#4446 = EDGE_LOOP ( 'NONE', ( #14663, #9636, #3066, #23674, #13844, #2492, #27196 ) ) ;
#4447 = CARTESIAN_POINT ( 'NONE',  ( -9.439731518140417776, -18.24720977618391515, -28.71013559075634802 ) ) ;
#4448 = DIRECTION ( 'NONE',  ( 0.2079116908177519041, -0.9781476007338072431, 0.000000000000000000 ) ) ;
#4449 = ORIENTED_EDGE ( 'NONE', *, *, #32946, .F. ) ;
#4450 = CARTESIAN_POINT ( 'NONE',  ( 29.84386241824243768, -0.001863274244196008950, -9.706340305527046297 ) ) ;
#4451 = FACE_OUTER_BOUND ( 'NONE', #10237, .T. ) ;
#4452 = CARTESIAN_POINT ( 'NONE',  ( -30.57450045107345815, -0.3656520783135126518, 16.87380292611442201 ) ) ;
#4453 = ORIENTED_EDGE ( 'NONE', *, *, #236, .F. ) ;
#4454 = CARTESIAN_POINT ( 'NONE',  ( -30.70419509168079841, 0.1269851510385121840, -5.946116814806951645 ) ) ;
#4455 = ORIENTED_EDGE ( 'NONE', *, *, #18486, .T. ) ;
#4456 = CARTESIAN_POINT ( 'NONE',  ( 34.88440358479222425, -8.370710937437479515, -7.181291740870185514 ) ) ;
#4457 = EDGE_CURVE ( 'NONE', #16497, #3811, #18067, .T. ) ;
#4458 = CIRCLE ( 'NONE', #7048, 0.5000000000000004441 ) ;
#4459 = AXIS2_PLACEMENT_3D ( 'NONE', #3693, #31529, #31922 ) ;
#4460 = ORIENTED_EDGE ( 'NONE', *, *, #22084, .T. ) ;
#4461 = DIRECTION ( 'NONE',  ( 0.000000000000000000, 0.000000000000000000, 1.000000000000000000 ) ) ;
#4462 = CARTESIAN_POINT ( 'NONE',  ( -13.80290580123969058, 34.21636679304901918, 11.00000000000033573 ) ) ;
#4463 = VECTOR ( 'NONE', #866, 1000.000000000000114 ) ;
#4464 = DIRECTION ( 'NONE',  ( 0.000000000000000000, 0.000000000000000000, 1.000000000000000000 ) ) ;
#4465 = CARTESIAN_POINT ( 'NONE',  ( 12.05736835487432579, 14.38397459621550567, 7.499999999999997335 ) ) ;
#4466 = CARTESIAN_POINT ( 'NONE',  ( -9.006936242053182440, 32.02107499576991501, 18.87996532025859864 ) ) ;
#4467 = LINE ( 'NONE', #16870, #9055 ) ;
#4468 = ORIENTED_EDGE ( 'NONE', *, *, #1727, .F. ) ;
#4469 = CARTESIAN_POINT ( 'NONE',  ( 0.000000000000000000, 0.000000000000000000, 0.000000000000000000 ) ) ;
#4470 = DIRECTION ( 'NONE',  ( 0.5720614028176880250, 0.4156269377774530760, -0.7071067811865446862 ) ) ;
#4471 = CYLINDRICAL_SURFACE ( 'NONE', #17630, 1.000000000000000888 ) ;
#4472 = DIRECTION ( 'NONE',  ( 1.000000000000000000, 0.000000000000000000, 0.000000000000000000 ) ) ;
#4473 = CARTESIAN_POINT ( 'NONE',  ( 16.97505978179442110, 15.88883797548840526, -16.88581435752053039 ) ) ;
#4474 = CARTESIAN_POINT ( 'NONE',  ( 6.476106366349275056, 22.41237707052495409, -22.08317005786570775 ) ) ;
#4475 = ORIENTED_EDGE ( 'NONE', *, *, #31463, .F. ) ;
#4476 = CARTESIAN_POINT ( 'NONE',  ( -2.853172919594720192, 21.57294901687549427, 13.00000000000000178 ) ) ;
#4477 = FACE_OUTER_BOUND ( 'NONE', #28424, .T. ) ;
#4478 = EDGE_CURVE ( 'NONE', #11050, #29636, #14953, .T. ) ;
#4479 = CARTESIAN_POINT ( 'NONE',  ( 13.07819759976932694, -21.99233217153179609, -17.34750951402496000 ) ) ;
#4480 = CARTESIAN_POINT ( 'NONE',  ( 14.01837422881150452, 21.26636931122159169, 13.00000000000000178 ) ) ;
#4481 = LINE ( 'NONE', #16886, #14670 ) ;
#4482 = CIRCLE ( 'NONE', #37576, 18.00000000000000000 ) ;
#4483 = ORIENTED_EDGE ( 'NONE', *, *, #38781, .T. ) ;
#4485 = CIRCLE ( 'NONE', #27195, 0.5000000000000000000 ) ;
#4484 = CARTESIAN_POINT ( 'NONE',  ( -11.48643516040400669, 18.43546103647281953, -23.85432110392739347 ) ) ;
#4486 = CARTESIAN_POINT ( 'NONE',  ( -33.75286824399729824, -19.48722756659376998, 15.72805884748939853 ) ) ;
#4487 = CARTESIAN_POINT ( 'NONE',  ( 10.18006096829566332, -19.67814488976349452, -22.77776888065764638 ) ) ;
#4488 = DIRECTION ( 'NONE',  ( 1.000000000000000000, 1.224646799147351235E-16, -0.000000000000000000 ) ) ;
#4489 = ORIENTED_EDGE ( 'NONE', *, *, #8305, .F. ) ;
#4490 = ORIENTED_EDGE ( 'NONE', *, *, #16846, .T. ) ;
#4491 = CIRCLE ( 'NONE', #28492, 0.9999999999999995559 ) ;
#4492 = CARTESIAN_POINT ( 'NONE',  ( -13.01238674544895169, 30.61633392914591667, -8.594047575497109293 ) ) ;
#4493 = CARTESIAN_POINT ( 'NONE',  ( -14.02522277065907019, -18.92975099516724313, -21.21400967010290373 ) ) ;
#4494 = FACE_OUTER_BOUND ( 'NONE', #4415, .T. ) ;
#4495 = CARTESIAN_POINT ( 'NONE',  ( -33.66249016428778873, -7.316504645895227199, -9.400858107290300580 ) ) ;
#4496 = DIRECTION ( 'NONE',  ( 0.2185080122244173473, 0.6724985119639624864, -0.7071067811865404673 ) ) ;
#4497 = ORIENTED_EDGE ( 'NONE', *, *, #22300, .T. ) ;
#4498 = CARTESIAN_POINT ( 'NONE',  ( 28.77352987854749600, 0.2413197295406705467, -11.60410763981559867 ) ) ;
#4499 = CYLINDRICAL_SURFACE ( 'NONE', #3730, 1.000000000000000000 ) ;
#4500 = DIRECTION ( 'NONE',  ( 0.8090169943749423442, -0.5877852522924800205, 0.000000000000000000 ) ) ;
#4501 = DIRECTION ( 'NONE',  ( 0.000000000000000000, 0.000000000000000000, 1.000000000000000000 ) ) ;
#4502 = ORIENTED_EDGE ( 'NONE', *, *, #11668, .F. ) ;
#4503 = CARTESIAN_POINT ( 'NONE',  ( -30.90411674721317326, -0.04211297212934830836, -4.999999999999999112 ) ) ;
#4504 = CARTESIAN_POINT ( 'NONE',  ( -15.96050091527624559, -30.99544168074540806, 11.00000000000000178 ) ) ;
#4505 = ORIENTED_EDGE ( 'NONE', *, *, #6887, .F. ) ;
#4506 = CARTESIAN_POINT ( 'NONE',  ( 27.24177960840210133, -2.437714896029509415, -16.14381839494960857 ) ) ;
#4507 = DIRECTION ( 'NONE',  ( 1.000000000000000000, 0.000000000000000000, 0.000000000000000000 ) ) ;
#4508 = CARTESIAN_POINT ( 'NONE',  ( 24.32690616642214465, -27.49953951067901414, 15.13084544680245713 ) ) ;
#4509 = EDGE_CURVE ( 'NONE', #16240, #10384, #34157, .T. ) ;
#4510 = ORIENTED_EDGE ( 'NONE', *, *, #21090, .F. ) ;
#4511 = CARTESIAN_POINT ( 'NONE',  ( -1.732136883777231740, 38.50629078351121137, 16.30093088680190050 ) ) ;
#4512 = EDGE_CURVE ( 'NONE', #15610, #32625, #33159, .T. ) ;
#4513 = CARTESIAN_POINT ( 'NONE',  ( 4.327222458066418466E-14, -22.50706359516090060, 18.42518152272108978 ) ) ;
#4514 = CARTESIAN_POINT ( 'NONE',  ( -6.354454053420248272, 35.54304081427989814, 7.500000000000000888 ) ) ;
#4515 = CARTESIAN_POINT ( 'NONE',  ( 2.374005179830479761, 29.54744178790033260, 20.82122704794079837 ) ) ;
#4516 = AXIS2_PLACEMENT_3D ( 'NONE', #1125, #13506, #10671 ) ;
#4517 = CARTESIAN_POINT ( 'NONE',  ( 11.11016527260166420, 31.83082137946473367, 7.000000000000000000 ) ) ;
#4518 = DIRECTION ( 'NONE',  ( 1.000000000000000000, 0.000000000000000000, 0.000000000000000000 ) ) ;
#4519 = EDGE_CURVE ( 'NONE', #17087, #11673, #12416, .T. ) ;
#4520 = AXIS2_PLACEMENT_3D ( 'NONE', #37548, #37145, #3412 ) ;
#4521 = CARTESIAN_POINT ( 'NONE',  ( 4.392928914044564870, 32.84871041364772282, -12.91564532669888443 ) ) ;
#4522 = LINE ( 'NONE', #26452, #17130 ) ;
#4523 = CARTESIAN_POINT ( 'NONE',  ( 29.28423149095877775, -1.632116715646416472, 18.42518152272108978 ) ) ;
#4524 = CARTESIAN_POINT ( 'NONE',  ( -21.91691631266333218, 8.533117302549259264, -14.88445492063216058 ) ) ;
#4525 = CARTESIAN_POINT ( 'NONE',  ( 20.45602243971594802, -26.70709334009890412, -8.136195482540582447 ) ) ;
#4526 = DIRECTION ( 'NONE',  ( 0.000000000000000000, 0.000000000000000000, 1.000000000000000000 ) ) ;
#4527 = CARTESIAN_POINT ( 'NONE',  ( 14.65949890303364711, 25.62925135841399182, -10.63803580328918130 ) ) ;
#4528 = ORIENTED_EDGE ( 'NONE', *, *, #22968, .F. ) ;
#4529 = CARTESIAN_POINT ( 'NONE',  ( -11.73368784223909600, 16.86169632780890026, -28.73611812094127060 ) ) ;
#4530 = CARTESIAN_POINT ( 'NONE',  ( -17.92913371968332825, -21.93458435334723333, 19.99202127657105876 ) ) ;
#4531 = EDGE_CURVE ( 'NONE', #23343, #14560, #22073, .T. ) ;
#4532 = CARTESIAN_POINT ( 'NONE',  ( -75.15099915297791711, 43.38844959084113384, 0.000000000000000000 ) ) ;
#4533 = CARTESIAN_POINT ( 'NONE',  ( 15.05161315844539693, 25.86266507323037800, -9.239641103395126009 ) ) ;
#4534 = ORIENTED_EDGE ( 'NONE', *, *, #27652, .F. ) ;
#4535 = CARTESIAN_POINT ( 'NONE',  ( 21.61405347744884153, -11.92327965266493983, -20.69245384154366363 ) ) ;
#4536 = ORIENTED_EDGE ( 'NONE', *, *, #17259, .F. ) ;
#4538 = DIRECTION ( 'NONE',  ( -0.000000000000000000, -0.000000000000000000, -1.000000000000000000 ) ) ;
#4537 = CARTESIAN_POINT ( 'NONE',  ( -10.79835490039502410, 17.42544872524608479, -29.34434079418894470 ) ) ;
#4539 = CARTESIAN_POINT ( 'NONE',  ( -15.79675373760014523, -26.30866209883446771, -8.737002122218552103 ) ) ;
#4540 = CYLINDRICAL_SURFACE ( 'NONE', #17875, 1.000000000000000888 ) ;
#4541 = CIRCLE ( 'NONE', #6473, 15.00000000000000000 ) ;
#4542 = ORIENTED_EDGE ( 'NONE', *, *, #15471, .T. ) ;
#4543 = CARTESIAN_POINT ( 'NONE',  ( -33.91942916316902057, -12.79638493585070869, -9.310156918177783680 ) ) ;
#4544 = CARTESIAN_POINT ( 'NONE',  ( -14.61288958351504164, -26.24343134248350040, -7.831338513189715300 ) ) ;
#4545 = DIRECTION ( 'NONE',  ( -0.000000000000000000, -0.000000000000000000, -1.000000000000000000 ) ) ;
#4546 = CARTESIAN_POINT ( 'NONE',  ( 14.31707047546269607, 16.20057490539070955, -23.09683113071953997 ) ) ;
#4547 = ORIENTED_EDGE ( 'NONE', *, *, #34823, .T. ) ;
#4548 = CARTESIAN_POINT ( 'NONE',  ( 22.12115478089299714, 3.764118972416656828, -20.87897183709134197 ) ) ;
#4549 = FACE_OUTER_BOUND ( 'NONE', #16582, .T. ) ;
#4550 = CARTESIAN_POINT ( 'NONE',  ( -39.05366788732968786, -6.582903524762039993, 22.99999999999811351 ) ) ;
#4551 = AXIS2_PLACEMENT_3D ( 'NONE', #19648, #29201, #38136 ) ;
#4552 = ORIENTED_EDGE ( 'NONE', *, *, #23555, .F. ) ;
#4553 = CARTESIAN_POINT ( 'NONE',  ( -28.49039815446405299, -0.04531349955599923290, -12.53146938658677456 ) ) ;
#4554 = CARTESIAN_POINT ( 'NONE',  ( 21.01377214067982280, 0.3319268877385900818, -26.18275839778970848 ) ) ;
#4555 = CARTESIAN_POINT ( 'NONE',  ( 30.12142568021469557, -17.39061322484706196, 19.27171037444156454 ) ) ;
#4556 = EDGE_CURVE ( 'NONE', #5579, #253, #17873, .T. ) ;
#4557 = ORIENTED_EDGE ( 'NONE', *, *, #18014, .F. ) ;
#4558 = CARTESIAN_POINT ( 'NONE',  ( -27.68563775692442874, 0.9759262997041426857, -12.58874013869143482 ) ) ;
#4559 = CARTESIAN_POINT ( 'NONE',  ( 2.927345865710861972E-15, 22.57051819516765789, -19.69475445967420768 ) ) ;
#4560 = B_SPLINE_CURVE_WITH_KNOTS ( 'NONE', 3,
 ( #18167, #34197, #8818, #18950, #2718, #15107 ),
 .UNSPECIFIED., .F., .F.,
 ( 4, 2, 4 ),
 ( 0.000000000000000000, 0.5000000000000000000, 1.000000000000000000 ),
 .UNSPECIFIED. ) ;
#4561 = DIRECTION ( 'NONE',  ( 0.6691306063588671194, 0.7431448254773861395, 0.000000000000000000 ) ) ;
#4562 = CONICAL_SURFACE ( 'NONE', #37645, 1.000000000000014655, 0.7853981633974526089 ) ;
#4563 = CARTESIAN_POINT ( 'NONE',  ( -9.831584923911586671, 26.22020669908462764, 10.50000000000000000 ) ) ;
#4564 = EDGE_CURVE ( 'NONE', #24685, #38824, #35951, .T. ) ;
#4565 = EDGE_CURVE ( 'NONE', #7663, #18302, #32911, .T. ) ;
#4566 = LINE ( 'NONE', #20012, #3927 ) ;
#4567 = DIRECTION ( 'NONE',  ( 0.000000000000000000, 0.000000000000000000, 1.000000000000000000 ) ) ;
#4568 = DIRECTION ( 'NONE',  ( 0.1045284632676570929, 0.9945218953682730678, -0.000000000000000000 ) ) ;
#4569 = ORIENTED_EDGE ( 'NONE', *, *, #39478, .T. ) ;
#4570 = CARTESIAN_POINT ( 'NONE',  ( 1.590043107810628298, 12.61456814725305442, 10.49999999999999467 ) ) ;
#4571 = CARTESIAN_POINT ( 'NONE',  ( -1.828660225306042442, 9.087095699275883121, 10.50000000000000000 ) ) ;
#4572 = CARTESIAN_POINT ( 'NONE',  ( 20.10367939777714597, -18.56949155725344625, -17.72620543299270679 ) ) ;
#4573 = AXIS2_PLACEMENT_3D ( 'NONE', #14961, #34448, #12115 ) ;
#4574 = LINE ( 'NONE', #4165, #29029 ) ;
#4575 = CARTESIAN_POINT ( 'NONE',  ( -8.294006203984645609, 33.46401007850805343, 13.00000000000000178 ) ) ;
#4576 = CARTESIAN_POINT ( 'NONE',  ( 12.61634089041212192, 22.15519939570359043, -17.36970231665867104 ) ) ;
#4577 = DIRECTION ( 'NONE',  ( -0.8090169943749426773, 0.5877852522924797984, 0.000000000000000000 ) ) ;
#4578 = ORIENTED_EDGE ( 'NONE', *, *, #688, .T. ) ;
#4579 = CARTESIAN_POINT ( 'NONE',  ( -14.67830838625119760, 14.96923418678847462, -25.37387372424442944 ) ) ;
#4580 = FACE_OUTER_BOUND ( 'NONE', #34181, .T. ) ;
#4581 = ADVANCED_FACE ( 'NONE', ( #30051 ), #4562, .T. ) ;
#4582 = CARTESIAN_POINT ( 'NONE',  ( 12.93205350682161026, -23.08767904844866337, -15.45577339185666155 ) ) ;
#4583 = EDGE_CURVE ( 'NONE', #8501, #27275, #27005, .T. ) ;
#4584 = FACE_OUTER_BOUND ( 'NONE', #23081, .T. ) ;
#4585 = CARTESIAN_POINT ( 'NONE',  ( 15.42600414702388001, 26.74738280129588475, -5.000000000000002665 ) ) ;
#4586 = VERTEX_POINT ( 'NONE', #23956 ) ;
#4587 = CARTESIAN_POINT ( 'NONE',  ( 12.64961623683766412, 21.05878950761225354, -18.45162358594998153 ) ) ;
#4588 = EDGE_LOOP ( 'NONE', ( #21407, #5230, #40183, #19119 ) ) ;
#4590 = DIRECTION ( 'NONE',  ( -0.000000000000000000, -0.000000000000000000, -1.000000000000000000 ) ) ;
#4589 = CARTESIAN_POINT ( 'NONE',  ( -15.39213581000993436, 26.86843326188214576, -5.000000000000001776 ) ) ;
#4591 = CARTESIAN_POINT ( 'NONE',  ( -9.613986047678359625, -18.34424821771797198, -27.44831228072173346 ) ) ;
#4592 = CARTESIAN_POINT ( 'NONE',  ( -37.34232268491270190, -8.983628415038371173, 11.55979286843934872 ) ) ;
#4593 = VECTOR ( 'NONE', #37937, 1000.000000000000000 ) ;
#4594 = CARTESIAN_POINT ( 'NONE',  ( -17.22680934732288449, -11.86017600268841576, -26.97611126009332594 ) ) ;
#4595 = CARTESIAN_POINT ( 'NONE',  ( -8.692887668960288750, -24.30300274338556932, -11.76202580396936703 ) ) ;
#4596 = CARTESIAN_POINT ( 'NONE',  ( 13.77818766908856496, 21.23702865708559528, -16.52942667850394898 ) ) ;
#4597 = ORIENTED_EDGE ( 'NONE', *, *, #32250, .F. ) ;
#4598 = CARTESIAN_POINT ( 'NONE',  ( 22.26820236916659468, 7.937833278018120886, -14.86918834064916339 ) ) ;
#4599 = AXIS2_PLACEMENT_3D ( 'NONE', #28743, #23053, #23263 ) ;
#4600 = DIRECTION ( 'NONE',  ( 0.4999999999999919509, -0.8660254037844432595, 0.000000000000000000 ) ) ;
#4601 = CARTESIAN_POINT ( 'NONE',  ( -10.04974741695039242, 22.44923726269184527, 10.49999999999999467 ) ) ;
#4602 = DIRECTION ( 'NONE',  ( -0.2079116908177663092, -0.9781476007338040235, 0.000000000000000000 ) ) ;
#4603 = ORIENTED_EDGE ( 'NONE', *, *, #20515, .F. ) ;
#4604 = CARTESIAN_POINT ( 'NONE',  ( -21.48125279631567608, -1.916317976078901753, -24.72592479754959172 ) ) ;
#4605 = CARTESIAN_POINT ( 'NONE',  ( -7.976544127345993829, 18.48053530966456037, 20.94377226548371596 ) ) ;
#4606 = ORIENTED_EDGE ( 'NONE', *, *, #7349, .T. ) ;
#4607 = DIRECTION ( 'NONE',  ( 0.000000000000000000, 0.000000000000000000, 1.000000000000000000 ) ) ;
#4608 = CARTESIAN_POINT ( 'NONE',  ( 0.6237317017440463518, 25.43444280220171194, 12.00000000000000000 ) ) ;
#4609 = CONICAL_SURFACE ( 'NONE', #11748, 1.000000000000002665, 0.7853981633974532750 ) ;
#4610 = EDGE_CURVE ( 'NONE', #38482, #6428, #36350, .T. ) ;
#4611 = FACE_OUTER_BOUND ( 'NONE', #29914, .T. ) ;
#4612 = CARTESIAN_POINT ( 'NONE',  ( 21.43836447692151737, -10.19457909919293748, -21.85517601310809965 ) ) ;
#4613 = CARTESIAN_POINT ( 'NONE',  ( 37.14493776307928385, -9.008680429015726077, 12.73282698324853435 ) ) ;
#4614 = EDGE_LOOP ( 'NONE', ( #6625, #10565, #8299, #19367, #37634 ) ) ;
#4615 = CARTESIAN_POINT ( 'NONE',  ( 12.19971670159632637, 4.637739668175409058, 7.500000000000010658 ) ) ;
#4616 = LINE ( 'NONE', #10924, #4593 ) ;
#4617 = AXIS2_PLACEMENT_3D ( 'NONE', #7761, #29901, #38243 ) ;
#4618 = CARTESIAN_POINT ( 'NONE',  ( 5.547064146435681131, 36.18820672788721993, 10.94611345180490680 ) ) ;
#4619 = DIRECTION ( 'NONE',  ( 0.000000000000000000, 0.000000000000000000, 1.000000000000000000 ) ) ;
#4620 = CARTESIAN_POINT ( 'NONE',  ( -0.7148412076571604157, 36.18692081534198479, -10.17225141934236277 ) ) ;
#4621 = VECTOR ( 'NONE', #26848, 1000.000000000000000 ) ;
#4622 = CARTESIAN_POINT ( 'NONE',  ( -13.42604558747169463, 21.08886574588681384, 7.000000000000000000 ) ) ;
#4623 = CARTESIAN_POINT ( 'NONE',  ( 5.947717410344610656, 34.62949535663720013, 10.00000000000000000 ) ) ;
#4624 = CARTESIAN_POINT ( 'NONE',  ( 27.36225479889086287, 10.16098284204021240, 10.99999999999999645 ) ) ;
#4625 = FACE_OUTER_BOUND ( 'NONE', #4729, .T. ) ;
#4626 = CARTESIAN_POINT ( 'NONE',  ( 14.26584437371809777, 27.13525491562438319, 13.00000000000000178 ) ) ;
#4627 = CARTESIAN_POINT ( 'NONE',  ( 14.40481049750849785, 29.13314888007769810, -6.837637242531308779 ) ) ;
#4628 = CARTESIAN_POINT ( 'NONE',  ( 35.48557158208991069, -9.180432008922032594, -4.999999999999999112 ) ) ;
#4629 = VERTEX_POINT ( 'NONE', #36949 ) ;
#4631 = DIRECTION ( 'NONE',  ( -0.8090169943749426773, 0.5877852522924797984, 0.000000000000000000 ) ) ;
#4630 = CARTESIAN_POINT ( 'NONE',  ( -20.02443676921326698, 14.51187564404416719, -8.402881453741647633 ) ) ;
#4632 = DIRECTION ( 'NONE',  ( -1.000000000000000000, 0.000000000000000000, 0.000000000000000000 ) ) ;
#4633 = CARTESIAN_POINT ( 'NONE',  ( 15.11688860189568295, -26.15468757429319169, -8.766268934131305812 ) ) ;
#4634 = CARTESIAN_POINT ( 'NONE',  ( 0.000000000000000000, 22.50000000000000355, 12.00000000000000000 ) ) ;
#4635 = CARTESIAN_POINT ( 'NONE',  ( 15.15954330274506923, 26.33225921297029970, -8.295889340952182778 ) ) ;
#4636 = CARTESIAN_POINT ( 'NONE',  ( -13.47223693944937040, 18.09844039693852125, -21.24786896499725231 ) ) ;
#4637 = CARTESIAN_POINT ( 'NONE',  ( 4.476901250629513385, 26.36149378532653031, 13.00000000000000178 ) ) ;
#4638 = ADVANCED_FACE ( 'NONE', ( #39984 ), #21700, .T. ) ;
#4639 = CARTESIAN_POINT ( 'NONE',  ( -16.49540125530320722, -15.47634539844835011, -23.14752693098630942 ) ) ;
#4640 = CARTESIAN_POINT ( 'NONE',  ( 3.412941554391075716, -22.67929815799855220, -16.95258892673083295 ) ) ;
#4641 = CARTESIAN_POINT ( 'NONE',  ( 15.49509892345262330, 26.24234491965495764, -6.417516081753649182 ) ) ;
#4642 = CARTESIAN_POINT ( 'NONE',  ( 21.05838016133584389, 12.97903285513515925, -6.453896350353760525 ) ) ;
#4643 = CARTESIAN_POINT ( 'NONE',  ( -3.607749162633401507, 7.931741834401821123, 11.00000000000000000 ) ) ;
#4644 = ORIENTED_EDGE ( 'NONE', *, *, #35287, .T. ) ;
#4645 = CARTESIAN_POINT ( 'NONE',  ( -5.935793614171071653, 34.20645656082695041, -11.10577846936933000 ) ) ;
#4646 = ORIENTED_EDGE ( 'NONE', *, *, #30393, .T. ) ;
#4647 = AXIS2_PLACEMENT_3D ( 'NONE', #20118, #29450, #10365 ) ;
#4648 = CARTESIAN_POINT ( 'NONE',  ( 13.47830981910552062, 21.58612669357076896, 10.50000000000000000 ) ) ;
#4649 = ORIENTED_EDGE ( 'NONE', *, *, #5889, .T. ) ;
#4650 = VECTOR ( 'NONE', #32510, 1000.000000000000227 ) ;
#4651 = DIRECTION ( 'NONE',  ( 1.000000000000000000, 0.000000000000000000, 0.000000000000000000 ) ) ;
#4652 = CARTESIAN_POINT ( 'NONE',  ( 8.981834765181430313, 10.98821582489669169, 10.99387789255785997 ) ) ;
#4653 = B_SPLINE_CURVE_WITH_KNOTS ( 'NONE', 3,
 ( #1522, #7200, #19601, #4158, #10871, #1122 ),
 .UNSPECIFIED., .F., .F.,
 ( 4, 2, 4 ),
 ( 0.000000000000000000, 0.5000000000000000000, 1.000000000000000000 ),
 .UNSPECIFIED. ) ;
#4654 = B_SPLINE_CURVE_WITH_KNOTS ( 'NONE', 3,
 ( #25403, #31705, #28455, #7313, #26005, #1034, #38402, #9973, #25210, #22351, #34757, #16679, #4071, #6908, #37611, #7113, #7517, #22157 ),
 .UNSPECIFIED., .F., .F.,
 ( 4, 2, 2, 2, 2, 2, 2, 2, 4 ),
 ( 0.000000000000000000, 0.1249999999999999445, 0.2499999999999999445, 0.3749999999999999445, 0.4999999999999998890, 0.6249999999999997780, 0.7499999999999998890, 0.8749999999999998890, 1.000000000000000000 ),
 .UNSPECIFIED. ) ;
#4655 = VERTEX_POINT ( 'NONE', #3610 ) ;
#4656 = CARTESIAN_POINT ( 'NONE',  ( -30.56378389754250335, 0.1368832906204832112, -6.888355321334826087 ) ) ;
#4657 = ADVANCED_FACE ( 'NONE', ( #33906 ), #12952, .T. ) ;
#4658 = ORIENTED_EDGE ( 'NONE', *, *, #24570, .T. ) ;
#4659 = CARTESIAN_POINT ( 'NONE',  ( 33.99017495331719374, -9.144035213149372510, -9.360703722008313576 ) ) ;
#4660 = EDGE_CURVE ( 'NONE', #8524, #22764, #16983, .T. ) ;
#4661 = EDGE_LOOP ( 'NONE', ( #20499, #36912, #28846, #12553 ) ) ;
#4662 = AXIS2_PLACEMENT_3D ( 'NONE', #32076, #3446, #4244 ) ;
#4663 = ORIENTED_EDGE ( 'NONE', *, *, #25063, .F. ) ;
#4664 = DIRECTION ( 'NONE',  ( -0.7071067811865521247, 0.000000000000000000, -0.7071067811865430208 ) ) ;
#4665 = DIRECTION ( 'NONE',  ( 0.000000000000000000, 0.000000000000000000, -1.000000000000000000 ) ) ;
#4666 = CARTESIAN_POINT ( 'NONE',  ( -13.22866120779009336, 26.17694675929174153, 18.42518152272108622 ) ) ;
#4667 = EDGE_CURVE ( 'NONE', #24512, #10050, #37738, .T. ) ;
#4668 = CARTESIAN_POINT ( 'NONE',  ( -8.577547685840080760, 11.84256962714647798, 13.00000000000000178 ) ) ;
#4669 = ORIENTED_EDGE ( 'NONE', *, *, #12319, .T. ) ;
#4670 = CARTESIAN_POINT ( 'NONE',  ( -6.151085731882353969, 35.08626808545859888, 7.500000000000000888 ) ) ;
#4671 = DIRECTION ( 'NONE',  ( 0.000000000000000000, 0.000000000000000000, -1.000000000000000000 ) ) ;
#4672 = CARTESIAN_POINT ( 'NONE',  ( -32.33143948541797386, 1.358872982501903248, 11.00000000000000000 ) ) ;
#4673 = CARTESIAN_POINT ( 'NONE',  ( 18.55918025685463846, 17.91805357396305354, -6.442381077251955190 ) ) ;
#4674 = CARTESIAN_POINT ( 'NONE',  ( 10.59284826014176240, 33.08844111058793658, -8.954051444611645039 ) ) ;
#4675 = APPLICATION_CONTEXT ( 'automotive_design' ) ;
#4676 = VERTEX_POINT ( 'NONE', #24745 ) ;
#4677 = DIRECTION ( 'NONE',  ( 0.000000000000000000, 0.000000000000000000, 1.000000000000000000 ) ) ;
#4678 = CARTESIAN_POINT ( 'NONE',  ( 0.000000000000000000, 22.50000000000000355, 7.000000000000000000 ) ) ;
#4679 = CARTESIAN_POINT ( 'NONE',  ( 16.00895768845574096, -26.86996021029318626, -5.471689731333394313 ) ) ;
#4680 = DIRECTION ( 'NONE',  ( 1.000000000000000000, 0.000000000000000000, 0.000000000000000000 ) ) ;
#4681 = ADVANCED_FACE ( 'NONE', ( #28192 ), #29142, .T. ) ;
#4682 = DIRECTION ( 'NONE',  ( 0.000000000000000000, 0.000000000000000000, 1.000000000000000000 ) ) ;
#4683 = EDGE_CURVE ( 'NONE', #4972, #12781, #2712, .T. ) ;
#4684 = ORIENTED_EDGE ( 'NONE', *, *, #11757, .F. ) ;
#4685 = CARTESIAN_POINT ( 'NONE',  ( -10.97587534684186927, 17.31416389292776614, -29.34816979712976348 ) ) ;
#4686 = CARTESIAN_POINT ( 'NONE',  ( -30.37673449013114890, -23.61083502489086428, 15.72805884748940031 ) ) ;
#4687 = CARTESIAN_POINT ( 'NONE',  ( 14.33171430583705330, -25.57000458597046588, -10.18806973492949908 ) ) ;
#4688 = CIRCLE ( 'NONE', #9873, 18.00000000000000000 ) ;
#4689 = CARTESIAN_POINT ( 'NONE',  ( 24.58993327517434224, 16.11278406388105111, 7.499999999999996447 ) ) ;
#4690 = EDGE_LOOP ( 'NONE', ( #3098, #25683, #14065, #31716 ) ) ;
#4691 = VERTEX_POINT ( 'NONE', #27994 ) ;
#4692 = CARTESIAN_POINT ( 'NONE',  ( -11.80206329693653267, 32.84136598961480757, -7.211666007103653797 ) ) ;
#4693 = DIRECTION ( 'NONE',  ( 0.1045284632676569680, 0.9945218953682730678, 0.000000000000000000 ) ) ;
#4694 = FACE_BOUND ( 'NONE', #9684, .T. ) ;
#4695 = TOROIDAL_SURFACE ( 'NONE', #27398, 1.000000000000000000, 0.5000000000000000000 ) ;
#4696 = CARTESIAN_POINT ( 'NONE',  ( -29.01561123397027941, -6.266648261260574060, -14.93538031197087790 ) ) ;
#4697 = DIRECTION ( 'NONE',  ( -0.5000000000000039968, -0.8660254037844363761, 0.000000000000000000 ) ) ;
#4698 = ORIENTED_EDGE ( 'NONE', *, *, #21447, .F. ) ;
#4699 = CARTESIAN_POINT ( 'NONE',  ( 25.14345260446027552, 0.5055508715397122321, -17.45113365086313806 ) ) ;
#4700 = CARTESIAN_POINT ( 'NONE',  ( -10.75008043808887948, 32.97797437800713283, 10.49999999999999822 ) ) ;
#4701 = PLANE ( 'NONE',  #22594 ) ;
#4702 = CARTESIAN_POINT ( 'NONE',  ( -2.538198952020866539, 7.704401919100564378, 10.49999999999999822 ) ) ;
#4703 = UNCERTAINTY_MEASURE_WITH_UNIT (LENGTH_MEASURE( 1.000000000000000082E-05 ), #37207, 'distance_accuracy_value', 'NONE');
#4704 = ORIENTED_EDGE ( 'NONE', *, *, #22788, .T. ) ;
#4705 = CARTESIAN_POINT ( 'NONE',  ( -25.86155482627544444, 0.3215476971549391383, -16.44404694673128375 ) ) ;
#4706 = DIRECTION ( 'NONE',  ( 0.4067366430758010409, 0.9135454576426005335, -0.000000000000000000 ) ) ;
#4707 = EDGE_CURVE ( 'NONE', #17253, #39380, #30611, .T. ) ;
#4708 = ORIENTED_EDGE ( 'NONE', *, *, #6811, .F. ) ;
#4709 = CARTESIAN_POINT ( 'NONE',  ( 22.58427089344845129, -1.187563055018421299, -22.50445793986171950 ) ) ;
#4710 = CIRCLE ( 'NONE', #32611, 1.000000000000000000 ) ;
#4711 = CARTESIAN_POINT ( 'NONE',  ( 33.75286824399746166, -19.48722756659364919, 15.72805884748939498 ) ) ;
#4712 = EDGE_CURVE ( 'NONE', #4212, #23885, #37030, .T. ) ;
#4713 = ORIENTED_EDGE ( 'NONE', *, *, #27851, .T. ) ;
#4714 = CARTESIAN_POINT ( 'NONE',  ( -9.968062119478286576, 35.61660815598440166, 15.72805884748939853 ) ) ;
#4715 = CARTESIAN_POINT ( 'NONE',  ( -10.93513760491349274, -22.50092802249447033, 18.87996532025975327 ) ) ;
#4716 = CYLINDRICAL_SURFACE ( 'NONE', #24740, 0.4999999999999999445 ) ;
#4717 = CARTESIAN_POINT ( 'NONE',  ( -6.606256860318982405, 26.00827479057969072, 20.82122704794080548 ) ) ;
#4718 = CARTESIAN_POINT ( 'NONE',  ( -8.118377661053489902, 10.47536095541709322, 7.000000000000000000 ) ) ;
#4719 = ORIENTED_EDGE ( 'NONE', *, *, #39168, .F. ) ;
#4720 = CARTESIAN_POINT ( 'NONE',  ( -2.525645716490710679, 8.212903943950959018, 7.000000000000000000 ) ) ;
#4721 = CARTESIAN_POINT ( 'NONE',  ( 2.151556361536091089, 21.31112605819426165, -25.60121844493111709 ) ) ;
#4722 = VECTOR ( 'NONE', #20399, 1000.000000000000000 ) ;
#4723 = CARTESIAN_POINT ( 'NONE',  ( 5.947717410344610656, 34.62949535663720013, 10.50000000000000000 ) ) ;
#4724 = CARTESIAN_POINT ( 'NONE',  ( 21.05742987670727118, 12.15751280775815424, 16.87380292611441490 ) ) ;
#4725 = CARTESIAN_POINT ( 'NONE',  ( 22.01692992093476775, -27.08823313053303750, -5.451586861850059584 ) ) ;
#4726 = CARTESIAN_POINT ( 'NONE',  ( 14.06524961900339399, 27.71236540882591015, 7.500000000000000888 ) ) ;
#4727 = DIRECTION ( 'NONE',  ( -0.4999999999999921729, 0.8660254037844432595, 0.000000000000000000 ) ) ;
#4728 = DIRECTION ( 'NONE',  ( -0.6724985119639511622, 0.2185080122244150436, -0.7071067811865519026 ) ) ;
#4729 = EDGE_LOOP ( 'NONE', ( #24943, #31736, #35055, #4206 ) ) ;
#4730 = CARTESIAN_POINT ( 'NONE',  ( 14.97126155631352340, 26.12067504759210834, -9.230760338622234329 ) ) ;
#4731 = VERTEX_POINT ( 'NONE', #25145 ) ;
#4732 = CARTESIAN_POINT ( 'NONE',  ( -11.62347246686722357, 17.43168280077985699, -26.27056211956100285 ) ) ;
#4733 = CARTESIAN_POINT ( 'NONE',  ( -29.86387254395543778, -6.221772116353116111, 19.66345542862528717 ) ) ;
#4734 = CARTESIAN_POINT ( 'NONE',  ( -2.036571916123810055, 8.108948098542073879, 10.50000000000000355 ) ) ;
#4735 = CARTESIAN_POINT ( 'NONE',  ( 15.20036834786406565, 26.19538653648924864, -8.298372456229270000 ) ) ;
#4736 = VERTEX_POINT ( 'NONE', #12557 ) ;
#4737 = CARTESIAN_POINT ( 'NONE',  ( 28.26220087632740885, -17.92022017449335536, -12.89082178051953598 ) ) ;
#4738 = EDGE_CURVE ( 'NONE', #16076, #15620, #21895, .T. ) ;
#4739 = EDGE_LOOP ( 'NONE', ( #2342, #7493, #38067, #10112 ) ) ;
#4741 = CARTESIAN_POINT ( 'NONE',  ( -10.16521142134453548, 24.66068167190384841, 12.00000000000000000 ) ) ;
#4740 = CARTESIAN_POINT ( 'NONE',  ( -15.15816994429180120, 27.21337269842945972, -6.875229718665281986 ) ) ;
#4742 = CARTESIAN_POINT ( 'NONE',  ( -10.51723664951211923, -17.65706093263121090, -28.66670352760397833 ) ) ;
#4743 = DIRECTION ( 'NONE',  ( -0.3090169943749450643, 0.9510565162951544194, -0.000000000000000000 ) ) ;
#4744 = CIRCLE ( 'NONE', #13846, 15.99999999999999645 ) ;
#4745 = ORIENTED_EDGE ( 'NONE', *, *, #17376, .F. ) ;
#4746 = CARTESIAN_POINT ( 'NONE',  ( -20.79469271605055880, -9.355953883521966219, -23.01360647773964629 ) ) ;
#4747 = CARTESIAN_POINT ( 'NONE',  ( -9.088232624166426632, -18.50880257564897491, -28.10325226193693737 ) ) ;
#4748 = CARTESIAN_POINT ( 'NONE',  ( 38.66460482714355607, -17.32098561216399446, 22.99999999999999645 ) ) ;
#4749 = CARTESIAN_POINT ( 'NONE',  ( 15.52097626904955874, 19.85846508565274959, -14.68172677917668878 ) ) ;
#4750 = ORIENTED_EDGE ( 'NONE', *, *, #28240, .T. ) ;
#4751 = CARTESIAN_POINT ( 'NONE',  ( 20.09308256140095139, 4.507873197570775758, -28.22047126094187774 ) ) ;
#4752 = DIRECTION ( 'NONE',  ( 0.000000000000000000, 0.000000000000000000, 1.000000000000000000 ) ) ;
#4753 = AXIS2_PLACEMENT_3D ( 'NONE', #31957, #37853, #1289 ) ;
#4754 = DIRECTION ( 'NONE',  ( 1.000000000000000000, 0.000000000000000000, 0.000000000000000000 ) ) ;
#4755 = EDGE_LOOP ( 'NONE', ( #6573, #6456 ) ) ;
#4756 = CARTESIAN_POINT ( 'NONE',  ( -30.97995496863966380, -0.2256375777535584437, -6.412869061000700199 ) ) ;
#4757 = CARTESIAN_POINT ( 'NONE',  ( 30.06298335927989740, -0.4822708793880832734, -10.14075447114801420 ) ) ;
#4758 = VECTOR ( 'NONE', #31494, 1000.000000000000114 ) ;
#4759 = CARTESIAN_POINT ( 'NONE',  ( 28.09977684436853806, -21.02662082632513574, 18.87996532025785967 ) ) ;
#4760 = ORIENTED_EDGE ( 'NONE', *, *, #34932, .T. ) ;
#4761 = CARTESIAN_POINT ( 'NONE',  ( -28.27971916306745470, 2.627406427308467851, -6.898641429403003400 ) ) ;
#4762 = CARTESIAN_POINT ( 'NONE',  ( -19.69645987729884595, 11.37175641224114919, -21.56489709563623691 ) ) ;
#4763 = AXIS2_PLACEMENT_3D ( 'NONE', #21855, #12709, #18225 ) ;
#4764 = CARTESIAN_POINT ( 'NONE',  ( 10.78893975237932956, 23.27376113029817617, 12.00000000000000000 ) ) ;
#4765 = FACE_OUTER_BOUND ( 'NONE', #32845, .T. ) ;
#4766 = AXIS2_PLACEMENT_3D ( 'NONE', #20680, #38550, #14372 ) ;
#4767 = DIRECTION ( 'NONE',  ( -1.000000000000000000, 0.000000000000000000, 0.000000000000000000 ) ) ;
#4768 = CARTESIAN_POINT ( 'NONE',  ( -14.11133924723978161, 27.61078317377194224, 11.00000000000000000 ) ) ;
#4769 = DIRECTION ( 'NONE',  ( -0.2079116908177533474, 0.9781476007338067991, 0.000000000000000000 ) ) ;
#4770 = ORIENTED_EDGE ( 'NONE', *, *, #15113, .T. ) ;
#4771 = CARTESIAN_POINT ( 'NONE',  ( -22.69455887956607754, 5.944439957561778343, -16.84495653843570651 ) ) ;
#4772 = CARTESIAN_POINT ( 'NONE',  ( -0.5000000000000004441, 32.50000000000000000, 10.00000000000000000 ) ) ;
#4773 = CARTESIAN_POINT ( 'NONE',  ( -0.9999999999999993339, 33.00000000000000000, 10.50000000000000000 ) ) ;
#4774 = CARTESIAN_POINT ( 'NONE',  ( 27.89879264781504276, -24.25791139881312120, -7.574806088488642786 ) ) ;
#4775 = DIRECTION ( 'NONE',  ( 1.000000000000000000, 0.000000000000000000, 0.000000000000000000 ) ) ;
#4776 = CARTESIAN_POINT ( 'NONE',  ( 5.440908595777814050, 35.94977745735560859, 7.500000000000000888 ) ) ;
#4777 = CARTESIAN_POINT ( 'NONE',  ( 12.67051716736391498, 22.07145339077409929, -17.38087975008689057 ) ) ;
#4778 = VERTEX_POINT ( 'NONE', #34298 ) ;
#4779 = CIRCLE ( 'NONE', #9970, 1.000000000000000888 ) ;
#4780 = CARTESIAN_POINT ( 'NONE',  ( -17.53063491166886578, 19.28413246547140503, -9.334923713665935097 ) ) ;
#4781 = CARTESIAN_POINT ( 'NONE',  ( -24.96922908923108508, -9.289876063515562166, 21.00000000000004619 ) ) ;
#4782 = ADVANCED_FACE ( 'NONE', ( #2816 ), #15210, .T. ) ;
#4783 = CARTESIAN_POINT ( 'NONE',  ( 9.439680310844765998, -18.19733056428809803, -29.34954212647691563 ) ) ;
#4784 = FACE_OUTER_BOUND ( 'NONE', #11902, .T. ) ;
#4785 = CARTESIAN_POINT ( 'NONE',  ( 15.11232028572299946, 26.10242263575024424, -8.767989562428970984 ) ) ;
#4786 = EDGE_LOOP ( 'NONE', ( #3221, #29275, #15404, #36512 ) ) ;
#4787 = CARTESIAN_POINT ( 'NONE',  ( 15.33430753556601722, 26.63135885691745486, -6.887879096180697047 ) ) ;
#4788 = ORIENTED_EDGE ( 'NONE', *, *, #11668, .T. ) ;
#4790 = CARTESIAN_POINT ( 'NONE',  ( -14.97009266215794021, 21.42933399866948463, 11.00000000000000000 ) ) ;
#4789 = CARTESIAN_POINT ( 'NONE',  ( -12.09709384379045005, 19.96450846454217043, -20.53406412358028277 ) ) ;
#4791 = CARTESIAN_POINT ( 'NONE',  ( -14.96743987807556842, -25.98747055160875874, -9.238933126925131134 ) ) ;
#4792 = CARTESIAN_POINT ( 'NONE',  ( -37.09709568333396845, -7.051483854460184553, 10.99999999999968026 ) ) ;
#4793 = CARTESIAN_POINT ( 'NONE',  ( -32.07387720787730956, -20.72040958422635981, -6.698075182882634593 ) ) ;
#4794 = AXIS2_PLACEMENT_3D ( 'NONE', #25889, #38289, #14512 ) ;
#4795 = CARTESIAN_POINT ( 'NONE',  ( -4.727911438284216672, -20.01714751873747744, -28.25398441486722589 ) ) ;
#4796 = CARTESIAN_POINT ( 'NONE',  ( 11.60051960103743873, 17.04428010164728136, -28.10970223773723120 ) ) ;
#4797 = ADVANCED_FACE ( 'NONE', ( #21500 ), #18462, .F. ) ;
#4798 = VERTEX_POINT ( 'NONE', #10107 ) ;
#4799 = CARTESIAN_POINT ( 'NONE',  ( 19.95678360488982861, 7.462870846925651058, -23.27266411727370254 ) ) ;
#4800 = LINE ( 'NONE', #1151, #1158 ) ;
#4801 = CARTESIAN_POINT ( 'NONE',  ( -12.30264615366000491, 13.91750221598363346, 7.102637441331451029 ) ) ;
#4802 = ADVANCED_FACE ( 'NONE', ( #7451 ), #38744, .F. ) ;
#4803 = CARTESIAN_POINT ( 'NONE',  ( -8.007761790012255076, 9.776959832083379709, 11.00000000000000000 ) ) ;
#4804 = EDGE_LOOP ( 'NONE', ( #13605, #24050, #2645, #25143 ) ) ;
#4805 = CARTESIAN_POINT ( 'NONE',  ( -22.00238895739720490, -1.313321433655290971, -23.60997353844526359 ) ) ;
#4806 = VECTOR ( 'NONE', #39449, 999.9999999999998863 ) ;
#4807 = CARTESIAN_POINT ( 'NONE',  ( -7.205739717619530360, 18.19477196585663137, 20.99999999999999645 ) ) ;
#4808 = CARTESIAN_POINT ( 'NONE',  ( 23.43324262027548599, -8.134040356058102716, 20.99999999999999645 ) ) ;
#4809 = CARTESIAN_POINT ( 'NONE',  ( -24.56921341014758653, -25.93758952935236906, -7.617217473784200443 ) ) ;
#4810 = CARTESIAN_POINT ( 'NONE',  ( 0.9819609608163288872, 14.62372257652092422, 13.00000000000000178 ) ) ;
#4811 = CARTESIAN_POINT ( 'NONE',  ( 22.27145313233416957, -10.58722233873939444, -20.70863184773896037 ) ) ;
#4812 = CARTESIAN_POINT ( 'NONE',  ( 35.68447701591248489, -3.401722300707758162, 11.00000000000000000 ) ) ;
#4813 = AXIS2_PLACEMENT_3D ( 'NONE', #22690, #16609, #20467 ) ;
#4814 = EDGE_CURVE ( 'NONE', #35744, #14392, #35747, .T. ) ;
#4815 = ORIENTED_EDGE ( 'NONE', *, *, #39284, .F. ) ;
#4816 = EDGE_CURVE ( 'NONE', #21531, #22937, #764, .T. ) ;
#4817 = DIRECTION ( 'NONE',  ( -0.4999999999999920619, 0.8660254037844433705, 0.000000000000000000 ) ) ;
#4818 = CARTESIAN_POINT ( 'NONE',  ( 6.354454053420414361, 35.54304081427980577, 11.00000000000000000 ) ) ;
#4819 = EDGE_LOOP ( 'NONE', ( #12199, #8147, #21082, #23738 ) ) ;
#4820 = VECTOR ( 'NONE', #22495, 1000.000000000000000 ) ;
#4821 = CARTESIAN_POINT ( 'NONE',  ( 0.2168302826061950517, 20.49890265953407109, -30.00000000000000711 ) ) ;
#4822 = FACE_OUTER_BOUND ( 'NONE', #32447, .T. ) ;
#4823 = CARTESIAN_POINT ( 'NONE',  ( 3.587660364795204782, 9.681887955242936883, 13.00000000000000178 ) ) ;
#4824 = CARTESIAN_POINT ( 'NONE',  ( -17.34253826592568970, 27.32041144456614390, -5.000000000000000000 ) ) ;
#4825 = CARTESIAN_POINT ( 'NONE',  ( 12.53339520833710985, 14.68649063341690564, 10.94611345180490680 ) ) ;
#4826 = CARTESIAN_POINT ( 'NONE',  ( 0.000000000000000000, 22.50000000000000355, 7.000000000000000000 ) ) ;
#4827 = CARTESIAN_POINT ( 'NONE',  ( 14.11763978891951687, 27.49014883721196156, -10.07373652601078007 ) ) ;
#4828 = CARTESIAN_POINT ( 'NONE',  ( 22.38266491662918156, 24.02827644978115984, 10.00000000000000000 ) ) ;
#4829 = VERTEX_POINT ( 'NONE', #35499 ) ;
#4831 = LINE ( 'NONE', #17442, #38887 ) ;
#4830 = CARTESIAN_POINT ( 'NONE',  ( -18.80845520939411486, 12.28582799405812587, -18.01515471683427450 ) ) ;
#4832 = FACE_OUTER_BOUND ( 'NONE', #58, .T. ) ;
#4833 = CARTESIAN_POINT ( 'NONE',  ( 9.514046198846664026, -18.15855281542499000, -29.34801595497529547 ) ) ;
#4834 = CARTESIAN_POINT ( 'NONE',  ( -1.623738443162547007, 19.56555719779890978, 13.00000000000000178 ) ) ;
#4835 = CARTESIAN_POINT ( 'NONE',  ( 11.86360577746352973, 19.41276117560862957, -21.61155111211224877 ) ) ;
#4836 = CARTESIAN_POINT ( 'NONE',  ( -30.41237130417910706, 3.314011747244096195, -5.000000000000000000 ) ) ;
#4837 = EDGE_CURVE ( 'NONE', #2755, #36470, #14306, .T. ) ;
#4838 = DIRECTION ( 'NONE',  ( -0.9135454576426059736, -0.4067366430757888285, 0.000000000000000000 ) ) ;
#4839 = CARTESIAN_POINT ( 'NONE',  ( -21.40755417942576244, -20.13335966822008061, -15.79869096137255546 ) ) ;
#4840 = CARTESIAN_POINT ( 'NONE',  ( 3.865693630706900308, -24.30145578791679029, -10.37003140332352480 ) ) ;
#4841 = CARTESIAN_POINT ( 'NONE',  ( 15.46458721040396078, 26.18010667664744417, -6.888852476684097503 ) ) ;
#4842 = CARTESIAN_POINT ( 'NONE',  ( 17.84088086924548122, 11.87538515410224527, -22.23966607540548068 ) ) ;
#4843 = DIRECTION ( 'NONE',  ( -0.8090169943749426773, 0.5877852522924796874, -0.000000000000000000 ) ) ;
#4844 = ORIENTED_EDGE ( 'NONE', *, *, #15955, .F. ) ;
#4845 = CARTESIAN_POINT ( 'NONE',  ( -6.380476842507320612, 37.12010437673579588, -5.863956392860120381 ) ) ;
#4846 = ORIENTED_EDGE ( 'NONE', *, *, #8910, .T. ) ;
#4847 = CARTESIAN_POINT ( 'NONE',  ( 5.397160494303298250, 36.49555269156554260, 7.455686640544908705 ) ) ;
#4848 = ORIENTED_EDGE ( 'NONE', *, *, #29746, .T. ) ;
#4849 = DIRECTION ( 'NONE',  ( 0.8660254037844362651, -0.5000000000000041078, -3.469446951953615767E-15 ) ) ;
#4850 = CARTESIAN_POINT ( 'NONE',  ( -8.271785691010729025, 10.26421291652884449, 10.94611345180490147 ) ) ;
#4851 = VERTEX_POINT ( 'NONE', #16208 ) ;
#4852 = CARTESIAN_POINT ( 'NONE',  ( -29.79950855980051827, 0.2397400637421467640, -9.241859429830270756 ) ) ;
#4853 = ORIENTED_EDGE ( 'NONE', *, *, #9315, .F. ) ;
#4854 = CARTESIAN_POINT ( 'NONE',  ( 35.47190708691255168, -11.90251233358380212, -5.000000000000003553 ) ) ;
#4855 = ORIENTED_EDGE ( 'NONE', *, *, #6989, .T. ) ;
#4856 = CYLINDRICAL_SURFACE ( 'NONE', #9602, 1.000000000000000000 ) ;
#4857 = EDGE_LOOP ( 'NONE', ( #3094, #10835, #17762 ) ) ;
#4858 = EDGE_CURVE ( 'NONE', #19220, #2217, #4616, .T. ) ;
#4859 = CYLINDRICAL_SURFACE ( 'NONE', #13205, 0.5000000000000024425 ) ;
#4860 = AXIS2_PLACEMENT_3D ( 'NONE', #23059, #19610, #26519 ) ;
#4861 = DIRECTION ( 'NONE',  ( 0.1045284632676436593, -0.9945218953682742891, 0.000000000000000000 ) ) ;
#4862 = CARTESIAN_POINT ( 'NONE',  ( -9.991731067009840928, 30.98181186424739408, 18.87996532025781704 ) ) ;
#4863 = CIRCLE ( 'NONE', #9418, 1.000000000000000000 ) ;
#4864 = CARTESIAN_POINT ( 'NONE',  ( 8.593266739736568738, 16.38397459621552699, 10.50000000000000000 ) ) ;
#4865 = ORIENTED_EDGE ( 'NONE', *, *, #2893, .T. ) ;
#4866 = CARTESIAN_POINT ( 'NONE',  ( -4.727507481117087629, 31.88885898370948269, 11.00000000000000000 ) ) ;
#4867 = CYLINDRICAL_SURFACE ( 'NONE', #18285, 0.5000000000000004441 ) ;
#4868 = LINE ( 'NONE', #17282, #37031 ) ;
#4869 = CARTESIAN_POINT ( 'NONE',  ( 18.17512370925090792, 17.42502396823083899, -10.34031744549918308 ) ) ;
#4870 = CARTESIAN_POINT ( 'NONE',  ( 5.926286245021443300, 20.46757980983786851, -25.76132644253925719 ) ) ;
#4871 = VERTEX_POINT ( 'NONE', #28994 ) ;
#4872 = DIRECTION ( 'NONE',  ( 1.000000000000000000, 0.000000000000000000, 0.000000000000000000 ) ) ;
#4873 = DIRECTION ( 'NONE',  ( 0.000000000000000000, 0.000000000000000000, 1.000000000000000000 ) ) ;
#4874 = B_SPLINE_CURVE_WITH_KNOTS ( 'NONE', 3,
 ( #26550, #20054, #20460, #11111, #19143, #31141, #22377, #28483, #37637, #9406, #2907, #28286, #27686, #21786, #31535, #16098, #37036, #12448 ),
 .UNSPECIFIED., .F., .F.,
 ( 4, 2, 2, 2, 2, 2, 2, 2, 4 ),
 ( 0.000000000000000000, 0.1250000000000000000, 0.2500000000000000000, 0.3750000000000000000, 0.5000000000000000000, 0.6250000000000000000, 0.7500000000000000000, 0.8750000000000000000, 1.000000000000000000 ),
 .UNSPECIFIED. ) ;
#4875 = CARTESIAN_POINT ( 'NONE',  ( 15.76324282396835486, -26.51440755082071732, -7.811281871053155967 ) ) ;
#4876 = CARTESIAN_POINT ( 'NONE',  ( 16.05557028316289703, -24.54483004364954368, 18.42518152272108978 ) ) ;
#4877 = B_SPLINE_CURVE_WITH_KNOTS ( 'NONE', 3,
 ( #23107, #25747, #25545, #4624, #19653, #35506 ),
 .UNSPECIFIED., .F., .F.,
 ( 4, 2, 4 ),
 ( 0.000000000000000000, 0.5000000000000000000, 1.000000000000000000 ),
 .UNSPECIFIED. ) ;
#4878 = CARTESIAN_POINT ( 'NONE',  ( 13.46929972531963848, 26.35070966310165375, 7.500000000000000000 ) ) ;
#4879 = ADVANCED_FACE ( 'NONE', ( #38338 ), #26142, .F. ) ;
#4880 = CIRCLE ( 'NONE', #10713, 16.00000000000000000 ) ;
#4881 = ORIENTED_EDGE ( 'NONE', *, *, #4352, .T. ) ;
#4882 = CARTESIAN_POINT ( 'NONE',  ( -12.13347509736119889, 19.92089084820641176, -20.54147204449933994 ) ) ;
#4883 = CARTESIAN_POINT ( 'NONE',  ( -34.59909889755191159, -19.97579906222007295, 13.92931973827808534 ) ) ;
#4884 = CARTESIAN_POINT ( 'NONE',  ( 12.18486585843677972, -23.95081470295607318, -13.58225421544179667 ) ) ;
#4885 = ADVANCED_FACE ( 'NONE', ( #23306 ), #34894, .T. ) ;
#4886 = EDGE_CURVE ( 'NONE', #17473, #5105, #1367, .T. ) ;
#4887 = FACE_OUTER_BOUND ( 'NONE', #1160, .T. ) ;
#4888 = EDGE_LOOP ( 'NONE', ( #3087, #15606, #21210 ) ) ;
#4889 = EDGE_LOOP ( 'NONE', ( #28303, #36699 ) ) ;
#4890 = CARTESIAN_POINT ( 'NONE',  ( -12.29079644195909005, 31.26159447669306246, -9.015097560565573431 ) ) ;
#4891 = VECTOR ( 'NONE', #15322, 1000.000000000000114 ) ;
#4892 = CARTESIAN_POINT ( 'NONE',  ( 10.73859285986296541, 31.49625607628530588, 7.499999999999996447 ) ) ;
#4893 = FACE_BOUND ( 'NONE', #36289, .T. ) ;
#4894 = CIRCLE ( 'NONE', #37344, 0.5000000000000004441 ) ;
#4895 = EDGE_CURVE ( 'NONE', #5646, #860, #7001, .T. ) ;
#4897 = VECTOR ( 'NONE', #31475, 1000.000000000000114 ) ;
#4896 = CARTESIAN_POINT ( 'NONE',  ( -28.69299338070981875, -4.470963161381146911, -15.02617031471227627 ) ) ;
#4898 = CARTESIAN_POINT ( 'NONE',  ( 18.00000000000000000, 22.50000000000000711, 11.00000000000000178 ) ) ;
#4899 = ORIENTED_EDGE ( 'NONE', *, *, #18324, .T. ) ;
#4900 = CARTESIAN_POINT ( 'NONE',  ( 29.91352946887046826, 0.1146846962358806787, -9.239818586298255809 ) ) ;
#4901 = CARTESIAN_POINT ( 'NONE',  ( -10.58109189495859326, 32.70007430011122551, 10.96580508970283141 ) ) ;
#4902 = DIRECTION ( 'NONE',  ( 0.4999999999999933942, -0.8660254037844425934, 0.000000000000000000 ) ) ;
#4903 = CARTESIAN_POINT ( 'NONE',  ( -2.231660708550785799, 7.803782283739876036, 10.49999999999999822 ) ) ;
#4904 = ORIENTED_EDGE ( 'NONE', *, *, #19699, .T. ) ;
#4905 = CARTESIAN_POINT ( 'NONE',  ( -23.31796685322062501, 0.5495358244031924855, -20.54176272741512221 ) ) ;
#4906 = CARTESIAN_POINT ( 'NONE',  ( 22.37674264578617667, 24.85189042352198641, 7.000000000000000000 ) ) ;
#4907 = ORIENTED_EDGE ( 'NONE', *, *, #31190, .T. ) ;
#4908 = CARTESIAN_POINT ( 'NONE',  ( 32.78999465087354537, -4.002307633261452224, -9.046564716739682765 ) ) ;
#4909 = CARTESIAN_POINT ( 'NONE',  ( 18.88617201209933683, -28.19481557848324726, 15.13084544680231502 ) ) ;
#4910 = ORIENTED_EDGE ( 'NONE', *, *, #3818, .F. ) ;
#4911 = CARTESIAN_POINT ( 'NONE',  ( -1.888379873391735186, 39.95159812444025249, 13.92931973827808534 ) ) ;
#4912 = EDGE_CURVE ( 'NONE', #31959, #18376, #7246, .T. ) ;
#4913 = CARTESIAN_POINT ( 'NONE',  ( 16.05557028316878387, -24.54483004365089371, 18.42518152272108978 ) ) ;
#4914 = ADVANCED_FACE ( 'NONE', ( #16611 ), #13550, .T. ) ;
#4915 = LINE ( 'NONE', #11214, #13046 ) ;
#4916 = EDGE_CURVE ( 'NONE', #21094, #3673, #31186, .T. ) ;
#4917 = CARTESIAN_POINT ( 'NONE',  ( 0.9851783940329167377, 31.60047892813805248, 20.50957957746028626 ) ) ;
#4918 = DIRECTION ( 'NONE',  ( 1.000000000000000000, 0.000000000000000000, 0.000000000000000000 ) ) ;
#4919 = EDGE_LOOP ( 'NONE', ( #19898, #39272, #17299, #35275 ) ) ;
#4920 = DIRECTION ( 'NONE',  ( 0.000000000000000000, 0.000000000000000000, 1.000000000000000000 ) ) ;
#4921 = AXIS2_PLACEMENT_3D ( 'NONE', #13465, #3922, #19564 ) ;
#4922 = AXIS2_PLACEMENT_3D ( 'NONE', #23321, #35305, #29210 ) ;
#4923 = CARTESIAN_POINT ( 'NONE',  ( 2.065624757052793914, 20.48161944704045823, -28.45443914133164753 ) ) ;
#4924 = AXIS2_PLACEMENT_3D ( 'NONE', #9695, #540, #6618 ) ;
#4925 = CARTESIAN_POINT ( 'NONE',  ( 2.256323172317815207, 14.28970123917151192, 9.000000000000001776 ) ) ;
#4926 = CARTESIAN_POINT ( 'NONE',  ( 6.462764152049920163, 17.91932574229958419, 20.99999999999999645 ) ) ;
#4927 = CIRCLE ( 'NONE', #1042, 1.000000000000000888 ) ;
#4928 = CARTESIAN_POINT ( 'NONE',  ( 19.11282184975060972, -26.40045450798872295, -9.072278811920540420 ) ) ;
#4929 = CARTESIAN_POINT ( 'NONE',  ( -12.64211604268330724, 20.79918788657763429, 12.00000000000000000 ) ) ;
#4930 = DIRECTION ( 'NONE',  ( -0.6691306063588671194, -0.7431448254773861395, 0.000000000000000000 ) ) ;
#4931 = CARTESIAN_POINT ( 'NONE',  ( 2.485571585149743523, -11.24999999999995737, 10.00000000000000000 ) ) ;
#4932 = EDGE_LOOP ( 'NONE', ( #4910, #36188, #32120, #16272 ) ) ;
#4933 = EDGE_CURVE ( 'NONE', #3614, #6055, #5766, .T. ) ;
#4934 = CARTESIAN_POINT ( 'NONE',  ( 15.30043618030332553, 26.74953473181076902, -6.885117079756076564 ) ) ;
#4935 = ORIENTED_EDGE ( 'NONE', *, *, #37681, .T. ) ;
#4936 = CARTESIAN_POINT ( 'NONE',  ( -12.10739415485800841, 18.50350219561722653, -22.80206802353507101 ) ) ;
#4937 = CARTESIAN_POINT ( 'NONE',  ( -20.32014898129551739, -22.75198622026924511, 19.66345542862528717 ) ) ;
#4938 = EDGE_CURVE ( 'NONE', #888, #39039, #9781, .T. ) ;
#4939 = DIRECTION ( 'NONE',  ( 1.000000000000000000, 0.000000000000000000, 0.000000000000000000 ) ) ;
#4940 = CARTESIAN_POINT ( 'NONE',  ( 11.11640272627978021, 17.47322625280633801, -27.45115658143717141 ) ) ;
#4941 = ORIENTED_EDGE ( 'NONE', *, *, #12213, .T. ) ;
#4942 = CARTESIAN_POINT ( 'NONE',  ( 32.02639718292716964, -18.95205052879796526, -8.842390373194950470 ) ) ;
#4943 = ORIENTED_EDGE ( 'NONE', *, *, #27945, .T. ) ;
#4945 = CARTESIAN_POINT ( 'NONE',  ( 5.198706521309295780, 29.65540566576566661, 9.000000000000001776 ) ) ;
#4944 = CARTESIAN_POINT ( 'NONE',  ( -12.13084903553365557, 20.83183464748637093, -19.44244853017589492 ) ) ;
#4946 = CARTESIAN_POINT ( 'NONE',  ( -16.83103474447717574, -26.46333433132708279, -8.697577348884802717 ) ) ;
#4947 = DIRECTION ( 'NONE',  ( 0.000000000000000000, 0.000000000000000000, 1.000000000000000000 ) ) ;
#4948 = ORIENTED_EDGE ( 'NONE', *, *, #9412, .F. ) ;
#4949 = CARTESIAN_POINT ( 'NONE',  ( -18.77890958615538608, -8.456140786848550306, -28.45356751116922567 ) ) ;
#4950 = CARTESIAN_POINT ( 'NONE',  ( -14.98552525403816205, -26.61491965241963342, -5.000000000000000888 ) ) ;
#4951 = DIRECTION ( 'NONE',  ( -0.000000000000000000, -0.000000000000000000, 1.000000000000000000 ) ) ;
#4952 = CARTESIAN_POINT ( 'NONE',  ( 16.61617810080481661, 21.74609680309975346, -8.817940406396488129 ) ) ;
#4953 = ORIENTED_EDGE ( 'NONE', *, *, #11067, .T. ) ;
#4954 = CARTESIAN_POINT ( 'NONE',  ( 29.78831017271203763, 1.106291696078458120, -4.999999999999999112 ) ) ;
#4955 = CARTESIAN_POINT ( 'NONE',  ( -8.347978306607240384, 10.15934277794837293, 10.82238861112331740 ) ) ;
#4956 = CARTESIAN_POINT ( 'NONE',  ( -14.48927117870124093, -30.61587158504648443, 22.99999999999999289 ) ) ;
#4957 = VECTOR ( 'NONE', #32535, 1000.000000000000000 ) ;
#4958 = ORIENTED_EDGE ( 'NONE', *, *, #25517, .F. ) ;
#4959 = CARTESIAN_POINT ( 'NONE',  ( -20.83595133204223515, 0.5720877597900050349, -26.81050348232703229 ) ) ;
#4960 = CARTESIAN_POINT ( 'NONE',  ( 27.63112615685908935, -0.4701152805647206279, -14.39745280081397283 ) ) ;
#4961 = CIRCLE ( 'NONE', #38035, 0.5000000000000004441 ) ;
#4962 = CARTESIAN_POINT ( 'NONE',  ( 32.23453252384990719, -8.210301902000198382, 18.87996532025784191 ) ) ;
#4963 = VECTOR ( 'NONE', #24081, 1000.000000000000000 ) ;
#4964 = ORIENTED_EDGE ( 'NONE', *, *, #29902, .T. ) ;
#4965 = CARTESIAN_POINT ( 'NONE',  ( -25.48370164714067343, 1.883020324448871463, -15.57262912828922552 ) ) ;
#4966 = CARTESIAN_POINT ( 'NONE',  ( 16.84920187454417828, 29.09530251867925443, -13.79123840944734880 ) ) ;
#4967 = PLANE ( 'NONE',  #32990 ) ;
#4968 = DIRECTION ( 'NONE',  ( 1.000000000000000000, 0.000000000000000000, 0.000000000000000000 ) ) ;
#4969 = CYLINDRICAL_SURFACE ( 'NONE', #3271, 18.00000000000002487 ) ;
#4970 = CARTESIAN_POINT ( 'NONE',  ( 2.421689871081641687, 8.701977744317826335, 9.500000000000000000 ) ) ;
#4971 = DIRECTION ( 'NONE',  ( 0.000000000000000000, 0.000000000000000000, 1.000000000000000000 ) ) ;
#4972 = VERTEX_POINT ( 'NONE', #30756 ) ;
#4973 = CARTESIAN_POINT ( 'NONE',  ( -25.21997133566067006, 6.187216884184454813, -8.370264087233126205 ) ) ;
#4974 = DIRECTION ( 'NONE',  ( 0.000000000000000000, 0.000000000000000000, 1.000000000000000000 ) ) ;
#4975 = FACE_OUTER_BOUND ( 'NONE', #21712, .T. ) ;
#4976 = CARTESIAN_POINT ( 'NONE',  ( 26.14537312525837010, -25.55590668144287747, -6.734860050313713487 ) ) ;
#4977 = CARTESIAN_POINT ( 'NONE',  ( 7.064564986133971658, 13.54338174056915456, 12.00000000000000000 ) ) ;
#4978 = CARTESIAN_POINT ( 'NONE',  ( -14.66655470856257182, 20.08105443166860127, 10.49999999999999822 ) ) ;
#4979 = CARTESIAN_POINT ( 'NONE',  ( 15.11844294575625014, 26.78304985304260555, -7.815403913362212407 ) ) ;
#4980 = AXIS2_PLACEMENT_3D ( 'NONE', #33745, #33543, #3044 ) ;
#4981 = FACE_OUTER_BOUND ( 'NONE', #2852, .T. ) ;
#4982 = ORIENTED_EDGE ( 'NONE', *, *, #11891, .T. ) ;
#4983 = CARTESIAN_POINT ( 'NONE',  ( -16.89125701550774394, 21.69970515213497109, -7.382923725449230368 ) ) ;
#4984 = DIRECTION ( 'NONE',  ( 0.3090169943749465631, -0.9510565162951538642, 0.000000000000000000 ) ) ;
#4985 = CARTESIAN_POINT ( 'NONE',  ( 11.13486383234526400, -20.47745619191486099, -20.54734414695593259 ) ) ;
#4986 = CARTESIAN_POINT ( 'NONE',  ( -13.05736835487441994, 16.11602540378456183, 7.499999999999993783 ) ) ;
#4987 = CARTESIAN_POINT ( 'NONE',  ( 12.94181704842254454, 21.63114967576204961, -17.44000072231445486 ) ) ;
#4988 = VERTEX_POINT ( 'NONE', #15513 ) ;
#4989 = CARTESIAN_POINT ( 'NONE',  ( 11.12160456634176953, 17.61533166272543482, -26.83009323505504184 ) ) ;
#4990 = ORIENTED_EDGE ( 'NONE', *, *, #37543, .F. ) ;
#4992 = DIRECTION ( 'NONE',  ( 0.000000000000000000, 0.000000000000000000, 1.000000000000000000 ) ) ;
#4991 = CARTESIAN_POINT ( 'NONE',  ( -11.05928181430064861, 17.65851141523520340, -26.82422181314475296 ) ) ;
#4993 = CARTESIAN_POINT ( 'NONE',  ( -11.19645373508086195, -20.46641504268867351, -20.53998934932196363 ) ) ;
#4994 = CARTESIAN_POINT ( 'NONE',  ( -28.24711154207075481, -27.09388640670391979, 11.00000000000006573 ) ) ;
#4995 = CARTESIAN_POINT ( 'NONE',  ( -32.24083685196362836, -20.82486095561948503, -5.856421537953417911 ) ) ;
#4996 = CARTESIAN_POINT ( 'NONE',  ( -6.503947451768620880, -20.28793242900468385, -24.22034738830593881 ) ) ;
#4997 = CARTESIAN_POINT ( 'NONE',  ( 15.80018706099420633, 25.22022683934922682, -6.419152679462878375 ) ) ;
#4998 = ORIENTED_EDGE ( 'NONE', *, *, #13100, .F. ) ;
#4999 = CARTESIAN_POINT ( 'NONE',  ( 22.54818472930890039, 7.997166754206832096, -13.85798304266238645 ) ) ;
#5000 = CYLINDRICAL_SURFACE ( 'NONE', #23854, 0.5000000000000004441 ) ;
#5001 = LINE ( 'NONE', #8247, #36135 ) ;
#5002 = FACE_OUTER_BOUND ( 'NONE', #23601, .T. ) ;
#5003 = VERTEX_POINT ( 'NONE', #27304 ) ;
#5004 = CARTESIAN_POINT ( 'NONE',  ( -23.24856704062857915, -1.463813097875870550, -21.34811639290027685 ) ) ;
#5005 = CARTESIAN_POINT ( 'NONE',  ( -20.63240589125325641, -1.802217369530700442, 20.82122704794238999 ) ) ;
#5006 = CARTESIAN_POINT ( 'NONE',  ( 25.16128423893353627, -12.39270898182871328, 20.99999999999999645 ) ) ;
#5007 = DIRECTION ( 'NONE',  ( 0.000000000000000000, -0.000000000000000000, 1.000000000000000000 ) ) ;
#5008 = CARTESIAN_POINT ( 'NONE',  ( -14.45538749008468038, 26.50521816028845734, 7.489440493383480835 ) ) ;
#5009 = CARTESIAN_POINT ( 'NONE',  ( 32.33143948541781043, 1.358872982501757143, 11.55979286843934872 ) ) ;
#5010 = AXIS2_PLACEMENT_3D ( 'NONE', #31976, #20198, #28927 ) ;
#5011 = VECTOR ( 'NONE', #31034, 1000.000000000000114 ) ;
#5012 = EDGE_CURVE ( 'NONE', #20519, #15902, #20814, .T. ) ;
#5013 = ORIENTED_EDGE ( 'NONE', *, *, #571, .T. ) ;
#5014 = DIRECTION ( 'NONE',  ( 0.000000000000000000, 0.000000000000000000, 1.000000000000000000 ) ) ;
#5015 = CIRCLE ( 'NONE', #27714, 1.000000000000000000 ) ;
#5016 = VECTOR ( 'NONE', #7409, 1000.000000000000114 ) ;
#5017 = CARTESIAN_POINT ( 'NONE',  ( 16.38619327006176718, 7.072988944186808347, 11.00000000000000000 ) ) ;
#5018 = LINE ( 'NONE', #17429, #13189 ) ;
#5019 = EDGE_CURVE ( 'NONE', #7705, #26791, #27896, .T. ) ;
#5020 = CARTESIAN_POINT ( 'NONE',  ( 0.2168302826061956068, 20.49890265953407109, -29.21218655438333656 ) ) ;
#5021 = DIRECTION ( 'NONE',  ( 0.5877852522924796874, 0.8090169943749426773, -0.000000000000000000 ) ) ;
#5022 = CARTESIAN_POINT ( 'NONE',  ( 8.411683849014126579, 19.76687823897103868, 9.000000000000001776 ) ) ;
#5023 = EDGE_CURVE ( 'NONE', #19849, #1872, #39691, .T. ) ;
#5024 = CARTESIAN_POINT ( 'NONE',  ( -5.947717410344452560, 34.62949535663727829, 7.000000000000000000 ) ) ;
#5025 = CARTESIAN_POINT ( 'NONE',  ( 11.94134295108989896, 16.18301270189217433, 10.50000000000000000 ) ) ;
#5026 = CARTESIAN_POINT ( 'NONE',  ( 9.427394962683440127, 11.06314620782477753, 10.49999999999999822 ) ) ;
#5027 = CARTESIAN_POINT ( 'NONE',  ( 11.97830265401803729, 21.99462655053814331, -18.31500106451969856 ) ) ;
#5028 = CARTESIAN_POINT ( 'NONE',  ( -6.572794801194226544, 16.58182897866500127, 7.000000000000000000 ) ) ;
#5029 = ORIENTED_EDGE ( 'NONE', *, *, #29518, .T. ) ;
#5031 = DIRECTION ( 'NONE',  ( 1.000000000000000000, 0.000000000000000000, 0.000000000000000000 ) ) ;
#5030 = CARTESIAN_POINT ( 'NONE',  ( -19.40296131254754641, 15.36279795482867883, -9.381991658370749221 ) ) ;
#5032 = CARTESIAN_POINT ( 'NONE',  ( -9.831584923911588447, 26.22020669908463830, 11.00000000000000000 ) ) ;
#5033 = CARTESIAN_POINT ( 'NONE',  ( 9.815459356401843749, -18.55056478758831062, -26.22197369305180459 ) ) ;
#5034 = CARTESIAN_POINT ( 'NONE',  ( -19.48557158514985588, -11.25000000000002309, 6.000000000000000000 ) ) ;
#5035 = CARTESIAN_POINT ( 'NONE',  ( 14.27839713554442902, 24.50480966180208142, -12.54774083478067226 ) ) ;
#5036 = CARTESIAN_POINT ( 'NONE',  ( 15.29245034862073283, 32.56469986092002955, -4.999999999999995559 ) ) ;
#5037 = CARTESIAN_POINT ( 'NONE',  ( -19.23557158514982746, 34.18301270189230934, 11.00000000000000000 ) ) ;
#5038 = AXIS2_PLACEMENT_3D ( 'NONE', #27236, #20552, #8549 ) ;
#5039 = CIRCLE ( 'NONE', #22538, 1.000000000000000888 ) ;
#5040 = CARTESIAN_POINT ( 'NONE',  ( -28.06200121101475986, -24.80525908879649322, -5.439734138379792583 ) ) ;
#5041 = CARTESIAN_POINT ( 'NONE',  ( 3.177462754434345449, -21.84557965789944234, -20.09034133618861873 ) ) ;
#5042 = CARTESIAN_POINT ( 'NONE',  ( 13.65169929130708759, 22.50395429108296241, -15.47332144221692296 ) ) ;
#5043 = CARTESIAN_POINT ( 'NONE',  ( 20.53490407377033833, 13.94885239385593678, -6.452535063080207856 ) ) ;
#5044 = DIRECTION ( 'NONE',  ( 1.000000000000000000, 0.000000000000000000, 0.000000000000000000 ) ) ;
#5045 = EDGE_CURVE ( 'NONE', #11442, #7975, #40083, .T. ) ;
#5046 = VERTEX_POINT ( 'NONE', #27693 ) ;
#5047 = CARTESIAN_POINT ( 'NONE',  ( -4.882102130403945139, 28.26406243695034348, -16.69742253351011740 ) ) ;
#5048 = AXIS2_PLACEMENT_3D ( 'NONE', #16760, #16152, #4561 ) ;
#5049 = ORIENTED_EDGE ( 'NONE', *, *, #12811, .T. ) ;
#5050 = CIRCLE ( 'NONE', #18021, 16.00000000000000000 ) ;
#5051 = CARTESIAN_POINT ( 'NONE',  ( -14.61785853667976554, 5.591280219786782801, 9.500000000000000000 ) ) ;
#5052 = ORIENTED_EDGE ( 'NONE', *, *, #28478, .T. ) ;
#5053 = CARTESIAN_POINT ( 'NONE',  ( 10.54700836463452340, 22.39697303105787540, 10.50000000000000355 ) ) ;
#5054 = LINE ( 'NONE', #26991, #17436 ) ;
#5055 = VERTEX_POINT ( 'NONE', #24450 ) ;
#5056 = CARTESIAN_POINT ( 'NONE',  ( -28.01095669528613286, 0.5552823997827627256, -12.56944446269342031 ) ) ;
#5057 = ORIENTED_EDGE ( 'NONE', *, *, #23647, .F. ) ;
#5058 = CARTESIAN_POINT ( 'NONE',  ( 19.98763201709199322, -6.042670552197736633, -27.05847892281659028 ) ) ;
#5059 = ORIENTED_EDGE ( 'NONE', *, *, #5820, .F. ) ;
#5060 = CARTESIAN_POINT ( 'NONE',  ( -0.4999999999999998890, 37.44611345180491213, 10.76099332938163755 ) ) ;
#5061 = ORIENTED_EDGE ( 'NONE', *, *, #5889, .F. ) ;
#5062 = VECTOR ( 'NONE', #1848, 1000.000000000000114 ) ;
#5063 = CARTESIAN_POINT ( 'NONE',  ( -4.100643064501314328, 15.70406341247269211, 13.00000000000000178 ) ) ;
#5064 = DIRECTION ( 'NONE',  ( -0.5877852522924690293, 0.8090169943749503378, -0.000000000000000000 ) ) ;
#5065 = ADVANCED_FACE ( 'NONE', ( #36451 ), #27499, .T. ) ;
#5066 = VECTOR ( 'NONE', #2612, 1000.000000000000000 ) ;
#5067 = AXIS2_PLACEMENT_3D ( 'NONE', #31572, #4139, #10648 ) ;
#5068 = CYLINDRICAL_SURFACE ( 'NONE', #19444, 1.000000000000000888 ) ;
#5069 = VERTEX_POINT ( 'NONE', #34002 ) ;
#5070 = FILL_AREA_STYLE ('',( #39790 ) ) ;
#5071 = FACE_OUTER_BOUND ( 'NONE', #22935, .T. ) ;
#5072 = CARTESIAN_POINT ( 'NONE',  ( 14.57486473880226185, 26.18419839932902349, 11.00000000000000000 ) ) ;
#5073 = EDGE_CURVE ( 'NONE', #12092, #4676, #14974, .T. ) ;
#5074 = CIRCLE ( 'NONE', #16092, 1.000000000000014655 ) ;
#5075 = CARTESIAN_POINT ( 'NONE',  ( -3.831203748877743731, 25.75875950449070118, 23.00000000000000000 ) ) ;
#5076 = CARTESIAN_POINT ( 'NONE',  ( 19.05816791551096401, 16.93792299125899348, -5.962097903736426119 ) ) ;
#5077 = AXIS2_PLACEMENT_3D ( 'NONE', #22933, #7083, #19896 ) ;
#5078 = CARTESIAN_POINT ( 'NONE',  ( 9.191611640655853677, 25.94598456426656696, -16.91844301956545138 ) ) ;
#5079 = EDGE_LOOP ( 'NONE', ( #2646, #28638, #28377, #14455 ) ) ;
#5080 = LINE ( 'NONE', #14419, #12544 ) ;
#5081 = FACE_OUTER_BOUND ( 'NONE', #11146, .T. ) ;
#5082 = CARTESIAN_POINT ( 'NONE',  ( 9.998379901438696038, -18.29407794464048109, -26.80397355526891801 ) ) ;
#5083 = DIRECTION ( 'NONE',  ( -0.000000000000000000, 0.000000000000000000, -1.000000000000000000 ) ) ;
#5084 = CARTESIAN_POINT ( 'NONE',  ( 35.84808252048253507, -3.038699442442316379, -13.99876745781542553 ) ) ;
#5085 = CARTESIAN_POINT ( 'NONE',  ( -15.41023552481722447, 26.80405844223972522, -5.000000000000001776 ) ) ;
#5086 = CARTESIAN_POINT ( 'NONE',  ( -35.19094867589920028, -3.640833979052929603, 13.92931973827808889 ) ) ;
#5087 = CARTESIAN_POINT ( 'NONE',  ( 14.07774217773769898, -26.11933264415325340, -7.834443513061088105 ) ) ;
#5088 = EDGE_CURVE ( 'NONE', #22937, #30242, #17971, .T. ) ;
#5089 = DIRECTION ( 'NONE',  ( 0.3090169943749573322, 0.9510565162951504226, -0.000000000000000000 ) ) ;
#5090 = EDGE_CURVE ( 'NONE', #3614, #1872, #6158, .T. ) ;
#5091 = VERTEX_POINT ( 'NONE', #5959 ) ;
#5092 = ORIENTED_EDGE ( 'NONE', *, *, #9815, .F. ) ;
#5093 = CARTESIAN_POINT ( 'NONE',  ( -11.80160148247466978, 29.89982266266324729, -11.28701977302258541 ) ) ;
#5094 = LINE ( 'NONE', #5292, #37337 ) ;
#5095 = DIRECTION ( 'NONE',  ( -0.1045284632676436315, 0.9945218953682742891, 0.000000000000000000 ) ) ;
#5096 = AXIS2_PLACEMENT_3D ( 'NONE', #7676, #13160, #38352 ) ;
#5097 = CARTESIAN_POINT ( 'NONE',  ( -26.13677174093514566, -4.840508227981996647, -17.91196310124766455 ) ) ;
#5098 = CARTESIAN_POINT ( 'NONE',  ( 18.00000000000002487, 22.50000000000001421, 3.000000000000000000 ) ) ;
#5099 = ORIENTED_EDGE ( 'NONE', *, *, #31891, .T. ) ;
#5100 = CARTESIAN_POINT ( 'NONE',  ( 22.20747034583386892, 0.7192958970858360779, -22.74178951375157354 ) ) ;
#5101 = CARTESIAN_POINT ( 'NONE',  ( 11.20744270277970855, 31.91841037101594125, 11.00000000000000355 ) ) ;
#5102 = FACE_OUTER_BOUND ( 'NONE', #3933, .T. ) ;
#5103 = CARTESIAN_POINT ( 'NONE',  ( -24.45973306916671319, -28.60230771035024233, 10.99999999999987033 ) ) ;
#5104 = AXIS2_PLACEMENT_3D ( 'NONE', #2526, #39290, #24449 ) ;
#5105 = VERTEX_POINT ( 'NONE', #39493 ) ;
#5106 = CARTESIAN_POINT ( 'NONE',  ( -20.48192033757745278, 0.8608427067432721236, -29.34839852770058499 ) ) ;
#5107 = DIRECTION ( 'NONE',  ( 1.000000000000000000, 0.000000000000000000, 0.000000000000000000 ) ) ;
#5108 = ORIENTED_EDGE ( 'NONE', *, *, #6636, .T. ) ;
#5109 = CARTESIAN_POINT ( 'NONE',  ( 21.05756235747694305, -2.325109266878002678, -25.95433224628644098 ) ) ;
#5110 = CIRCLE ( 'NONE', #10946, 18.00000000000000000 ) ;
#5111 = CARTESIAN_POINT ( 'NONE',  ( 35.98781724630865142, -12.75392035872628860, 15.72805884748942873 ) ) ;
#5112 = ORIENTED_EDGE ( 'NONE', *, *, #16329, .T. ) ;
#5113 = CARTESIAN_POINT ( 'NONE',  ( -5.381339405376368568, 38.47497618056175384, 15.13084544680213561 ) ) ;
#5114 = CARTESIAN_POINT ( 'NONE',  ( 5.304193131309242304, -23.76115801358234947, 17.42190598798392998 ) ) ;
#5115 = LINE ( 'NONE', #17522, #9812 ) ;
#5116 = ADVANCED_FACE ( 'NONE', ( #32660 ), #11070, .F. ) ;
#5117 = CARTESIAN_POINT ( 'NONE',  ( -6.949287954459967942, 25.26733242291857451, 20.82122704794066692 ) ) ;
#5118 = CARTESIAN_POINT ( 'NONE',  ( -3.370709253380788084E-06, 22.50000000000031264, 12.00000000000000000 ) ) ;
#5119 = ORIENTED_EDGE ( 'NONE', *, *, #23443, .T. ) ;
#5120 = CARTESIAN_POINT ( 'NONE',  ( 5.473344025737212348, 14.11593743010426394, 10.00000000000000000 ) ) ;
#5121 = CARTESIAN_POINT ( 'NONE',  ( 19.48557158514982746, -11.25000000000009415, 0.000000000000000000 ) ) ;
#5122 = AXIS2_PLACEMENT_3D ( 'NONE', #3034, #22118, #19265 ) ;
#5124 = CIRCLE ( 'NONE', #38212, 18.00000000000000000 ) ;
#5123 = CARTESIAN_POINT ( 'NONE',  ( 3.938319053363494859, 24.20383553360720796, -20.77087860374098938 ) ) ;
#5125 = DIRECTION ( 'NONE',  ( -0.6724985119639661502, -0.2185080122244085765, -0.7071067811865395791 ) ) ;
#5126 = CARTESIAN_POINT ( 'NONE',  ( 11.11100267139158859, 25.58833710558854690, 19.66345542862528362 ) ) ;
#5127 = CARTESIAN_POINT ( 'NONE',  ( 19.65700424793906009, -25.74060475042004015, -10.40124817034949167 ) ) ;
#5128 = CARTESIAN_POINT ( 'NONE',  ( -10.36702044712414938, 31.16169077310601665, 10.00000000000000000 ) ) ;
#5129 = AXIS2_PLACEMENT_3D ( 'NONE', #32355, #20369, #4918 ) ;
#5130 = DIRECTION ( 'NONE',  ( 1.000000000000000000, 0.000000000000000000, 0.000000000000000000 ) ) ;
#5131 = CARTESIAN_POINT ( 'NONE',  ( 2.518583951651050867, 7.712953814960687104, 7.499999999999990230 ) ) ;
#5132 = EDGE_LOOP ( 'NONE', ( #10626, #13423, #30043, #14936 ) ) ;
#5133 = CARTESIAN_POINT ( 'NONE',  ( 12.33829340598856916, 20.56101506373660470, -19.48517987220360226 ) ) ;
#5134 = EDGE_LOOP ( 'NONE', ( #35801, #2702 ) ) ;
#5135 = CARTESIAN_POINT ( 'NONE',  ( -13.45522894562555116, 21.80059734131468474, -16.48174157838437281 ) ) ;
#5136 = CARTESIAN_POINT ( 'NONE',  ( -19.04855072600353338, -23.59522350949000469, 19.27171037444189139 ) ) ;
#5137 = DIRECTION ( 'NONE',  ( -0.6123724356957963577, -0.3535533905932671805, -0.7071067811865491270 ) ) ;
#5138 = CARTESIAN_POINT ( 'NONE',  ( 14.59096746045820581, 24.81100808824554704, -11.60372034950707842 ) ) ;
#5139 = ORIENTED_EDGE ( 'NONE', *, *, #27671, .T. ) ;
#5140 = CARTESIAN_POINT ( 'NONE',  ( 31.64230937557188739, -20.05769974086166130, -8.405444945822866387 ) ) ;
#5141 = ORIENTED_EDGE ( 'NONE', *, *, #35796, .F. ) ;
#5143 = CARTESIAN_POINT ( 'NONE',  ( -5.458872323573595864, 26.51478363815348160, 6.000000000000000000 ) ) ;
#5142 = CARTESIAN_POINT ( 'NONE',  ( -10.67558526762242188, 17.55646416338892735, -28.69320066300005934 ) ) ;
#5144 = CARTESIAN_POINT ( 'NONE',  ( -18.17112659014724230, -26.98930163720866560, -7.288977103906384869 ) ) ;
#5145 = CARTESIAN_POINT ( 'NONE',  ( 12.30736835487432757, 14.81698729810772441, 11.00000000000000000 ) ) ;
#5146 = ADVANCED_FACE ( 'NONE', ( #17780 ), #2527, .T. ) ;
#5147 = ORIENTED_EDGE ( 'NONE', *, *, #4164, .T. ) ;
#5148 = CARTESIAN_POINT ( 'NONE',  ( -22.09523395385413380, -8.380097828030171669, -21.91654685885929155 ) ) ;
#5149 = CARTESIAN_POINT ( 'NONE',  ( -14.83609535436326432, -26.57805634534657102, -5.000000000000000888 ) ) ;
#5150 = CARTESIAN_POINT ( 'NONE',  ( 18.23649648353767461, -16.09146789626181118, 23.00000000000000000 ) ) ;
#5151 = EDGE_LOOP ( 'NONE', ( #28880, #36655, #18979, #36838 ) ) ;
#5152 = CARTESIAN_POINT ( 'NONE',  ( 28.80506163160762512, 1.156882464205359007, -9.731288915196888212 ) ) ;
#5153 = DIRECTION ( 'NONE',  ( 1.000000000000000000, 0.000000000000000000, 0.000000000000000000 ) ) ;
#5154 = CARTESIAN_POINT ( 'NONE',  ( -5.348113209407908464, 9.835177808069893501, 6.000000000000000000 ) ) ;
#5155 = ORIENTED_EDGE ( 'NONE', *, *, #14362, .T. ) ;
#5156 = CARTESIAN_POINT ( 'NONE',  ( -22.24152314221094784, 0.5810505375398892225, -22.72432294289647103 ) ) ;
#5157 = CARTESIAN_POINT ( 'NONE',  ( 24.27527364323341175, -0.3479384314849937043, -19.38528656166962705 ) ) ;
#5158 = CIRCLE ( 'NONE', #12286, 0.4999999999999988898 ) ;
#5159 = CARTESIAN_POINT ( 'NONE',  ( 28.78471548569268279, -2.122417091766370945, 18.87996532025785257 ) ) ;
#5160 = EDGE_LOOP ( 'NONE', ( #5092, #21096, #24093, #4982, #16138, #5494, #19649, #5139, #40159, #8031, #4200, #33238, #35762, #16784, #28868, #23622, #29969, #24635, #35062, #27667, #22322, #3745, #9855, #31781, #18261, #292 ) ) ;
#5161 = CARTESIAN_POINT ( 'NONE',  ( -21.85307150740203141, 2.101201123924372194, -22.89954997427944505 ) ) ;
#5162 = CIRCLE ( 'NONE', #27861, 1.000000000000004441 ) ;
#5163 = CARTESIAN_POINT ( 'NONE',  ( -9.163310636333559245, 20.63632441393290762, -20.55760979252981357 ) ) ;
#5164 = ADVANCED_FACE ( 'NONE', ( #27102 ), #11865, .T. ) ;
#5165 = CARTESIAN_POINT ( 'NONE',  ( -13.47830981910552772, 21.58612669357095015, 9.500000000000000000 ) ) ;
#5166 = DIRECTION ( 'NONE',  ( -0.000000000000000000, 0.000000000000000000, -1.000000000000000000 ) ) ;
#5167 = ADVANCED_FACE ( 'NONE', ( #24254 ), #36649, .F. ) ;
#5168 = EDGE_CURVE ( 'NONE', #34341, #15686, #31817, .T. ) ;
#5169 = DIRECTION ( 'NONE',  ( -0.000000000000000000, -0.000000000000000000, -1.000000000000000000 ) ) ;
#5170 = CARTESIAN_POINT ( 'NONE',  ( -4.706342468480190000, 20.64589803375067945, 12.00000000000000000 ) ) ;
#5171 = DIRECTION ( 'NONE',  ( 0.7071067811865500152, 0.000000000000000000, -0.7071067811865450192 ) ) ;
#5172 = ORIENTED_EDGE ( 'NONE', *, *, #30341, .T. ) ;
#5173 = CARTESIAN_POINT ( 'NONE',  ( -20.62745669879552324, 5.024763284673062991, -24.24502725807042580 ) ) ;
#5174 = CARTESIAN_POINT ( 'NONE',  ( -9.665073660138977729, 25.11464168560200250, 10.50000000000000000 ) ) ;
#5175 = DIRECTION ( 'NONE',  ( -0.000000000000000000, -0.000000000000000000, -1.000000000000000000 ) ) ;
#5176 = CARTESIAN_POINT ( 'NONE',  ( 14.64330500336448004, -14.34584279044560162, -29.24371549410482274 ) ) ;
#5177 = DIRECTION ( 'NONE',  ( 1.000000000000000000, 1.734723475976793684E-15, 0.000000000000000000 ) ) ;
#5178 = CARTESIAN_POINT ( 'NONE',  ( 12.19134295108989718, 16.61602540378438775, 9.500000000000000000 ) ) ;
#5179 = CARTESIAN_POINT ( 'NONE',  ( 10.63104621300768216, 17.52826713075782905, -29.34073607691351526 ) ) ;
#5180 = CARTESIAN_POINT ( 'NONE',  ( -10.10865978838755908, -27.35622988135655476, 12.14047268034456017 ) ) ;
#5181 = CIRCLE ( 'NONE', #23367, 15.00000000000000000 ) ;
#5182 = ORIENTED_EDGE ( 'NONE', *, *, #13464, .F. ) ;
#5183 = CARTESIAN_POINT ( 'NONE',  ( -16.44336537299682988, 20.94030426362907704, -10.75757732011587109 ) ) ;
#5184 = CARTESIAN_POINT ( 'NONE',  ( -19.96384346486619066, -17.84145166816490047, 20.94377226548378346 ) ) ;
#5185 = CARTESIAN_POINT ( 'NONE',  ( 0.8712018466506370462, 31.30332840660451765, 6.000000000000000000 ) ) ;
#5186 = CARTESIAN_POINT ( 'NONE',  ( 15.10958474974925636, 26.11133633985198443, -8.767902982274385693 ) ) ;
#5187 = EDGE_LOOP ( 'NONE', ( #17458, #27885, #1714, #16908 ) ) ;
#5188 = CARTESIAN_POINT ( 'NONE',  ( -14.70895476143393488, 21.92515157238299039, 10.49999999999999822 ) ) ;
#5189 = CIRCLE ( 'NONE', #27892, 15.00000000000000000 ) ;
#5190 = ORIENTED_EDGE ( 'NONE', *, *, #8305, .T. ) ;
#5192 = DIRECTION ( 'NONE',  ( 0.000000000000000000, 0.000000000000000000, 1.000000000000000000 ) ) ;
#5191 = CARTESIAN_POINT ( 'NONE',  ( -10.92267213224567968, 17.34778819946280493, -29.34702194411721266 ) ) ;
#5193 = ADVANCED_FACE ( 'NONE', ( #6745 ), #38039, .T. ) ;
#5194 = CARTESIAN_POINT ( 'NONE',  ( -15.25928708397310096, -26.30311034880537235, -8.294554573284210974 ) ) ;
#5195 = CARTESIAN_POINT ( 'NONE',  ( -37.34232268491268769, -8.983628415038266368, 11.00000000000000000 ) ) ;
#5196 = ADVANCED_FACE ( 'NONE', ( #9618 ), #472, .F. ) ;
#5197 = CARTESIAN_POINT ( 'NONE',  ( -17.86905274512871244, -10.06606982860865784, -29.21172267095328223 ) ) ;
#5198 = CARTESIAN_POINT ( 'NONE',  ( -5.097925932147637340, -20.80854798773387770, -23.20461931772074138 ) ) ;
#5199 = FACE_OUTER_BOUND ( 'NONE', #13457, .T. ) ;
#5200 = CARTESIAN_POINT ( 'NONE',  ( 15.82933155468543518, 25.27777941642500537, -5.946733502468819488 ) ) ;
#5201 = VERTEX_POINT ( 'NONE', #28296 ) ;
#5202 = CARTESIAN_POINT ( 'NONE',  ( 24.82669879306046212, 6.427578836846941535, -9.348943503324091964 ) ) ;
#5203 = DIRECTION ( 'NONE',  ( 1.000000000000000000, 0.000000000000000000, 0.000000000000000000 ) ) ;
#5204 = DIRECTION ( 'NONE',  ( 0.000000000000000000, -1.000000000000000000, 0.000000000000000000 ) ) ;
#5205 = DIRECTION ( 'NONE',  ( 0.6216356077939589886, 0.000000000000000000, -0.7833065626704751594 ) ) ;
#5206 = ORIENTED_EDGE ( 'NONE', *, *, #19689, .F. ) ;
#5207 = CARTESIAN_POINT ( 'NONE',  ( -30.07554202086022954, -1.447249947434508854, -11.47170067724066733 ) ) ;
#5208 = CARTESIAN_POINT ( 'NONE',  ( 28.46466429971498968, -0.01335223302803286403, -12.53469640236253824 ) ) ;
#5209 = CARTESIAN_POINT ( 'NONE',  ( -13.01838097023000707, 23.73363068877903359, 12.00000000000000000 ) ) ;
#5210 = CARTESIAN_POINT ( 'NONE',  ( 20.67756474496276908, -17.78966446931796952, 20.94377226548379056 ) ) ;
#5211 = DIRECTION ( 'NONE',  ( -0.000000000000000000, -0.000000000000000000, -1.000000000000000000 ) ) ;
#5212 = SURFACE_STYLE_USAGE ( .BOTH. , #1980 ) ;
#5213 = EDGE_CURVE ( 'NONE', #1404, #39240, #34398, .T. ) ;
#5214 = CARTESIAN_POINT ( 'NONE',  ( 33.69589222704783538, -0.03122585499640089662, 11.00000000000003730 ) ) ;
#5215 = ADVANCED_FACE ( 'NONE', ( #3907 ), #15704, .F. ) ;
#5216 = ORIENTED_EDGE ( 'NONE', *, *, #39843, .T. ) ;
#5217 = AXIS2_PLACEMENT_3D ( 'NONE', #32609, #2875, #4767 ) ;
#5218 = DIRECTION ( 'NONE',  ( 1.000000000000000000, 0.000000000000000000, 0.000000000000000000 ) ) ;
#5219 = CARTESIAN_POINT ( 'NONE',  ( 14.26584437371809777, 27.13525491562438319, 12.00000000000000000 ) ) ;
#5220 = DIRECTION ( 'NONE',  ( 0.7771459614569634633, -0.6293203910498466058, 2.315526266344420400E-15 ) ) ;
#5221 = CARTESIAN_POINT ( 'NONE',  ( 0.3120762500772759629, 29.08244079073152477, -16.62608502115921993 ) ) ;
#5222 = CARTESIAN_POINT ( 'NONE',  ( -16.00000000000000000, 22.50000000000000355, 10.00000000000000000 ) ) ;
#5223 = DIRECTION ( 'NONE',  ( 0.000000000000000000, 0.000000000000000000, 1.000000000000000000 ) ) ;
#5224 = CARTESIAN_POINT ( 'NONE',  ( 5.440908595777817602, 35.94977745735560859, 7.000000000000000000 ) ) ;
#5225 = CARTESIAN_POINT ( 'NONE',  ( 7.659620408498160060, 26.92228390473674793, 9.000000000000001776 ) ) ;
#5226 = DIRECTION ( 'NONE',  ( 0.000000000000000000, 0.000000000000000000, 1.000000000000000000 ) ) ;
#5227 = CARTESIAN_POINT ( 'NONE',  ( 3.000488737323008248, 30.46850471149999962, 9.000000000000001776 ) ) ;
#5228 = CARTESIAN_POINT ( 'NONE',  ( 14.88818521422670571, 28.28006465736570618, -5.930970288686092218 ) ) ;
#5229 = DIRECTION ( 'NONE',  ( 0.9135454576426004225, -0.4067366430758009854, 0.000000000000000000 ) ) ;
#5230 = ORIENTED_EDGE ( 'NONE', *, *, #7321, .F. ) ;
#5231 = AXIS2_PLACEMENT_3D ( 'NONE', #28692, #19549, #13450 ) ;
#5233 = CARTESIAN_POINT ( 'NONE',  ( -7.096882951594430722, 29.56287847632736288, 10.49999999999999822 ) ) ;
#5232 = CARTESIAN_POINT ( 'NONE',  ( -18.87212912419562016, 14.83998797668345659, -12.86572329467758458 ) ) ;
#5234 = CARTESIAN_POINT ( 'NONE',  ( -1.000000000000000444, 37.00000000000000711, 10.49999999999999822 ) ) ;
#5235 = AXIS2_PLACEMENT_3D ( 'NONE', #9269, #24703, #21653 ) ;
#5236 = CARTESIAN_POINT ( 'NONE',  ( 15.52090202525632279, -26.75102145164868972, -5.000000000000000888 ) ) ;
#5237 = CARTESIAN_POINT ( 'NONE',  ( 12.64210930126479937, 24.20081211342298744, 13.00000000000000178 ) ) ;
#5238 = B_SPLINE_CURVE_WITH_KNOTS ( 'NONE', 3,
 ( #31058, #18665, #379, #16012, #15812, #12757 ),
 .UNSPECIFIED., .F., .F.,
 ( 4, 2, 4 ),
 ( 0.000000000000000000, 0.3000000000367072928, 0.6000000000734145855 ),
 .UNSPECIFIED. ) ;
#5239 = CARTESIAN_POINT ( 'NONE',  ( 15.32791351282358505, 26.65397767157460507, -6.887199522823470588 ) ) ;
#5240 = CARTESIAN_POINT ( 'NONE',  ( 9.831584923911636409, 26.22020669908449975, 10.00000000000000000 ) ) ;
#5241 = CARTESIAN_POINT ( 'NONE',  ( 23.09341954621653414, -31.04079623342705574, 11.00000000000000000 ) ) ;
#5242 = CARTESIAN_POINT ( 'NONE',  ( -16.07603441159168867, -13.35307911771159972, -27.01628995842852987 ) ) ;
#5243 = CARTESIAN_POINT ( 'NONE',  ( 1.676194954344619292, -23.72096887343614924, -12.89182188841930454 ) ) ;
#5244 = CARTESIAN_POINT ( 'NONE',  ( 12.29335586182468631, 19.73195647831804678, -20.56948206563339454 ) ) ;
#5245 = CARTESIAN_POINT ( 'NONE',  ( 17.63004972000715753, 10.74884895982777522, -27.17813552644222241 ) ) ;
#5246 = CARTESIAN_POINT ( 'NONE',  ( 0.5000000000000001110, 37.00000000000000711, 11.00000000000000000 ) ) ;
#5247 = EDGE_CURVE ( 'NONE', #30411, #17610, #30558, .T. ) ;
#5248 = VERTEX_POINT ( 'NONE', #18954 ) ;
#5249 = CARTESIAN_POINT ( 'NONE',  ( -4.870223975577004261, 20.79813088136934240, -25.69976142956964438 ) ) ;
#5250 = ORIENTED_EDGE ( 'NONE', *, *, #21062, .T. ) ;
#5251 = CARTESIAN_POINT ( 'NONE',  ( 5.537946624086096392, 36.44027069998188750, 7.500000000000000888 ) ) ;
#5252 = ORIENTED_EDGE ( 'NONE', *, *, #25945, .T. ) ;
#5253 = DIRECTION ( 'NONE',  ( 0.2876062384759510704, 0.6459741880212550580, -0.7071067811865435759 ) ) ;
#5254 = FACE_OUTER_BOUND ( 'NONE', #17209, .T. ) ;
#5255 = ORIENTED_EDGE ( 'NONE', *, *, #11339, .T. ) ;
#5256 = CARTESIAN_POINT ( 'NONE',  ( -28.17636587710437368, 0.3453695044007577541, -12.55976439041781312 ) ) ;
#5257 = EDGE_LOOP ( 'NONE', ( #14272, #17943, #32119, #19918 ) ) ;
#5258 = CARTESIAN_POINT ( 'NONE',  ( 30.05582894924074111, -10.02326609248156331, -13.87827096244793879 ) ) ;
#5259 = CIRCLE ( 'NONE', #6548, 0.4999999999999995559 ) ;
#5260 = CIRCLE ( 'NONE', #10451, 18.00000000000000000 ) ;
#5261 = ORIENTED_EDGE ( 'NONE', *, *, #27749, .T. ) ;
#5262 = CARTESIAN_POINT ( 'NONE',  ( -0.4999999999999995559, 37.00000000000000711, 11.00000000000000000 ) ) ;
#5263 = EDGE_LOOP ( 'NONE', ( #265, #23594, #32859, #9443 ) ) ;
#5264 = DIRECTION ( 'NONE',  ( 0.4999999999999933942, -0.8660254037844425934, 0.000000000000000000 ) ) ;
#5265 = DIRECTION ( 'NONE',  ( 0.5254827454987650581, -0.4731467892558172683, -0.7071067811865414665 ) ) ;
#5266 = CARTESIAN_POINT ( 'NONE',  ( 9.806975420853749625, 31.15003855377755571, 6.000000000000000000 ) ) ;
#5267 = ORIENTED_EDGE ( 'NONE', *, *, #33008, .F. ) ;
#5268 = CARTESIAN_POINT ( 'NONE',  ( 6.354454053420413473, 35.54304081427980577, 11.00000000000000000 ) ) ;
#5269 = CARTESIAN_POINT ( 'NONE',  ( 2.036571916123615100, 8.108948098542045457, 10.49999999999999467 ) ) ;
#5270 = ADVANCED_FACE ( 'NONE', ( #12657 ), #25050, .T. ) ;
#5271 = CIRCLE ( 'NONE', #12401, 1.000000000000000888 ) ;
#5272 = DIRECTION ( 'NONE',  ( 0.9945218953682727347, -0.1045284632676597436, -3.469446951953608667E-15 ) ) ;
#5273 = CARTESIAN_POINT ( 'NONE',  ( 18.50304859244888789, 17.84556192672934927, -7.408648105292232167 ) ) ;
#5274 = CARTESIAN_POINT ( 'NONE',  ( 7.149399299886240122, 20.02420714680316394, -25.84280504995552619 ) ) ;
#5275 = EDGE_LOOP ( 'NONE', ( #11952, #31131, #17080, #33165 ) ) ;
#5276 = CARTESIAN_POINT ( 'NONE',  ( -18.35172899305704064, 9.167379654309337766, -29.99999999999999645 ) ) ;
#5277 = DIRECTION ( 'NONE',  ( -0.3090169943749457304, 0.9510565162951540863, 0.000000000000000000 ) ) ;
#5278 = CARTESIAN_POINT ( 'NONE',  ( -13.16028273094462975, 27.30176617939698147, 9.500000000000000000 ) ) ;
#5279 = CARTESIAN_POINT ( 'NONE',  ( 15.58925272520251148, -26.26116752309117786, -8.745968726765523726 ) ) ;
#5280 = CARTESIAN_POINT ( 'NONE',  ( 17.83459896181130944, -17.64923967996766052, 20.94377226548378701 ) ) ;
#5281 = CARTESIAN_POINT ( 'NONE',  ( 17.34253826539385201, 27.32041144647958575, -5.000000000000000000 ) ) ;
#5282 = CARTESIAN_POINT ( 'NONE',  ( -13.20200830158507443, 22.24945722037973184, -16.44235390662751328 ) ) ;
#5283 = VECTOR ( 'NONE', #25347, 1000.000000000000114 ) ;
#5284 = CARTESIAN_POINT ( 'NONE',  ( -34.99622266290882777, -18.09877784578709026, 15.13084544680241272 ) ) ;
#5285 = CARTESIAN_POINT ( 'NONE',  ( 13.83190959151879618, -25.74325333655491121, -9.252723044361745863 ) ) ;
#5286 = VECTOR ( 'NONE', #38388, 1000.000000000000000 ) ;
#5287 = ADVANCED_FACE ( 'NONE', ( #16308 ), #25248, .T. ) ;
#5288 = CARTESIAN_POINT ( 'NONE',  ( 11.44473057578109021, 31.45924896672603310, 10.49999999999999822 ) ) ;
#5289 = ORIENTED_EDGE ( 'NONE', *, *, #12815, .F. ) ;
#5290 = VERTEX_POINT ( 'NONE', #9814 ) ;
#5291 = CARTESIAN_POINT ( 'NONE',  ( -12.43868061211408005, 31.69022611209930318, -8.118098891794449656 ) ) ;
#5292 = CARTESIAN_POINT ( 'NONE',  ( -13.62380822250706736, 25.87518140495425101, 9.500000000000000000 ) ) ;
#5293 = ADVANCED_FACE ( 'NONE', ( #21999 ), #4107, .T. ) ;
#5294 = DIRECTION ( 'NONE',  ( -0.7032331762534049791, 0.07391278520358846027, -0.7071067811865444641 ) ) ;
#5295 = FACE_OUTER_BOUND ( 'NONE', #6973, .T. ) ;
#5296 = EDGE_LOOP ( 'NONE', ( #23160, #17802, #16395, #37290 ) ) ;
#5297 = CARTESIAN_POINT ( 'NONE',  ( 20.47975215921984216, 0.9111364859620189049, -29.34931494995705847 ) ) ;
#5298 = ADVANCED_FACE ( 'NONE', ( #34200 ), #16107, .F. ) ;
#5299 = DIRECTION ( 'NONE',  ( 1.000000000000000000, 0.000000000000000000, 0.000000000000000000 ) ) ;
#5300 = FACE_OUTER_BOUND ( 'NONE', #19706, .T. ) ;
#5301 = CARTESIAN_POINT ( 'NONE',  ( -2.061816823438740620, 8.019625857904001620, 10.49999999999999822 ) ) ;
#5302 = ADVANCED_FACE ( 'NONE', ( #868 ), #18760, .F. ) ;
#5303 = ORIENTED_EDGE ( 'NONE', *, *, #36682, .F. ) ;
#5304 = CARTESIAN_POINT ( 'NONE',  ( -29.78514619038734068, 0.06227709271290194498, -9.709532440474664128 ) ) ;
#5305 = CARTESIAN_POINT ( 'NONE',  ( -5.517564457587356586, 36.12194934191566631, 10.96580508970282430 ) ) ;
#5306 = ORIENTED_EDGE ( 'NONE', *, *, #9261, .T. ) ;
#5307 = CARTESIAN_POINT ( 'NONE',  ( 33.96295552133759088, -5.157459216464866714, -7.229003133675814929 ) ) ;
#5308 = CARTESIAN_POINT ( 'NONE',  ( 26.00889624226716990, -26.79364542773732083, 15.13084544680213384 ) ) ;
#5309 = ORIENTED_EDGE ( 'NONE', *, *, #34978, .F. ) ;
#5310 = CARTESIAN_POINT ( 'NONE',  ( 13.38235399890562682, 33.85943911868815093, 13.92931973827816883 ) ) ;
#5311 = DIRECTION ( 'NONE',  ( 0.000000000000000000, 0.000000000000000000, 1.000000000000000000 ) ) ;
#5312 = LINE ( 'NONE', #11810, #29907 ) ;
#5313 = CARTESIAN_POINT ( 'NONE',  ( -4.288075229729694016, 29.62123851723948675, 20.69868183039744025 ) ) ;
#5314 = LINE ( 'NONE', #29896, #18131 ) ;
#5315 = EDGE_LOOP ( 'NONE', ( #39821, #10489, #17426, #25936 ) ) ;
#5316 = DIRECTION ( 'NONE',  ( 1.000000000000000000, 0.000000000000000000, 0.000000000000000000 ) ) ;
#5317 = EDGE_CURVE ( 'NONE', #17826, #34540, #13248, .T. ) ;
#5318 = CARTESIAN_POINT ( 'NONE',  ( -8.927394655428429360, 11.06314620770957013, 7.500000000000000888 ) ) ;
#5319 = EDGE_CURVE ( 'NONE', #3128, #6055, #19150, .T. ) ;
#5320 = CARTESIAN_POINT ( 'NONE',  ( 3.344107530154690977, 20.63130717731051789, -27.01118353652808679 ) ) ;
#5321 = CARTESIAN_POINT ( 'NONE',  ( 8.183240348400453001, 28.21559575157615996, 13.00000000000000178 ) ) ;
#5322 = CARTESIAN_POINT ( 'NONE',  ( 21.27192666511442098, -1.272056932922072114, 20.69868183040414422 ) ) ;
#5323 = VECTOR ( 'NONE', #29632, 1000.000000000000227 ) ;
#5324 = CARTESIAN_POINT ( 'NONE',  ( 18.80843487349309839, -26.01514764349690978, -9.984653526650497213 ) ) ;
#5325 = CARTESIAN_POINT ( 'NONE',  ( 15.98959510862178668, 30.99271259066394180, 10.99999999999987743 ) ) ;
#5326 = CARTESIAN_POINT ( 'NONE',  ( -11.41268156625113406, 18.79179606750104981, 12.00000000000000000 ) ) ;
#5327 = CARTESIAN_POINT ( 'NONE',  ( 37.57549957648898697, 32.94422479542058824, 3.000000000000000000 ) ) ;
#5328 = EDGE_LOOP ( 'NONE', ( #8807, #2289, #6785, #39254 ) ) ;
#5329 = CARTESIAN_POINT ( 'NONE',  ( 15.06417566331624336, 26.26151533851359332, -8.762166468963160426 ) ) ;
#5330 = EDGE_LOOP ( 'NONE', ( #14409, #26437 ) ) ;
#5331 = CARTESIAN_POINT ( 'NONE',  ( -15.46686712649010254, 26.33727822508064875, -6.417365845589783291 ) ) ;
#5332 = VECTOR ( 'NONE', #10036, 1000.000000000000000 ) ;
#5333 = CARTESIAN_POINT ( 'NONE',  ( -30.32526513704001303, -2.692717509695762512, 18.42518152272108622 ) ) ;
#5334 = CARTESIAN_POINT ( 'NONE',  ( 20.23296131041715640, 28.12381335138032412, 3.000000000000000000 ) ) ;
#5335 = CARTESIAN_POINT ( 'NONE',  ( 11.20885904078801687, 17.55440590958596658, -26.83820411716370913 ) ) ;
#5336 = VERTEX_POINT ( 'NONE', #25436 ) ;
#5337 = CARTESIAN_POINT ( 'NONE',  ( 18.45928777744525817, -10.91947781374027926, -25.57488933213381088 ) ) ;
#5338 = ORIENTED_EDGE ( 'NONE', *, *, #20021, .T. ) ;
#5340 = CARTESIAN_POINT ( 'NONE',  ( -9.468266739736646898, 17.89951905283841782, 10.74999999999999822 ) ) ;
#5339 = CARTESIAN_POINT ( 'NONE',  ( -11.32776516902169206, 19.24857545329237496, -22.67347498135675821 ) ) ;
#5341 = CARTESIAN_POINT ( 'NONE',  ( -17.74186490489988444, -26.41810987378744002, -9.118522922409818321 ) ) ;
#5342 = ADVANCED_FACE ( 'NONE', ( #666 ), #13047, .F. ) ;
#5343 = DIRECTION ( 'NONE',  ( -0.7071067811865524577, 0.000000000000000000, -0.7071067811865426878 ) ) ;
#5344 = ORIENTED_EDGE ( 'NONE', *, *, #34521, .T. ) ;
#5345 = CARTESIAN_POINT ( 'NONE',  ( -24.05107439686812398, -8.291669621499529796, -19.73756104527254962 ) ) ;
#5346 = CARTESIAN_POINT ( 'NONE',  ( -9.780434648196228764, -18.88852710088067610, -25.03561068106941079 ) ) ;
#5347 = AXIS2_PLACEMENT_3D ( 'NONE', #14063, #39450, #5130 ) ;
#5348 = CARTESIAN_POINT ( 'NONE',  ( 23.54493052986452284, -14.21898406159493788, 23.00000000000000000 ) ) ;
#5349 = VERTEX_POINT ( 'NONE', #31746 ) ;
#5350 = CARTESIAN_POINT ( 'NONE',  ( 27.98159544772139995, 1.197522363590045602, -11.63887822456392840 ) ) ;
#5351 = PLANE ( 'NONE',  #17417 ) ;
#5352 = CARTESIAN_POINT ( 'NONE',  ( -38.42882785865669604, -4.479089857567689847, 11.00000000000000000 ) ) ;
#5353 = EDGE_LOOP ( 'NONE', ( #24730, #19339, #20809, #22845 ) ) ;
#5354 = CARTESIAN_POINT ( 'NONE',  ( -29.44376907024975765, -0.02629414463411203565, -10.64560707404265116 ) ) ;
#5355 = ORIENTED_EDGE ( 'NONE', *, *, #22653, .F. ) ;
#5356 = CARTESIAN_POINT ( 'NONE',  ( 22.91868624822824074, -0.04345034985262812705, -21.52910780376702249 ) ) ;
#5357 = CARTESIAN_POINT ( 'NONE',  ( 17.49459433713328593, -24.91609123032452899, 18.42518152272071674 ) ) ;
#5358 = EDGE_LOOP ( 'NONE', ( #9191, #9766, #40103, #27292 ) ) ;
#5359 = AXIS2_PLACEMENT_3D ( 'NONE', #14330, #14531, #11689 ) ;
#5360 = CARTESIAN_POINT ( 'NONE',  ( -27.46442853353828184, 3.518614321624921715, -7.380921586237230159 ) ) ;
#5361 = DIRECTION ( 'NONE',  ( 1.000000000000000000, 0.000000000000000000, 0.000000000000000000 ) ) ;
#5362 = DIRECTION ( 'NONE',  ( 0.000000000000000000, 0.000000000000000000, 1.000000000000000000 ) ) ;
#5363 = VECTOR ( 'NONE', #38421, 1000.000000000000000 ) ;
#5364 = CARTESIAN_POINT ( 'NONE',  ( -17.21213525677265821, -20.06193531423681975, 20.50957957746029692 ) ) ;
#5365 = EDGE_CURVE ( 'NONE', #31289, #39512, #6515, .T. ) ;
#5366 = DIRECTION ( 'NONE',  ( -0.9135454576426071949, -0.4067366430757861639, 0.000000000000000000 ) ) ;
#5367 = CARTESIAN_POINT ( 'NONE',  ( -7.935776944912362296, 22.65328985282726393, 13.00000000000000178 ) ) ;
#5368 = DIRECTION ( 'NONE',  ( 0.6037757019622813637, 0.000000000000000000, 0.7971542521494534572 ) ) ;
#5369 = ORIENTED_EDGE ( 'NONE', *, *, #22039, .T. ) ;
#5370 = CARTESIAN_POINT ( 'NONE',  ( -25.46978366468587041, 6.210661816339332120, -6.438542239147753143 ) ) ;
#5371 = DIRECTION ( 'NONE',  ( -0.5000000000000041078, -0.8660254037844362651, 0.000000000000000000 ) ) ;
#5372 = PLANE ( 'NONE',  #37636 ) ;
#5373 = CARTESIAN_POINT ( 'NONE',  ( 20.09942049894790728, -20.92583357156711799, -15.85785305014610458 ) ) ;
#5374 = CARTESIAN_POINT ( 'NONE',  ( -6.688306800005769048, 28.52217545723006609, 13.00000000000000178 ) ) ;
#5375 = CARTESIAN_POINT ( 'NONE',  ( -14.40879062396297883, 19.98622263052321557, 10.49999999999999822 ) ) ;
#5376 = CARTESIAN_POINT ( 'NONE',  ( 10.96925589186059113, 18.29886720915252241, -24.96787355622415561 ) ) ;
#5377 = AXIS2_PLACEMENT_3D ( 'NONE', #38600, #32106, #4872 ) ;
#5378 = CARTESIAN_POINT ( 'NONE',  ( 10.29072928255106234, -26.28675887227032248, 15.13084544680038235 ) ) ;
#5379 = EDGE_LOOP ( 'NONE', ( #954, #17255, #39948, #14445, #27629 ) ) ;
#5380 = CARTESIAN_POINT ( 'NONE',  ( -14.49113235944208355, 19.17988935812739371, -17.67406450707707322 ) ) ;
#5381 = CARTESIAN_POINT ( 'NONE',  ( -24.79273775960151482, -6.040746354374424421, 20.82122704794080192 ) ) ;
#5382 = CIRCLE ( 'NONE', #6050, 16.00000000000000000 ) ;
#5383 = DIRECTION ( 'NONE',  ( -0.000000000000000000, -0.000000000000000000, -1.000000000000000000 ) ) ;
#5384 = CARTESIAN_POINT ( 'NONE',  ( 11.32792303687276991, 18.02407018003295747, -25.01698112430106846 ) ) ;
#5385 = EDGE_LOOP ( 'NONE', ( #16291, #21565, #14687, #13936 ) ) ;
#5386 = CARTESIAN_POINT ( 'NONE',  ( -14.94248101481484170, 21.43223609974793220, 10.68306085400105587 ) ) ;
#5387 = ORIENTED_EDGE ( 'NONE', *, *, #1461, .T. ) ;
#5389 = CYLINDRICAL_SURFACE ( 'NONE', #23133, 1.000000000000000000 ) ;
#5388 = CARTESIAN_POINT ( 'NONE',  ( -10.97556112068393652, 17.46725186558634846, -28.07356528432091025 ) ) ;
#5390 = CARTESIAN_POINT ( 'NONE',  ( -15.33514102452888039, -26.41503892009194132, -7.825054394630688748 ) ) ;
#5391 = EDGE_CURVE ( 'NONE', #31473, #16736, #9901, .T. ) ;
#5392 = LINE ( 'NONE', #21037, #9419 ) ;
#5393 = VECTOR ( 'NONE', #29957, 1000.000000000000114 ) ;
#5394 = CARTESIAN_POINT ( 'NONE',  ( -29.61831833031994066, -15.50338790811805545, -12.89226513978680444 ) ) ;
#5395 = CARTESIAN_POINT ( 'NONE',  ( -9.262515494080826528, -25.37554028901857350, -6.432242585004741109 ) ) ;
#5396 = CARTESIAN_POINT ( 'NONE',  ( -24.49409870380021204, -11.70597971641812407, 20.99999999999999645 ) ) ;
#5397 = CARTESIAN_POINT ( 'NONE',  ( 12.48130235025789503, 18.13369772704632865, -22.85847515466027247 ) ) ;
#5399 = EDGE_CURVE ( 'NONE', #10247, #22927, #1272, .T. ) ;
#5398 = VERTEX_POINT ( 'NONE', #35399 ) ;
#5400 = CARTESIAN_POINT ( 'NONE',  ( 25.26210396730482444, 6.474115558529597081, -6.439678367293860894 ) ) ;
#5401 = LINE ( 'NONE', #17814, #15419 ) ;
#5402 = CARTESIAN_POINT ( 'NONE',  ( -3.100643064501314328, 15.70406341247269211, 13.00000000000000178 ) ) ;
#5403 = CARTESIAN_POINT ( 'NONE',  ( 7.766013557953383106, 28.81973365084986938, 10.50000000000000178 ) ) ;
#5404 = ORIENTED_EDGE ( 'NONE', *, *, #14822, .F. ) ;
#5405 = CARTESIAN_POINT ( 'NONE',  ( -31.59685791085809115, -0.8232729786593077081, -5.935614622407810792 ) ) ;
#5406 = VECTOR ( 'NONE', #1129, 1000.000000000000000 ) ;
#5407 = CARTESIAN_POINT ( 'NONE',  ( 22.23423511320995161, 0.6107731265070599491, -22.72817852523589011 ) ) ;
#5408 = ADVANCED_FACE ( 'NONE', ( #26044 ), #29269, .T. ) ;
#5409 = DIRECTION ( 'NONE',  ( -0.1045284632676569680, -0.9945218953682729568, 0.000000000000000000 ) ) ;
#5410 = CARTESIAN_POINT ( 'NONE',  ( 25.12105899710777024, -7.724472287617720312, 20.94377226548389004 ) ) ;
#5411 = CARTESIAN_POINT ( 'NONE',  ( 19.69645987729881043, 11.37175641224107814, -29.99999999999998579 ) ) ;
#5412 = AXIS2_PLACEMENT_3D ( 'NONE', #35894, #38937, #20461 ) ;
#5413 = CARTESIAN_POINT ( 'NONE',  ( 20.78821643698968913, -29.20280246618838049, 11.00000000000000000 ) ) ;
#5414 = STYLED_ITEM ( 'NONE', ( #13404 ), #23086 ) ;
#5415 = ORIENTED_EDGE ( 'NONE', *, *, #16560, .T. ) ;
#5416 = EDGE_CURVE ( 'NONE', #24423, #17070, #5259, .T. ) ;
#5417 = CYLINDRICAL_SURFACE ( 'NONE', #15195, 1.000000000000000000 ) ;
#5418 = ADVANCED_FACE ( 'NONE', ( #29303 ), #14057, .F. ) ;
#5419 = B_SPLINE_CURVE_WITH_KNOTS ( 'NONE', 3,
 ( #403, #26335, #22673, #4394, #23488, #20451, #35077, #22874, #28222, #7231, #20249, #1352, #28977, #25923, #38322, #16799, #13736, #26126, #38522, #35483 ),
 .UNSPECIFIED., .F., .F.,
 ( 4, 2, 1, 1, 1, 1, 1, 1, 2, 2, 2, 2, 4 ),
 ( 0.000000000000000000, 0.0009765625000000845678, 0.001953125000000169136, 0.003906250000000261943, 0.007812500000000300107, 0.01562500000000022551, 0.03125000000000022898, 0.06250000000000023592, 0.1250000000000001388, 0.2500000000000001665, 0.5000000000000001110, 0.7500000000000001110, 1.000000000000000000 ),
 .UNSPECIFIED. ) ;
#5420 = ADVANCED_FACE ( 'NONE', ( #13860 ), #34460, .T. ) ;
#5421 = CIRCLE ( 'NONE', #17795, 1.000000000000000000 ) ;
#5422 = DIRECTION ( 'NONE',  ( 1.000000000000000000, 0.000000000000000000, 0.000000000000000000 ) ) ;
#5423 = CARTESIAN_POINT ( 'NONE',  ( -8.559512017365658920, 19.71884705062586107, 12.00000000000000000 ) ) ;
#5424 = CARTESIAN_POINT ( 'NONE',  ( 0.2421583011816821618, 22.82788874588058547, -22.98502890671374033 ) ) ;
#5425 = CARTESIAN_POINT ( 'NONE',  ( -2.568190708544568768, 12.82247983807084957, 10.00000000000000000 ) ) ;
#5426 = FACE_OUTER_BOUND ( 'NONE', #21592, .T. ) ;
#5427 = FACE_OUTER_BOUND ( 'NONE', #27942, .T. ) ;
#5428 = CARTESIAN_POINT ( 'NONE',  ( 11.14716901145161643, 12.46304090461738667, 6.000000000000000000 ) ) ;
#5429 = CARTESIAN_POINT ( 'NONE',  ( 12.74038105676654631, 14.56698729810772264, 10.63089969389957545 ) ) ;
#5430 = DIRECTION ( 'NONE',  ( 0.000000000000000000, 0.000000000000000000, 1.000000000000000000 ) ) ;
#5431 = CARTESIAN_POINT ( 'NONE',  ( 13.25098614097699823, 25.59540253443141822, -13.36463472324928858 ) ) ;
#5432 = FACE_OUTER_BOUND ( 'NONE', #2471, .T. ) ;
#5433 = ORIENTED_EDGE ( 'NONE', *, *, #39892, .T. ) ;
#5435 = CARTESIAN_POINT ( 'NONE',  ( 13.63581098909226874, 27.45627467658428955, 7.500000000000000888 ) ) ;
#5434 = CARTESIAN_POINT ( 'NONE',  ( -19.07024319634674825, 16.49937253695148343, -7.903667226272353297 ) ) ;
#5436 = AXIS2_PLACEMENT_3D ( 'NONE', #36848, #21799, #34202 ) ;
#5437 = LINE ( 'NONE', #33682, #14673 ) ;
#5438 = CARTESIAN_POINT ( 'NONE',  ( 13.04810291801232047, -23.09410372734021877, -15.44714336548847911 ) ) ;
#5439 = LINE ( 'NONE', #5836, #8100 ) ;
#5440 = CARTESIAN_POINT ( 'NONE',  ( 10.95987886464238059, 17.32429135621979555, -29.34782466777161858 ) ) ;
#5441 = PLANE ( 'NONE',  #28293 ) ;
#5442 = CARTESIAN_POINT ( 'NONE',  ( 39.59914439537040209, -10.88071518964973805, 11.00000000000000178 ) ) ;
#5443 = EDGE_CURVE ( 'NONE', #32345, #22086, #17528, .T. ) ;
#5444 = AXIS2_PLACEMENT_3D ( 'NONE', #34904, #37751, #19455 ) ;
#5445 = CARTESIAN_POINT ( 'NONE',  ( -19.34051520155174941, -15.12089003882966054, -20.75336540952627118 ) ) ;
#5446 = CARTESIAN_POINT ( 'NONE',  ( 5.013169528391580698, -22.01313204235280452, -18.95530368308426716 ) ) ;
#5447 = CARTESIAN_POINT ( 'NONE',  ( 11.12785985892924678, 17.21691741209329862, -29.35143107680136865 ) ) ;
#5448 = ADVANCED_FACE ( 'NONE', ( #4314 ), #35604, .T. ) ;
#5449 = CARTESIAN_POINT ( 'NONE',  ( 21.64434010710703404, 12.04703973602239842, -5.483094818529050229 ) ) ;
#5450 = DIRECTION ( 'NONE',  ( 0.6691306063588570163, -0.7431448254773953543, 0.000000000000000000 ) ) ;
#5451 = CARTESIAN_POINT ( 'NONE',  ( -6.164342072519281679, 35.60899897206203235, -9.314755791877534108 ) ) ;
#5452 = VERTEX_POINT ( 'NONE', #1883 ) ;
#5453 = LINE ( 'NONE', #27383, #36484 ) ;
#5454 = ORIENTED_EDGE ( 'NONE', *, *, #16612, .F. ) ;
#5455 = CARTESIAN_POINT ( 'NONE',  ( -15.24159360913302841, 8.525723021988211414, 10.00000000000000000 ) ) ;
#5456 = CARTESIAN_POINT ( 'NONE',  ( 9.221287281574577221, 10.65863771052202935, 10.59344459855561738 ) ) ;
#5457 = CARTESIAN_POINT ( 'NONE',  ( -30.58060419123731677, 0.1872796535314501520, -6.417327285377274926 ) ) ;
#5458 = CARTESIAN_POINT ( 'NONE',  ( 34.93334028802587454, -11.69476465809384358, -7.578579032868311138 ) ) ;
#5459 = EDGE_LOOP ( 'NONE', ( #30077, #15142, #27697, #17278 ) ) ;
#5460 = CARTESIAN_POINT ( 'NONE',  ( 9.831584923911634633, 26.22020669908450330, 10.00000000000000000 ) ) ;
#5461 = EDGE_LOOP ( 'NONE', ( #23085, #2790, #25221, #22650, #9490 ) ) ;
#5462 = DIRECTION ( 'NONE',  ( 0.8660254037844424824, 0.4999999999999932832, 0.000000000000000000 ) ) ;
#5463 = CARTESIAN_POINT ( 'NONE',  ( 12.68475447279711510, 27.14725768220934299, 10.00000000000000000 ) ) ;
#5464 = AXIS2_PLACEMENT_3D ( 'NONE', #29508, #1685, #11031 ) ;
#5465 = DIRECTION ( 'NONE',  ( 0.9135454576425988682, -0.4067366430758048157, 0.000000000000000000 ) ) ;
#5466 = ORIENTED_EDGE ( 'NONE', *, *, #8665, .T. ) ;
#5467 = DIRECTION ( 'NONE',  ( -1.000000000000000000, 0.000000000000000000, 0.000000000000000000 ) ) ;
#5468 = FACE_OUTER_BOUND ( 'NONE', #34879, .T. ) ;
#5469 = CARTESIAN_POINT ( 'NONE',  ( -1.078765555139302945, 27.41260393370252402, 23.00000000000000000 ) ) ;
#5470 = CARTESIAN_POINT ( 'NONE',  ( 20.04635827611367205, 14.95022894506133859, -5.482161707068185841 ) ) ;
#5471 = CARTESIAN_POINT ( 'NONE',  ( 12.41906572600498926, 32.58765353250298347, -5.451709377992093764 ) ) ;
#5472 = EDGE_LOOP ( 'NONE', ( #4449, #8392, #18116, #11593, #2574 ) ) ;
#5473 = CARTESIAN_POINT ( 'NONE',  ( -22.38085876145960640, 10.82216326969894737, -5.000000000000000000 ) ) ;
#5474 = DIRECTION ( 'NONE',  ( 0.000000000000000000, 0.000000000000000000, 1.000000000000000000 ) ) ;
#5475 = CARTESIAN_POINT ( 'NONE',  ( 13.82587226056095986, 37.11292026376941777, 23.00000000000000000 ) ) ;
#5476 = CARTESIAN_POINT ( 'NONE',  ( 9.791560039807741589, -18.01123673837627592, -30.00000000000000000 ) ) ;
#5477 = CARTESIAN_POINT ( 'NONE',  ( -6.688306800005769048, 28.52217545723006609, 13.00000000000000178 ) ) ;
#5478 = CARTESIAN_POINT ( 'NONE',  ( 22.45323650136968396, -2.382502413133517738, -20.55760979252983134 ) ) ;
#5479 = CARTESIAN_POINT ( 'NONE',  ( -12.39277014389930720, 20.48808981389291972, -19.49672617547258113 ) ) ;
#5480 = CARTESIAN_POINT ( 'NONE',  ( -13.95730328712268253, -15.73161065168129191, -26.46684035671119872 ) ) ;
#5481 = CARTESIAN_POINT ( 'NONE',  ( 9.465041007626510350, -19.87709408547213030, -22.85921428194744109 ) ) ;
#5482 = DIRECTION ( 'NONE',  ( 0.000000000000000000, 0.000000000000000000, 1.000000000000000000 ) ) ;
#5483 = ORIENTED_EDGE ( 'NONE', *, *, #17328, .F. ) ;
#5484 = EDGE_CURVE ( 'NONE', #10090, #2692, #16956, .T. ) ;
#5485 = ORIENTED_EDGE ( 'NONE', *, *, #29461, .F. ) ;
#5486 = CARTESIAN_POINT ( 'NONE',  ( -8.292854476136895414, 20.68584148307280657, -23.41493881702373869 ) ) ;
#5487 = LINE ( 'NONE', #20139, #20468 ) ;
#5488 = LINE ( 'NONE', #20750, #28241 ) ;
#5489 = DIRECTION ( 'NONE',  ( 0.000000000000000000, 0.000000000000000000, 1.000000000000000000 ) ) ;
#5490 = EDGE_LOOP ( 'NONE', ( #692, #39856, #14190, #25497 ) ) ;
#5491 = CARTESIAN_POINT ( 'NONE',  ( 25.18250945046685985, 0.4325523370485113706, -17.44396110470962213 ) ) ;
#5492 = CARTESIAN_POINT ( 'NONE',  ( -8.737320611644010526, -1.152986690174108819, 7.499999999999999112 ) ) ;
#5493 = CARTESIAN_POINT ( 'NONE',  ( -0.01803903918367114056, 14.62372257652092422, 12.00000000000000000 ) ) ;
#5494 = ORIENTED_EDGE ( 'NONE', *, *, #8705, .F. ) ;
#5495 = CIRCLE ( 'NONE', #23004, 1.000000000000000888 ) ;
#5496 = CARTESIAN_POINT ( 'NONE',  ( -30.17422560392139630, 0.02279020665480178606, -8.767816438049354844 ) ) ;
#5497 = DIRECTION ( 'NONE',  ( -0.5000000000000038858, -0.8660254037844364872, 0.000000000000000000 ) ) ;
#5498 = EDGE_LOOP ( 'NONE', ( #30727, #32701 ) ) ;
#5499 = CARTESIAN_POINT ( 'NONE',  ( 20.36542025373884002, -2.868257021092958325, -28.57874933910315107 ) ) ;
#5500 = AXIS2_PLACEMENT_3D ( 'NONE', #17480, #17280, #32517 ) ;
#5501 = CARTESIAN_POINT ( 'NONE',  ( 24.49773858737317767, -28.07267629079924731, 13.92931973827831627 ) ) ;
#5502 = VERTEX_POINT ( 'NONE', #23408 ) ;
#5503 = CARTESIAN_POINT ( 'NONE',  ( -3.781581747449368258, 39.64129210796443914, 13.92931973827819903 ) ) ;
#5504 = LINE ( 'NONE', #10681, #33421 ) ;
#5505 = CARTESIAN_POINT ( 'NONE',  ( -5.644276917315532494, 36.40655018617699312, 10.50000000000000000 ) ) ;
#5506 = CARTESIAN_POINT ( 'NONE',  ( -4.721973484739690363, 30.34170004520404262, 20.50957957745984217 ) ) ;
#5507 = DIRECTION ( 'NONE',  ( 1.000000000000000000, 0.000000000000000000, 0.000000000000000000 ) ) ;
#5508 = VERTEX_POINT ( 'NONE', #32562 ) ;
#5509 = EDGE_CURVE ( 'NONE', #26584, #21822, #39643, .T. ) ;
#5510 = DIRECTION ( 'NONE',  ( 1.000000000000000000, 0.000000000000000000, 0.000000000000000000 ) ) ;
#5511 = DIRECTION ( 'NONE',  ( 0.000000000000000000, 0.000000000000000000, 1.000000000000000000 ) ) ;
#5512 = AXIS2_PLACEMENT_3D ( 'NONE', #13222, #32123, #13829 ) ;
#5513 = CARTESIAN_POINT ( 'NONE',  ( 3.643761437349164023, 22.44536600252848402, -23.06246887300423154 ) ) ;
#5514 = FACE_OUTER_BOUND ( 'NONE', #31260, .T. ) ;
#5515 = EDGE_CURVE ( 'NONE', #36822, #2452, #7958, .T. ) ;
#5516 = CARTESIAN_POINT ( 'NONE',  ( 13.32438941869560800, 7.692839817671511149, 20.94377226548378346 ) ) ;
#5517 = EDGE_CURVE ( 'NONE', #839, #22834, #26450, .T. ) ;
#5518 = CARTESIAN_POINT ( 'NONE',  ( 18.39798444451995607, -26.88534991441762756, -7.737902397617890671 ) ) ;
#5519 = DIRECTION ( 'NONE',  ( 1.000000000000000000, 0.000000000000000000, 0.000000000000000000 ) ) ;
#5520 = AXIS2_PLACEMENT_3D ( 'NONE', #7013, #19615, #7623 ) ;
#5521 = CARTESIAN_POINT ( 'NONE',  ( 8.118377661053324701, 10.47536095541698486, 7.000000000000000000 ) ) ;
#5522 = CARTESIAN_POINT ( 'NONE',  ( -0.6108529249776363246, 37.48755679569042343, 7.000000000000000000 ) ) ;
#5523 = ORIENTED_EDGE ( 'NONE', *, *, #11997, .F. ) ;
#5524 = CARTESIAN_POINT ( 'NONE',  ( 12.09121274333381990, 19.97150667970398530, -20.53287558875649665 ) ) ;
#5525 = ORIENTED_EDGE ( 'NONE', *, *, #337, .F. ) ;
#5526 = AXIS2_PLACEMENT_3D ( 'NONE', #5866, #39988, #27805 ) ;
#5527 = CARTESIAN_POINT ( 'NONE',  ( -11.97496251553392277, 18.63315434291826378, -22.78159754204189724 ) ) ;
#5528 = AXIS2_PLACEMENT_3D ( 'NONE', #40011, #33544, #33140 ) ;
#5529 = CARTESIAN_POINT ( 'NONE',  ( -16.41753675003402790, -23.14183271658250973, 19.27171037444156454 ) ) ;
#5530 = CARTESIAN_POINT ( 'NONE',  ( -14.19304739008513927, 26.58586953448673285, 10.94611345180490147 ) ) ;
#5531 = CARTESIAN_POINT ( 'NONE',  ( 11.09322631748854526, 17.29180187222242893, -28.71057073618882782 ) ) ;
#5532 = ORIENTED_EDGE ( 'NONE', *, *, #1324, .T. ) ;
#5533 = CARTESIAN_POINT ( 'NONE',  ( 26.99793250668803779, -15.97657516354929896, -14.72900161456918156 ) ) ;
#5534 = ORIENTED_EDGE ( 'NONE', *, *, #16258, .T. ) ;
#5536 = DIRECTION ( 'NONE',  ( 0.3535533905932645160, -0.6123724356958055726, 0.7071067811865425767 ) ) ;
#5535 = CARTESIAN_POINT ( 'NONE',  ( -10.99303974619111379, 18.28104912796820258, -24.97110850915958835 ) ) ;
#5537 = CARTESIAN_POINT ( 'NONE',  ( -17.22232769333860958, -27.00279332920328201, -6.390812999317612153 ) ) ;
#5538 = DIRECTION ( 'NONE',  ( -0.8090169943749510040, -0.5877852522924683631, -3.469446951953612611E-15 ) ) ;
#5539 = ORIENTED_EDGE ( 'NONE', *, *, #22163, .T. ) ;
#5540 = CARTESIAN_POINT ( 'NONE',  ( -22.93034800799257766, -8.692403048024743839, -20.77076282677819208 ) ) ;
#5541 = CARTESIAN_POINT ( 'NONE',  ( -9.270452999807254457, -18.33270093331148232, -28.71663414965336614 ) ) ;
#5542 = CARTESIAN_POINT ( 'NONE',  ( 31.08218589456564018, -27.68808744834087321, 22.99999999999905853 ) ) ;
#5543 = VERTEX_POINT ( 'NONE', #2082 ) ;
#5544 = CARTESIAN_POINT ( 'NONE',  ( 20.26233914688108229, 3.111977874782128506, -29.38369824820663467 ) ) ;
#5545 = FACE_OUTER_BOUND ( 'NONE', #14274, .T. ) ;
#5546 = EDGE_CURVE ( 'NONE', #18400, #8408, #39042, .T. ) ;
#5547 = CARTESIAN_POINT ( 'NONE',  ( 5.688300058587269170, 16.47782454277055564, 13.00000000000000178 ) ) ;
#5548 = EDGE_CURVE ( 'NONE', #11555, #28022, #9144, .T. ) ;
#5549 = ORIENTED_EDGE ( 'NONE', *, *, #25174, .F. ) ;
#5550 = CARTESIAN_POINT ( 'NONE',  ( -20.82302739279173664, 0.7399220483990450736, -26.82356524530285569 ) ) ;
#5551 = ORIENTED_EDGE ( 'NONE', *, *, #9813, .T. ) ;
#5552 = CARTESIAN_POINT ( 'NONE',  ( 31.66461267357289344, -1.371321637605815491, -7.774225005612001027 ) ) ;
#5553 = CARTESIAN_POINT ( 'NONE',  ( 34.49513285232596616, -12.61775564956195872, 17.42190598798392642 ) ) ;
#5554 = EDGE_LOOP ( 'NONE', ( #31328, #31703, #12353, #38632 ) ) ;
#5555 = CARTESIAN_POINT ( 'NONE',  ( -20.30511407948876013, 2.906241227738919353, -29.38143097496937273 ) ) ;
#5556 = AXIS2_PLACEMENT_3D ( 'NONE', #22014, #31953, #10023 ) ;
#5557 = DIRECTION ( 'NONE',  ( 0.000000000000000000, 0.000000000000000000, 1.000000000000000000 ) ) ;
#5558 = DIRECTION ( 'NONE',  ( 0.000000000000000000, 0.000000000000000000, 1.000000000000000000 ) ) ;
#5559 = CIRCLE ( 'NONE', #8137, 1.000000000000000888 ) ;
#5560 = VECTOR ( 'NONE', #5095, 1000.000000000000114 ) ;
#5561 = CARTESIAN_POINT ( 'NONE',  ( -16.80389827882203235, -21.64427909825945662, 19.99202127657104100 ) ) ;
#5562 = CARTESIAN_POINT ( 'NONE',  ( -8.927394655428429360, 11.06314620770957013, 11.00000000000000000 ) ) ;
#5563 = ADVANCED_FACE ( 'NONE', ( #19754 ), #32150, .F. ) ;
#5564 = FACE_BOUND ( 'NONE', #35416, .T. ) ;
#5565 = CARTESIAN_POINT ( 'NONE',  ( 14.47283171447379502, 21.48159823030311344, 7.000000000000000000 ) ) ;
#5566 = ORIENTED_EDGE ( 'NONE', *, *, #18532, .T. ) ;
#5567 = CARTESIAN_POINT ( 'NONE',  ( -25.37084529744385364, 6.201493023855051412, -7.401802512559587655 ) ) ;
#5568 = CARTESIAN_POINT ( 'NONE',  ( 8.843266739736572291, 16.81698729810774395, 10.50000000000000000 ) ) ;
#5569 = FACE_OUTER_BOUND ( 'NONE', #16070, .T. ) ;
#5570 = CARTESIAN_POINT ( 'NONE',  ( 24.58474773790242551, -25.53886705254056366, -8.487929553482985057 ) ) ;
#5571 = CARTESIAN_POINT ( 'NONE',  ( -8.633502029282189127, 11.46765470489704342, 7.499999999999999112 ) ) ;
#5572 = CARTESIAN_POINT ( 'NONE',  ( 14.36733273649021037, 25.42688099805458535, -11.56502463518844870 ) ) ;
#5573 = CARTESIAN_POINT ( 'NONE',  ( 15.07283634910031189, -28.35394831540551763, 13.32518128616608877 ) ) ;
#5574 = ORIENTED_EDGE ( 'NONE', *, *, #9889, .F. ) ;
#5575 = CARTESIAN_POINT ( 'NONE',  ( -16.67043351861327949, 21.32468196532498794, -9.304548275486963504 ) ) ;
#5576 = CARTESIAN_POINT ( 'NONE',  ( -25.74508372771330755, -9.012464122874943584, 20.94377226548387938 ) ) ;
#5577 = CARTESIAN_POINT ( 'NONE',  ( 10.36702044712426662, 31.16169077310587809, 7.000000000000000000 ) ) ;
#5578 = CARTESIAN_POINT ( 'NONE',  ( 15.11505727992676817, 26.09351122695967717, -8.768076250299181140 ) ) ;
#5579 = VERTEX_POINT ( 'NONE', #18516 ) ;
#5580 = CARTESIAN_POINT ( 'NONE',  ( 11.00500201062596517, 17.34882336543230252, -28.70691125584463421 ) ) ;
#5581 = ORIENTED_EDGE ( 'NONE', *, *, #7870, .F. ) ;
#5582 = AXIS2_PLACEMENT_3D ( 'NONE', #2644, #2451, #39611 ) ;
#5584 = FACE_OUTER_BOUND ( 'NONE', #27287, .T. ) ;
#5583 = CARTESIAN_POINT ( 'NONE',  ( -15.27621298814653805, 26.83222824197973111, -6.883326331195013026 ) ) ;
#5585 = CARTESIAN_POINT ( 'NONE',  ( -12.66759234962441205, -22.55799813172369284, -16.44235456654224592 ) ) ;
#5586 = CARTESIAN_POINT ( 'NONE',  ( -10.14717575287011542, 32.53695909538323860, 6.000000000000000000 ) ) ;
#5587 = VECTOR ( 'NONE', #3076, 1000.000000000000000 ) ;
#5588 = VECTOR ( 'NONE', #23769, 1000.000000000000114 ) ;
#5589 = CARTESIAN_POINT ( 'NONE',  ( -33.45162411266466762, -18.83634436166192572, -6.275798148608882521 ) ) ;
#5590 = CARTESIAN_POINT ( 'NONE',  ( -7.472041749460323068, -19.13836991950213928, -30.00000000000000000 ) ) ;
#5591 = CARTESIAN_POINT ( 'NONE',  ( 19.48557158514982746, -11.25000000000009415, 0.000000000000000000 ) ) ;
#5592 = CARTESIAN_POINT ( 'NONE',  ( 13.37849741503627321, 20.00359433874854886, -18.57205045318708514 ) ) ;
#5593 = VERTEX_POINT ( 'NONE', #11623 ) ;
#5594 = CARTESIAN_POINT ( 'NONE',  ( 19.15330224686634963, 7.305649259636135540, -29.42185863855868178 ) ) ;
#5595 = CIRCLE ( 'NONE', #28295, 5.999999999999994671 ) ;
#5596 = DIRECTION ( 'NONE',  ( -0.6724985119639655951, -0.2185080122244103806, -0.7071067811865396902 ) ) ;
#5597 = ADVANCED_FACE ( 'NONE', ( #36403 ), #2674, .T. ) ;
#5598 = CYLINDRICAL_SURFACE ( 'NONE', #18614, 59.99999999999995737 ) ;
#5599 = EDGE_CURVE ( 'NONE', #19098, #37418, #37000, .T. ) ;
#5600 = DIRECTION ( 'NONE',  ( 0.4999999999999920064, -0.8660254037844432595, 0.000000000000000000 ) ) ;
#5601 = VERTEX_POINT ( 'NONE', #2481 ) ;
#5602 = CARTESIAN_POINT ( 'NONE',  ( -31.20810765349570559, -1.166897260341405396, -8.705153276337458834 ) ) ;
#5603 = CARTESIAN_POINT ( 'NONE',  ( 23.33830534371964660, 0.4941299462022573086, -20.53406551574947159 ) ) ;
#5604 = LINE ( 'NONE', #33462, #15066 ) ;
#5605 = CARTESIAN_POINT ( 'NONE',  ( 23.05386822411317027, -7.747535282638454035, 20.99999999999999645 ) ) ;
#5606 = CARTESIAN_POINT ( 'NONE',  ( 18.07620401364302865, 24.68088026512193522, -5.000000000000000000 ) ) ;
#5607 = CARTESIAN_POINT ( 'NONE',  ( 14.09933648065468503, 26.02968990214155198, 11.00000000000000000 ) ) ;
#5608 = ORIENTED_EDGE ( 'NONE', *, *, #20532, .F. ) ;
#5609 = DIRECTION ( 'NONE',  ( -0.2876062384759389134, 0.6459741880212461762, -0.7071067811865567876 ) ) ;
#5610 = EDGE_CURVE ( 'NONE', #36997, #24077, #27059, .T. ) ;
#5611 = CARTESIAN_POINT ( 'NONE',  ( 6.431109915230138085, 35.71521269883979244, 10.96580508970282963 ) ) ;
#5612 = DIRECTION ( 'NONE',  ( -0.000000000000000000, 0.000000000000000000, -1.000000000000000000 ) ) ;
#5613 = CARTESIAN_POINT ( 'NONE',  ( 1.522946860592270912, 36.84862743726508683, -9.282692509776795831 ) ) ;
#5614 = LINE ( 'NONE', #2381, #982 ) ;
#5615 = VECTOR ( 'NONE', #40109, 1000.000000000000000 ) ;
#5616 = CARTESIAN_POINT ( 'NONE',  ( 10.54700836463452340, 22.39697303105787540, 10.50000000000000000 ) ) ;
#5617 = EDGE_CURVE ( 'NONE', #15610, #11440, #21553, .T. ) ;
#5618 = CARTESIAN_POINT ( 'NONE',  ( -14.52509594610762456, 21.97885917798744870, 7.500000000000004441 ) ) ;
#5619 = FACE_OUTER_BOUND ( 'NONE', #39417, .T. ) ;
#5620 = DIRECTION ( 'NONE',  ( 0.000000000000000000, 0.000000000000000000, -1.000000000000000000 ) ) ;
#5621 = DIRECTION ( 'NONE',  ( 0.000000000000000000, 0.000000000000000000, -1.000000000000000000 ) ) ;
#5622 = CARTESIAN_POINT ( 'NONE',  ( 14.70740557672079518, 28.82247346305062408, -4.999999999999998224 ) ) ;
#5623 = CARTESIAN_POINT ( 'NONE',  ( 3.835130509701798918, 15.55077355964573904, 12.00000000000000000 ) ) ;
#5624 = ORIENTED_EDGE ( 'NONE', *, *, #24737, .T. ) ;
#5626 = CARTESIAN_POINT ( 'NONE',  ( 13.16028273094469014, 27.30176617939681449, 9.500000000000000000 ) ) ;
#5625 = CARTESIAN_POINT ( 'NONE',  ( -15.95094248367131051, 12.99020724966809226, -28.27984824884035220 ) ) ;
#5627 = CARTESIAN_POINT ( 'NONE',  ( 4.706335727061685681, 24.35410196624994583, 13.00000000000000178 ) ) ;
#5628 = CARTESIAN_POINT ( 'NONE',  ( 14.62380663947432424, -25.46090403646468658, -10.65324618990382000 ) ) ;
#5629 = CARTESIAN_POINT ( 'NONE',  ( 13.20924685295715939, 22.23599012058760138, -16.44404666642637380 ) ) ;
#5630 = CARTESIAN_POINT ( 'NONE',  ( 11.28552181379516917, 18.05715790883359162, -25.01120835586647217 ) ) ;
#5631 = ORIENTED_EDGE ( 'NONE', *, *, #2415, .F. ) ;
#5632 = CARTESIAN_POINT ( 'NONE',  ( -25.71436706254305449, 9.015208126564347779, -5.000000000000000000 ) ) ;
#5633 = PLANE ( 'NONE',  #38885 ) ;
#5634 = CARTESIAN_POINT ( 'NONE',  ( -21.80912045058639137, -17.07601322584738668, -17.64863767831755226 ) ) ;
#5635 = CARTESIAN_POINT ( 'NONE',  ( -0.3892639042814902139, -24.76257045605676765, -5.967383921424669779 ) ) ;
#5636 = CARTESIAN_POINT ( 'NONE',  ( 14.28419796674242903, 23.34865556538064624, -13.54193682566124224 ) ) ;
#5637 = CARTESIAN_POINT ( 'NONE',  ( 21.09080728949390959, 11.74853788546874611, -10.88613492565143659 ) ) ;
#5638 = DIRECTION ( 'NONE',  ( -0.000000000000000000, -0.000000000000000000, -1.000000000000000000 ) ) ;
#5639 = CARTESIAN_POINT ( 'NONE',  ( -5.048995700102136830, 35.35551730485902766, -10.19541838177800308 ) ) ;
#5640 = ADVANCED_FACE ( 'NONE', ( #27651 ), #23806, .F. ) ;
#5641 = EDGE_LOOP ( 'NONE', ( #23166, #39721, #26480, #2895, #38662 ) ) ;
#5642 = EDGE_CURVE ( 'NONE', #14093, #28389, #1368, .T. ) ;
#5643 = VECTOR ( 'NONE', #3442, 1000.000000000000000 ) ;
#5644 = AXIS2_PLACEMENT_3D ( 'NONE', #19369, #35213, #19168 ) ;
#5645 = CARTESIAN_POINT ( 'NONE',  ( -28.74551992321994831, 4.923758765708712737, 12.14047268033756666 ) ) ;
#5646 = VERTEX_POINT ( 'NONE', #12014 ) ;
#5647 = FACE_OUTER_BOUND ( 'NONE', #8545, .T. ) ;
#5648 = FACE_OUTER_BOUND ( 'NONE', #15205, .T. ) ;
#5649 = CARTESIAN_POINT ( 'NONE',  ( -29.60162710802623565, 0.4573586862140032183, -9.245429160158396442 ) ) ;
#5650 = CARTESIAN_POINT ( 'NONE',  ( 35.51876124919839839, -10.74978321004375559, -5.441203547717361033 ) ) ;
#5651 = CIRCLE ( 'NONE', #31597, 0.5000000000000004441 ) ;
#5652 = ORIENTED_EDGE ( 'NONE', *, *, #17367, .F. ) ;
#5653 = ITEM_DEFINED_TRANSFORMATION ( 'NONE', 'NONE', #25528,  #24238 ) ;
#5654 = DIRECTION ( 'NONE',  ( 0.000000000000000000, 0.000000000000000000, 1.000000000000000000 ) ) ;
#5655 = ORIENTED_EDGE ( 'NONE', *, *, #6911, .F. ) ;
#5656 = CARTESIAN_POINT ( 'NONE',  ( 13.95683075005237050, 28.08631143191933432, 7.000000000000000000 ) ) ;
#5657 = CARTESIAN_POINT ( 'NONE',  ( -16.00000000000000000, 22.50000000000000711, 11.00000000000000178 ) ) ;
#5658 = EDGE_CURVE ( 'NONE', #14950, #31717, #8565, .T. ) ;
#5659 = CARTESIAN_POINT ( 'NONE',  ( -4.003793312560516071, 8.307369216259115063, 10.49999999999999822 ) ) ;
#5660 = EDGE_LOOP ( 'NONE', ( #1265, #23940, #6848, #24124 ) ) ;
#5661 = ADVANCED_FACE ( 'NONE', ( #6110 ), #20773, .T. ) ;
#5662 = CARTESIAN_POINT ( 'NONE',  ( -3.503793317224520365, 8.420815634768723967, 11.00000000000000000 ) ) ;
#5663 = CARTESIAN_POINT ( 'NONE',  ( -1.871208588069141143, 13.69667159339610762, 13.00000000000000178 ) ) ;
#5664 = DIRECTION ( 'NONE',  ( -0.1045284632676437703, 0.9945218953682745111, 0.000000000000000000 ) ) ;
#5665 = CARTESIAN_POINT ( 'NONE',  ( 28.80350438480166630, -23.56000536320865990, -7.566454254401802082 ) ) ;
#5666 = CARTESIAN_POINT ( 'NONE',  ( 19.54635772746084399, 15.94078878846792335, -5.000000000000000888 ) ) ;
#5667 = CIRCLE ( 'NONE', #5010, 0.5000000000000006661 ) ;
#5668 = CARTESIAN_POINT ( 'NONE',  ( 11.32514681141933544, 29.41259196502597462, -12.20161796427938405 ) ) ;
#5669 = AXIS2_PLACEMENT_3D ( 'NONE', #15191, #5450, #30033 ) ;
#5670 = VERTEX_POINT ( 'NONE', #27254 ) ;
#5671 = ADVANCED_FACE ( 'NONE', ( #33369 ), #27451, .F. ) ;
#5672 = CARTESIAN_POINT ( 'NONE',  ( -19.01626305010417539, 9.437311419952862934, -23.32612332779064701 ) ) ;
#5673 = DIRECTION ( 'NONE',  ( -1.000000000000000000, 0.000000000000000000, 0.000000000000000000 ) ) ;
#5674 = CYLINDRICAL_SURFACE ( 'NONE', #17931, 0.4999999999999995559 ) ;
#5675 = CARTESIAN_POINT ( 'NONE',  ( 11.68354902705863019, -20.96014224807484538, -19.47927830206757704 ) ) ;
#5676 = DIRECTION ( 'NONE',  ( 0.7431448254773953543, 0.6691306063588570163, 0.000000000000000000 ) ) ;
#5677 = CIRCLE ( 'NONE', #39403, 0.4999999999999995559 ) ;
#5678 = CARTESIAN_POINT ( 'NONE',  ( 19.69645987729881043, 11.37175641224107814, -29.99999999999998579 ) ) ;
#5679 = AXIS2_PLACEMENT_3D ( 'NONE', #17816, #20047, #35687 ) ;
#5680 = CARTESIAN_POINT ( 'NONE',  ( -11.45389309739204897, 18.46357293444315317, -23.84913706035775149 ) ) ;
#5681 = CARTESIAN_POINT ( 'NONE',  ( -24.27663368075341310, -25.65399678531768757, -8.493885956241761903 ) ) ;
#5682 = CARTESIAN_POINT ( 'NONE',  ( 12.06583107040341929, -23.04759528289364923, -15.51202566005124162 ) ) ;
#5683 = CARTESIAN_POINT ( 'NONE',  ( 11.61146752755227141, 31.78078372435978594, 10.49999999999999822 ) ) ;
#5684 = VERTEX_POINT ( 'NONE', #39837 ) ;
#5685 = ORIENTED_EDGE ( 'NONE', *, *, #2698, .F. ) ;
#5686 = CARTESIAN_POINT ( 'NONE',  ( -10.75718172855884802, 32.61644780836525115, -9.406819691704866315 ) ) ;
#5687 = ADVANCED_FACE ( 'NONE', ( #24403 ), #15640, .F. ) ;
#5688 = CARTESIAN_POINT ( 'NONE',  ( -3.914034194965524183, 30.06176806842423943, 9.000000000000001776 ) ) ;
#5689 = CARTESIAN_POINT ( 'NONE',  ( 5.947717410344610656, 34.62949535663720724, 9.500000000000000000 ) ) ;
#5690 = EDGE_CURVE ( 'NONE', #6428, #37593, #23447, .T. ) ;
#5691 = CARTESIAN_POINT ( 'NONE',  ( -9.221287281574664263, 10.65863771052210396, 10.49999999999999645 ) ) ;
#5692 = ORIENTED_EDGE ( 'NONE', *, *, #10041, .T. ) ;
#5693 = CARTESIAN_POINT ( 'NONE',  ( 29.53845057008524577, 0.1145761312098864948, -10.18194101559443077 ) ) ;
#5694 = DIRECTION ( 'NONE',  ( 1.000000000000000000, 0.000000000000000000, 0.000000000000000000 ) ) ;
#5695 = DIRECTION ( 'NONE',  ( -0.9135454576426004225, 0.4067366430758009854, 0.000000000000000000 ) ) ;
#5696 = AXIS2_PLACEMENT_3D ( 'NONE', #5037, #30231, #39960 ) ;
#5697 = ORIENTED_EDGE ( 'NONE', *, *, #38236, .F. ) ;
#5698 = CARTESIAN_POINT ( 'NONE',  ( -20.52651921773533417, 0.8666805026383144206, -28.70727906677954877 ) ) ;
#5699 = FACE_OUTER_BOUND ( 'NONE', #2209, .T. ) ;
#5700 = EDGE_LOOP ( 'NONE', ( #3466, #9802 ) ) ;
#5701 = CARTESIAN_POINT ( 'NONE',  ( 20.38971234282849565, -2.225416161360934897, -29.99999999999998579 ) ) ;
#5702 = CIRCLE ( 'NONE', #15417, 21.00000000000002842 ) ;
#5703 = CIRCLE ( 'NONE', #28404, 1.000000000000000000 ) ;
#5704 = CARTESIAN_POINT ( 'NONE',  ( 15.03860650580494074, -28.48662463501965192, 12.73282698324853257 ) ) ;
#5705 = ORIENTED_EDGE ( 'NONE', *, *, #17970, .T. ) ;
#5706 = CARTESIAN_POINT ( 'NONE',  ( -8.747212233150712279, 37.02488667718797899, 15.13084544680138954 ) ) ;
#5707 = AXIS2_PLACEMENT_3D ( 'NONE', #1219, #19494, #31888 ) ;
#5708 = CARTESIAN_POINT ( 'NONE',  ( 0.000000000000000000, 22.50000000000000355, 7.000000000000000000 ) ) ;
#5709 = PLANE ( 'NONE',  #18260 ) ;
#5710 = CARTESIAN_POINT ( 'NONE',  ( 8.883663045967715277, 28.52602195317101064, 19.99202127657103745 ) ) ;
#5711 = AXIS2_PLACEMENT_3D ( 'NONE', #17509, #24184, #11604 ) ;
#5712 = CARTESIAN_POINT ( 'NONE',  ( 1.828660225305861475, 9.087095699275852922, 9.500000000000000000 ) ) ;
#5713 = ORIENTED_EDGE ( 'NONE', *, *, #31638, .T. ) ;
#5714 = ADVANCED_FACE ( 'NONE', ( #17730 ), #30106, .T. ) ;
#5715 = DIRECTION ( 'NONE',  ( 0.000000000000000000, 0.000000000000000000, 1.000000000000000000 ) ) ;
#5716 = DIRECTION ( 'NONE',  ( 0.000000000000000000, 0.000000000000000000, 1.000000000000000000 ) ) ;
#5717 = CARTESIAN_POINT ( 'NONE',  ( 4.160566904805777178, 21.52518878017418658, -24.32380698736195512 ) ) ;
#5718 = FACE_OUTER_BOUND ( 'NONE', #31189, .T. ) ;
#5719 = CARTESIAN_POINT ( 'NONE',  ( 7.976544127178703647, 18.48053530960098811, 20.94377226548381898 ) ) ;
#5720 = CARTESIAN_POINT ( 'NONE',  ( 19.48118952213373234, -26.85980758568562266, -7.713377719299291613 ) ) ;
#5721 = FILL_AREA_STYLE_COLOUR ( '', #25548 ) ;
#5722 = CARTESIAN_POINT ( 'NONE',  ( 0.000000000000000000, 22.50000000000000355, 12.00000000000000000 ) ) ;
#5723 = DIRECTION ( 'NONE',  ( 0.000000000000000000, 0.000000000000000000, 1.000000000000000000 ) ) ;
#5724 = ORIENTED_EDGE ( 'NONE', *, *, #22456, .F. ) ;
#5725 = CARTESIAN_POINT ( 'NONE',  ( 11.43919839650344450, 18.47623239142585660, -23.84679931570577338 ) ) ;
#5726 = VECTOR ( 'NONE', #8095, 1000.000000000000114 ) ;
#5727 = ORIENTED_EDGE ( 'NONE', *, *, #34094, .T. ) ;
#5729 = VECTOR ( 'NONE', #15893, 1000.000000000000000 ) ;
#5728 = CARTESIAN_POINT ( 'NONE',  ( -15.40861458322169852, 26.71707234346735049, -5.946083594750080081 ) ) ;
#5730 = CARTESIAN_POINT ( 'NONE',  ( -16.05557028316514945, -24.54483004364971777, 18.42518152272108622 ) ) ;
#5731 = CARTESIAN_POINT ( 'NONE',  ( 15.27508919949933386, -26.56523461522311180, -6.888122384594280945 ) ) ;
#5732 = CARTESIAN_POINT ( 'NONE',  ( -14.42035624161473883, 26.65972665747678860, 10.49999999999999822 ) ) ;
#5733 = CARTESIAN_POINT ( 'NONE',  ( 14.35017349371148221, 24.32190247689503337, -12.55613400241091959 ) ) ;
#5734 = ORIENTED_EDGE ( 'NONE', *, *, #34833, .T. ) ;
#5735 = CARTESIAN_POINT ( 'NONE',  ( 31.27850618055397192, -21.17625281506686719, -7.548661271228884750 ) ) ;
#5736 = VERTEX_POINT ( 'NONE', #8769 ) ;
#5737 = AXIS2_PLACEMENT_3D ( 'NONE', #6256, #24349, #36748 ) ;
#5739 = CARTESIAN_POINT ( 'NONE',  ( 8.258442077957491634, 10.28257882428873771, 10.94387467463492136 ) ) ;
#5738 = CARTESIAN_POINT ( 'NONE',  ( -10.65603027360134902, 17.51308114404589844, -29.34127381359134290 ) ) ;
#5740 = CARTESIAN_POINT ( 'NONE',  ( -14.89315407779151101, -22.48991538682484048, -16.21632406099578105 ) ) ;
#5741 = CARTESIAN_POINT ( 'NONE',  ( -11.31392148919591811, 36.91540483778867099, -5.000000000000009770 ) ) ;
#5742 = AXIS2_PLACEMENT_3D ( 'NONE', #34487, #9505, #18651 ) ;
#5743 = ORIENTED_EDGE ( 'NONE', *, *, #12137, .F. ) ;
#5744 = CARTESIAN_POINT ( 'NONE',  ( -35.26882099528151571, -12.14860974803371008, -6.718074511898288748 ) ) ;
#5745 = CARTESIAN_POINT ( 'NONE',  ( -9.602157984762992982, -18.64544031278391856, -26.24206618660978307 ) ) ;
#5746 = CARTESIAN_POINT ( 'NONE',  ( 13.77067693704748308, 28.44713853003850801, 7.000000000000000000 ) ) ;
#5747 = ORIENTED_EDGE ( 'NONE', *, *, #37150, .F. ) ;
#5748 = CARTESIAN_POINT ( 'NONE',  ( 29.69046389894461413, 1.111644899601798020, -6.418887305067702442 ) ) ;
#5749 = CARTESIAN_POINT ( 'NONE',  ( -1.000000000000000000, 37.50000000000000711, 11.00000000000000000 ) ) ;
#5750 = CARTESIAN_POINT ( 'NONE',  ( -31.08218589456761549, -27.68808744834008451, 23.00000000000000000 ) ) ;
#5751 = EDGE_CURVE ( 'NONE', #4123, #29026, #18316, .T. ) ;
#5752 = ORIENTED_EDGE ( 'NONE', *, *, #10882, .F. ) ;
#5753 = CARTESIAN_POINT ( 'NONE',  ( -30.55268131219984795, -0.08272631737051794332, -7.824640561139657891 ) ) ;
#5754 = ORIENTED_EDGE ( 'NONE', *, *, #13036, .T. ) ;
#5755 = CARTESIAN_POINT ( 'NONE',  ( 26.35789183837046323, -0.5391633472264854010, -16.33873335832168294 ) ) ;
#5756 = CARTESIAN_POINT ( 'NONE',  ( 22.07432851697283382, -25.45711773545401613, 17.92354375535248323 ) ) ;
#5757 = ORIENTED_EDGE ( 'NONE', *, *, #26410, .T. ) ;
#5758 = CARTESIAN_POINT ( 'NONE',  ( -27.36767439016168169, 3.518543689082064496, -7.859504197288676330 ) ) ;
#5759 = ADVANCED_FACE ( 'NONE', ( #15262 ), #33566, .F. ) ;
#5760 = DIRECTION ( 'NONE',  ( -0.000000000000000000, -0.000000000000000000, -1.000000000000000000 ) ) ;
#5761 = CARTESIAN_POINT ( 'NONE',  ( 1.596172877504872689, 27.23837864096129735, 21.00000000000000355 ) ) ;
#5762 = VECTOR ( 'NONE', #32063, 1000.000000000000000 ) ;
#5763 = VECTOR ( 'NONE', #24118, 1000.000000000000000 ) ;
#5764 = DIRECTION ( 'NONE',  ( 1.000000000000000000, 0.000000000000000000, 0.000000000000000000 ) ) ;
#5765 = AXIS2_PLACEMENT_3D ( 'NONE', #2522, #14912, #33609 ) ;
#5766 = LINE ( 'NONE', #33420, #13656 ) ;
#5767 = AXIS2_PLACEMENT_3D ( 'NONE', #26246, #23204, #32559 ) ;
#5768 = FACE_BOUND ( 'NONE', #19749, .T. ) ;
#5769 = FACE_OUTER_BOUND ( 'NONE', #32262, .T. ) ;
#5770 = EDGE_LOOP ( 'NONE', ( #17945, #16997, #31115, #16326 ) ) ;
#5771 = CARTESIAN_POINT ( 'NONE',  ( -22.98333746671406175, 7.800124279482834488, -12.84308237461532087 ) ) ;
#5772 = DIRECTION ( 'NONE',  ( 5.027458560212894738E-15, -0.7071067811865500152, -0.7071067811865450192 ) ) ;
#5773 = EDGE_CURVE ( 'NONE', #39686, #4328, #28648, .T. ) ;
#5774 = CARTESIAN_POINT ( 'NONE',  ( -6.462764152204139023, 17.91932574235843134, 20.99999999999999289 ) ) ;
#5775 = CARTESIAN_POINT ( 'NONE',  ( 25.76273642380879991, -25.21432076522168941, -8.033030049480178292 ) ) ;
#5776 = DIRECTION ( 'NONE',  ( 0.000000000000000000, 0.000000000000000000, 1.000000000000000000 ) ) ;
#5777 = CARTESIAN_POINT ( 'NONE',  ( 14.92263478618264294, 26.27297000776338365, -9.223291497026121277 ) ) ;
#5778 = CARTESIAN_POINT ( 'NONE',  ( -15.12590024502445374, -28.14827041158513055, 13.92931973827808889 ) ) ;
#5779 = ORIENTED_EDGE ( 'NONE', *, *, #15719, .F. ) ;
#5780 = CARTESIAN_POINT ( 'NONE',  ( -15.86769938419567083, 19.96447385803967123, -13.70337137721306497 ) ) ;
#5781 = CARTESIAN_POINT ( 'NONE',  ( -27.79678266235375617, -11.09703717633735742, 20.69868183039817211 ) ) ;
#5782 = PLANE ( 'NONE',  #3609 ) ;
#5783 = CARTESIAN_POINT ( 'NONE',  ( 15.03495856122551189, 25.91540030226262914, -9.238980687715695694 ) ) ;
#5784 = ORIENTED_EDGE ( 'NONE', *, *, #38336, .F. ) ;
#5785 = CARTESIAN_POINT ( 'NONE',  ( 1.871201846650637046, 31.30332840660451765, 6.000000000000000000 ) ) ;
#5786 = ORIENTED_EDGE ( 'NONE', *, *, #35595, .F. ) ;
#5788 = CARTESIAN_POINT ( 'NONE',  ( 0.000000000000000000, 22.50000000000000355, 6.000000000000000000 ) ) ;
#5787 = CARTESIAN_POINT ( 'NONE',  ( -11.61453560076544633, 18.98021450145642675, -22.72268002348484117 ) ) ;
#5789 = CARTESIAN_POINT ( 'NONE',  ( -14.70220195220311687, -25.47735308124121900, -10.64826642331331463 ) ) ;
#5790 = CARTESIAN_POINT ( 'NONE',  ( -20.57674455326939267, 23.15285302515659893, 11.00000000000000000 ) ) ;
#5791 = AXIS2_PLACEMENT_3D ( 'NONE', #1894, #14271, #34861 ) ;
#5792 = VECTOR ( 'NONE', #11132, 1000.000000000000000 ) ;
#5793 = CARTESIAN_POINT ( 'NONE',  ( -33.36586913699030532, -18.78766072402438780, -6.696109138991947596 ) ) ;
#5794 = CARTESIAN_POINT ( 'NONE',  ( -13.49893695621550016, -25.67936680625057377, -9.257259980528091958 ) ) ;
#5795 = DIRECTION ( 'NONE',  ( 0.000000000000000000, -0.000000000000000000, 1.000000000000000000 ) ) ;
#5796 = CARTESIAN_POINT ( 'NONE',  ( 16.29902410653496148, 23.87181549541910641, -5.474405017214732716 ) ) ;
#5797 = ORIENTED_EDGE ( 'NONE', *, *, #32081, .F. ) ;
#5798 = CARTESIAN_POINT ( 'NONE',  ( 24.44976066607466336, 7.357379235516989802, -7.896790638060003253 ) ) ;
#5799 = EDGE_CURVE ( 'NONE', #33798, #21611, #22128, .T. ) ;
#5800 = DIRECTION ( 'NONE',  ( -0.9781476007338043566, 0.2079116908177658096, 0.000000000000000000 ) ) ;
#5801 = CARTESIAN_POINT ( 'NONE',  ( 15.01946716906679136, 1.539419383720357137, 23.00000000000000355 ) ) ;
#5802 = CARTESIAN_POINT ( 'NONE',  ( -22.37798348102460722, 33.25980436007204588, 7.000000000000000000 ) ) ;
#5803 = AXIS2_PLACEMENT_3D ( 'NONE', #18712, #24603, #22341 ) ;
#5804 = ORIENTED_EDGE ( 'NONE', *, *, #16052, .F. ) ;
#5805 = CARTESIAN_POINT ( 'NONE',  ( -29.80098406382914078, -1.038879420582270008, -11.50085024836739400 ) ) ;
#5806 = CARTESIAN_POINT ( 'NONE',  ( 23.99938430216166552, 0.3490643838479008942, -19.47749761754171516 ) ) ;
#5807 = DIRECTION ( 'NONE',  ( 0.4067366430758028728, 0.9135454576425997564, 0.000000000000000000 ) ) ;
#5808 = EDGE_CURVE ( 'NONE', #14858, #16847, #26300, .T. ) ;
#5809 = CARTESIAN_POINT ( 'NONE',  ( 22.68370119258272766, -18.87043823706619250, 20.69868183039780263 ) ) ;
#5810 = EDGE_CURVE ( 'NONE', #23095, #19744, #7857, .T. ) ;
#5811 = DIRECTION ( 'NONE',  ( -0.9135454576426029760, 0.4067366430757954898, 0.000000000000000000 ) ) ;
#5812 = CARTESIAN_POINT ( 'NONE',  ( 7.824485034907088021, 10.87986945260446170, 7.499999999999999112 ) ) ;
#5813 = ORIENTED_EDGE ( 'NONE', *, *, #35971, .F. ) ;
#5814 = CARTESIAN_POINT ( 'NONE',  ( 14.98803198171708218, 21.89746804854020112, 7.339470489435497846 ) ) ;
#5815 = VECTOR ( 'NONE', #36658, 1000.000000000000000 ) ;
#5816 = PLANE ( 'NONE',  #38295 ) ;
#5817 = DIRECTION ( 'NONE',  ( -0.6691306063588570163, 0.7431448254773952433, -0.000000000000000000 ) ) ;
#5818 = CARTESIAN_POINT ( 'NONE',  ( 1.749742296866609426, 24.60707399529504613, -20.70440855371920819 ) ) ;
#5819 = CARTESIAN_POINT ( 'NONE',  ( 15.02235689379175732, 21.92659494635341844, 7.000000000000000000 ) ) ;
#5820 = EDGE_CURVE ( 'NONE', #17915, #20949, #16274, .T. ) ;
#5821 = CARTESIAN_POINT ( 'NONE',  ( 8.118377661053324701, 10.47536095541698486, 7.500000000000000888 ) ) ;
#5822 = ADVANCED_FACE ( 'NONE', ( #31699 ), #25394, .F. ) ;
#5823 = LINE ( 'NONE', #18223, #14871 ) ;
#5824 = AXIS2_PLACEMENT_3D ( 'NONE', #22099, #6261, #15808 ) ;
#5825 = DIRECTION ( 'NONE',  ( 0.4067366430758009299, 0.9135454576426005335, 0.000000000000000000 ) ) ;
#5826 = CARTESIAN_POINT ( 'NONE',  ( 1.204925152852600378, 12.02153850147727887, 10.50000000000000000 ) ) ;
#5827 = CARTESIAN_POINT ( 'NONE',  ( -14.48927117870118408, -30.61587158504671180, 11.00000000000000000 ) ) ;
#5828 = CARTESIAN_POINT ( 'NONE',  ( 10.29438980144439419, 17.78647955463217301, -28.67741383145057199 ) ) ;
#5829 = CARTESIAN_POINT ( 'NONE',  ( -10.44103466624267185, 32.57396620494226624, 7.000000000000000000 ) ) ;
#5830 = ORIENTED_EDGE ( 'NONE', *, *, #27631, .T. ) ;
#5832 = PLANE ( 'NONE',  #3181 ) ;
#5831 = CARTESIAN_POINT ( 'NONE',  ( -18.73768915581330674, 17.66930787322032259, -4.999999999999999112 ) ) ;
#5833 = CARTESIAN_POINT ( 'NONE',  ( 7.293999462566144842, 11.53598992149257008, 12.00000000000000000 ) ) ;
#5834 = CARTESIAN_POINT ( 'NONE',  ( 15.32796092042050340, -26.50622118238649350, -7.357831815769672268 ) ) ;
#5835 = CARTESIAN_POINT ( 'NONE',  ( -22.76616367233569349, -26.90916104157130917, -5.891115712074672217 ) ) ;
#5836 = CARTESIAN_POINT ( 'NONE',  ( 14.84160187385922036, 20.32586711126977619, 7.500000000000010658 ) ) ;
#5837 = CARTESIAN_POINT ( 'NONE',  ( 14.92356852104117770, 25.83598546049896783, -9.706920252742902377 ) ) ;
#5838 = ORIENTED_EDGE ( 'NONE', *, *, #37633, .T. ) ;
#5839 = CARTESIAN_POINT ( 'NONE',  ( 9.163310636333564574, 20.63632441393291117, -29.99999999999999645 ) ) ;
#5840 = DIRECTION ( 'NONE',  ( -0.9781476007338043566, 0.2079116908177656708, 0.000000000000000000 ) ) ;
#5841 = CARTESIAN_POINT ( 'NONE',  ( -16.34560159223972065, -12.76520082579527404, -27.73245455758713618 ) ) ;
#5842 = CARTESIAN_POINT ( 'NONE',  ( 1.248574341839781221, -20.60364275570908532, -27.73818904947963304 ) ) ;
#5843 = CARTESIAN_POINT ( 'NONE',  ( 11.40065244407918144, 17.41857868398212972, -26.85574052250835919 ) ) ;
#5844 = CARTESIAN_POINT ( 'NONE',  ( 22.17839790455657933, 11.08535783459926094, -6.452902206156526432 ) ) ;
#5845 = CARTESIAN_POINT ( 'NONE',  ( 3.813962023474615215, 32.29559562678520024, 10.00000000000000000 ) ) ;
#5846 = CARTESIAN_POINT ( 'NONE',  ( -3.429749143149385837, 24.32645949754238046, -20.75053988368563651 ) ) ;
#5847 = ORIENTED_EDGE ( 'NONE', *, *, #39443, .T. ) ;
#5848 = CARTESIAN_POINT ( 'NONE',  ( -34.46511719672074747, -5.518907050001597092, -5.000000000000002665 ) ) ;
#5849 = ADVANCED_FACE ( 'NONE', ( #12411 ), #22544, .T. ) ;
#5850 = VECTOR ( 'NONE', #29858, 1000.000000000000000 ) ;
#5851 = CARTESIAN_POINT ( 'NONE',  ( -28.14004025859599878, 4.421764093230089010, 14.53008259254716705 ) ) ;
#5852 = ORIENTED_EDGE ( 'NONE', *, *, #31991, .F. ) ;
#5853 = DIRECTION ( 'NONE',  ( -0.000000000000000000, 0.000000000000000000, 1.000000000000000000 ) ) ;
#5854 = PLANE ( 'NONE',  #543 ) ;
#5855 = CARTESIAN_POINT ( 'NONE',  ( -26.72518533667481577, 0.8341530811610744500, -14.51637089005181203 ) ) ;
#5856 = CARTESIAN_POINT ( 'NONE',  ( 31.62610052856013709, -12.69311474474635482, -12.00053912072756646 ) ) ;
#5857 = ORIENTED_EDGE ( 'NONE', *, *, #32366, .T. ) ;
#5858 = DIRECTION ( 'NONE',  ( 0.000000000000000000, 0.000000000000000000, 1.000000000000000000 ) ) ;
#5859 = ORIENTED_EDGE ( 'NONE', *, *, #11260, .T. ) ;
#5860 = LINE ( 'NONE', #5656, #33992 ) ;
#5861 = DIRECTION ( 'NONE',  ( 1.000000000000000000, 0.000000000000000000, 0.000000000000000000 ) ) ;
#5862 = AXIS2_PLACEMENT_3D ( 'NONE', #21011, #18564, #36843 ) ;
#5863 = PLANE ( 'NONE',  #5824 ) ;
#5864 = ORIENTED_EDGE ( 'NONE', *, *, #27719, .F. ) ;
#5865 = CARTESIAN_POINT ( 'NONE',  ( -1.676223514573964568, 21.07032463922739751, -26.26967824088364267 ) ) ;
#5866 = CARTESIAN_POINT ( 'NONE',  ( 8.118377661053324701, 10.47536095541698486, 11.00000000000000000 ) ) ;
#5867 = DIRECTION ( 'NONE',  ( -0.6459741880212631626, 0.2876062384759295876, -0.7071067811865451302 ) ) ;
#5868 = DIRECTION ( 'NONE',  ( 0.000000000000000000, 0.000000000000000000, 1.000000000000000000 ) ) ;
#5869 = B_SPLINE_CURVE_WITH_KNOTS ( 'NONE', 3,
 ( #36475, #8643, #18389, #27526, #24280, #11890 ),
 .UNSPECIFIED., .F., .F.,
 ( 4, 2, 4 ),
 ( 0.000000000000000000, 0.5000000000000000000, 1.000000000000000000 ),
 .UNSPECIFIED. ) ;
#5870 = CARTESIAN_POINT ( 'NONE',  ( 29.22772011238637901, -23.88113300063707811, -5.863119439596483851 ) ) ;
#5871 = EDGE_CURVE ( 'NONE', #36923, #17177, #20845, .T. ) ;
#5872 = CARTESIAN_POINT ( 'NONE',  ( 19.51189016592634218, 15.90513825914224100, -6.448676663417378663 ) ) ;
#5873 = CARTESIAN_POINT ( 'NONE',  ( 11.78623425354685850, 30.69510100094851168, -10.36589696378858072 ) ) ;
#5874 = ORIENTED_EDGE ( 'NONE', *, *, #36728, .F. ) ;
#5875 = CARTESIAN_POINT ( 'NONE',  ( -18.53681031552473968, 9.242445014795279690, -26.61823075656795723 ) ) ;
#5876 = DIRECTION ( 'NONE',  ( 0.000000000000000000, 0.000000000000000000, 1.000000000000000000 ) ) ;
#5877 = CARTESIAN_POINT ( 'NONE',  ( 15.61814132907574759, -26.77569883083870650, -5.000000000000000888 ) ) ;
#5878 = CARTESIAN_POINT ( 'NONE',  ( 8.718266739736572291, 16.60048094716163192, 10.74999999999999467 ) ) ;
#5879 = VECTOR ( 'NONE', #27, 1000.000000000000000 ) ;
#5880 = CARTESIAN_POINT ( 'NONE',  ( -9.221287281574667816, 10.65863771052209863, 10.49999999999999822 ) ) ;
#5881 = CARTESIAN_POINT ( 'NONE',  ( -14.27740247628202397, 24.50748436584751744, -12.54751161500794510 ) ) ;
#5882 = CARTESIAN_POINT ( 'NONE',  ( -18.41842359106007265, -20.67470506895122995, -16.88471669450193957 ) ) ;
#5883 = CARTESIAN_POINT ( 'NONE',  ( 12.78458593907057050, -25.66269547989402611, -8.791706781336175780 ) ) ;
#5884 = CARTESIAN_POINT ( 'NONE',  ( -39.48557158258395816, -9.956519981528337837, 11.00000000000000178 ) ) ;
#5885 = ORIENTED_EDGE ( 'NONE', *, *, #22009, .F. ) ;
#5886 = ORIENTED_EDGE ( 'NONE', *, *, #18565, .F. ) ;
#5887 = CARTESIAN_POINT ( 'NONE',  ( -6.900714968323537590, 23.11544720565516187, -20.95321129010784844 ) ) ;
#5888 = CARTESIAN_POINT ( 'NONE',  ( -10.78894649379783388, 21.72623886970244911, 6.000000000000000000 ) ) ;
#5889 = EDGE_CURVE ( 'NONE', #24176, #25190, #11467, .T. ) ;
#5890 = DIRECTION ( 'NONE',  ( 0.4067366430758009854, 0.9135454576426005335, 0.000000000000000000 ) ) ;
#5891 = CARTESIAN_POINT ( 'NONE',  ( -9.608347198026818248, 2.148595524579384630, 11.00000000000000000 ) ) ;
#5892 = ORIENTED_EDGE ( 'NONE', *, *, #11685, .F. ) ;
#5893 = CARTESIAN_POINT ( 'NONE',  ( 30.85552734886118031, -0.02813967135195542812, -5.946081206346901737 ) ) ;
#5894 = ADVANCED_FACE ( 'NONE', ( #229 ), #34953, .T. ) ;
#5895 = CONICAL_SURFACE ( 'NONE', #707, 1.000000000000004441, 0.7853981633974583820 ) ;
#5896 = CARTESIAN_POINT ( 'NONE',  ( 1.732915686479641781, 38.50000000000001421, -5.000000000000000000 ) ) ;
#5897 = DIRECTION ( 'NONE',  ( -1.000000000000000000, 0.000000000000000000, 0.000000000000000000 ) ) ;
#5898 = ORIENTED_EDGE ( 'NONE', *, *, #8388, .T. ) ;
#5899 = CARTESIAN_POINT ( 'NONE',  ( -27.14151991403504738, 0.2337522234014248468, -14.47646250802335288 ) ) ;
#5900 = LINE ( 'NONE', #21735, #10549 ) ;
#5901 = ORIENTED_EDGE ( 'NONE', *, *, #36979, .T. ) ;
#5902 = CARTESIAN_POINT ( 'NONE',  ( 32.37911471581676182, -6.707950149574112508, -11.21564572321703324 ) ) ;
#5903 = EDGE_CURVE ( 'NONE', #13055, #35073, #31209, .T. ) ;
#5904 = VERTEX_POINT ( 'NONE', #21749 ) ;
#5905 = CARTESIAN_POINT ( 'NONE',  ( 14.73160032165944777, 32.49283138996950981, 12.73282698324854145 ) ) ;
#5906 = VECTOR ( 'NONE', #27405, 1000.000000000000000 ) ;
#5907 = CARTESIAN_POINT ( 'NONE',  ( 12.28720923547795429, -14.55658080553756406, 20.99999999999999645 ) ) ;
#5908 = FACE_BOUND ( 'NONE', #32186, .T. ) ;
#5909 = CARTESIAN_POINT ( 'NONE',  ( 6.000734348600325063, 30.39614672895685032, 20.25080042701566896 ) ) ;
#5910 = CARTESIAN_POINT ( 'NONE',  ( -6.577547685840081648, 11.84256962714647798, 6.000000000000000000 ) ) ;
#5911 = VERTEX_POINT ( 'NONE', #34156 ) ;
#5912 = LINE ( 'NONE', #12214, #4198 ) ;
#5913 = DIRECTION ( 'NONE',  ( -0.9510565162951503115, 0.3090169943749573878, 0.000000000000000000 ) ) ;
#5914 = EDGE_CURVE ( 'NONE', #17958, #9757, #13691, .T. ) ;
#5915 = EDGE_CURVE ( 'NONE', #36419, #16093, #5918, .T. ) ;
#5916 = EDGE_CURVE ( 'NONE', #29319, #2590, #24103, .T. ) ;
#5917 = CARTESIAN_POINT ( 'NONE',  ( 8.159785424745114923, 36.31054560068550785, -5.000000000000000000 ) ) ;
#5918 = CIRCLE ( 'NONE', #1402, 6.000000000000001776 ) ;
#5919 = LINE ( 'NONE', #18319, #10109 ) ;
#5920 = AXIS2_PLACEMENT_3D ( 'NONE', #28643, #6104, #30899 ) ;
#5921 = CARTESIAN_POINT ( 'NONE',  ( 18.30297387338707082, -26.76169866048132562, -8.193128520525432279 ) ) ;
#5922 = CARTESIAN_POINT ( 'NONE',  ( -5.400683141673551013, 15.91724817395922997, 9.000000000000001776 ) ) ;
#5923 = CARTESIAN_POINT ( 'NONE',  ( 37.48538792151179422, -11.24999995791135809, -5.000000000000002665 ) ) ;
#5924 = DIRECTION ( 'NONE',  ( 1.000000000000000000, 0.000000000000000000, 0.000000000000000000 ) ) ;
#5925 = EDGE_LOOP ( 'NONE', ( #38579, #33830 ) ) ;
#5926 = CARTESIAN_POINT ( 'NONE',  ( -11.34638386317097414, 17.63893688852765251, -26.24216709345637710 ) ) ;
#5927 = CARTESIAN_POINT ( 'NONE',  ( -28.09977684436795187, -21.02662082632541285, 18.87996532025785257 ) ) ;
#5928 = CARTESIAN_POINT ( 'NONE',  ( 15.10518904483066116, -26.35922348767928014, -7.828561976387642396 ) ) ;
#5929 = CIRCLE ( 'NONE', #12425, 1.000000000000004441 ) ;
#5930 = CARTESIAN_POINT ( 'NONE',  ( -12.41268156625113406, 18.79179606750104981, 6.000000000000000000 ) ) ;
#5931 = VERTEX_POINT ( 'NONE', #34550 ) ;
#5932 = ORIENTED_EDGE ( 'NONE', *, *, #21456, .F. ) ;
#5933 = CARTESIAN_POINT ( 'NONE',  ( -10.07426590969644309, 18.03558095023054975, -28.02002322309929028 ) ) ;
#5934 = CARTESIAN_POINT ( 'NONE',  ( -13.81792096330566544, -19.81716108706868340, -20.21201242374250739 ) ) ;
#5935 = EDGE_CURVE ( 'NONE', #7759, #14281, #9172, .T. ) ;
#5936 = CARTESIAN_POINT ( 'NONE',  ( -7.133890061153688400, 30.26901619224549123, 10.50000000000000000 ) ) ;
#5937 = ORIENTED_EDGE ( 'NONE', *, *, #33881, .F. ) ;
#5938 = CARTESIAN_POINT ( 'NONE',  ( -19.92632346219155437, -6.217451167954449964, -27.05300979642112935 ) ) ;
#5939 = CARTESIAN_POINT ( 'NONE',  ( -13.41747663621706899, -24.08286238317321093, -13.52655550282949726 ) ) ;
#5940 = DIRECTION ( 'NONE',  ( 0.000000000000000000, 0.000000000000000000, 1.000000000000000000 ) ) ;
#5941 = ORIENTED_EDGE ( 'NONE', *, *, #9645, .T. ) ;
#5942 = CARTESIAN_POINT ( 'NONE',  ( 30.37118094322071116, 0.2378720938948036268, -7.359078499018228747 ) ) ;
#5943 = EDGE_CURVE ( 'NONE', #22772, #22802, #22153, .T. ) ;
#5944 = LINE ( 'NONE', #9197, #20660 ) ;
#5945 = CARTESIAN_POINT ( 'NONE',  ( 1.838889047819958655, 31.15129278236397781, 7.000000000000000000 ) ) ;
#5946 = EDGE_LOOP ( 'NONE', ( #18149, #14637, #26187, #7315 ) ) ;
#5947 = CARTESIAN_POINT ( 'NONE',  ( -30.97418125221157226, -0.1138930278413792935, -5.473725232278036756 ) ) ;
#5948 = ORIENTED_EDGE ( 'NONE', *, *, #23308, .F. ) ;
#5949 = CARTESIAN_POINT ( 'NONE',  ( 31.47160406948570355, -0.9748322044563902944, -7.325666882419753279 ) ) ;
#5950 = CIRCLE ( 'NONE', #12414, 17.00000000000000000 ) ;
#5951 = CARTESIAN_POINT ( 'NONE',  ( 8.689152191311208639, -18.57991728069408310, -30.00000000000000711 ) ) ;
#5952 = CARTESIAN_POINT ( 'NONE',  ( 32.40618899211592918, -4.990034233201372516, 17.92354375535250810 ) ) ;
#5953 = ORIENTED_EDGE ( 'NONE', *, *, #28148, .F. ) ;
#5954 = CARTESIAN_POINT ( 'NONE',  ( -22.49929938967337151, 2.786806827506322470, -20.78965617405635413 ) ) ;
#5955 = DIRECTION ( 'NONE',  ( -0.000000000000000000, -0.000000000000000000, 1.000000000000000000 ) ) ;
#5956 = FACE_OUTER_BOUND ( 'NONE', #9030, .T. ) ;
#5957 = CARTESIAN_POINT ( 'NONE',  ( -35.70677476034837383, -3.361263978139850117, 11.00000000000007994 ) ) ;
#5958 = AXIS2_PLACEMENT_3D ( 'NONE', #794, #28226, #25777 ) ;
#5959 = CARTESIAN_POINT ( 'NONE',  ( -9.221287281574667816, 10.65863771052209863, 10.49999999999999822 ) ) ;
#5960 = FACE_BOUND ( 'NONE', #38459, .T. ) ;
#5961 = CARTESIAN_POINT ( 'NONE',  ( 17.34253826607180216, 27.32041144404034227, 11.00000000000000000 ) ) ;
#5962 = ORIENTED_EDGE ( 'NONE', *, *, #24166, .F. ) ;
#5963 = CARTESIAN_POINT ( 'NONE',  ( -24.38549669577123780, 7.057000079732201669, -9.358091487992030721 ) ) ;
#5964 = DIRECTION ( 'NONE',  ( 0.000000000000000000, 0.000000000000000000, 1.000000000000000000 ) ) ;
#5965 = CARTESIAN_POINT ( 'NONE',  ( 4.577399223880711965, 35.23960032125090436, 10.50000000000000000 ) ) ;
#5966 = CARTESIAN_POINT ( 'NONE',  ( 16.73819527976525734, -18.47801620150503155, -19.92011894488071277 ) ) ;
#5967 = ADVANCED_FACE ( 'NONE', ( #17281 ), #1629, .T. ) ;
#5968 = CYLINDRICAL_SURFACE ( 'NONE', #39070, 16.00000000000000000 ) ;
#5969 = CARTESIAN_POINT ( 'NONE',  ( 12.49158913934741655, 21.29194851371496355, -18.41699628959158019 ) ) ;
#5970 = ORIENTED_EDGE ( 'NONE', *, *, #19001, .F. ) ;
#5971 = CARTESIAN_POINT ( 'NONE',  ( -13.25082632412080486, 16.82596296396004831, -24.09658587792272399 ) ) ;
#5972 = CIRCLE ( 'NONE', #16358, 1.000000000000000888 ) ;
#5973 = CARTESIAN_POINT ( 'NONE',  ( -26.86294352747613345, -10.31366695439962911, 20.82122704794079837 ) ) ;
#5974 = CARTESIAN_POINT ( 'NONE',  ( -13.16028273094462975, 27.30176617939698147, 7.499999999999994671 ) ) ;
#5975 = CARTESIAN_POINT ( 'NONE',  ( 11.49677055501553724, 18.42658349193868972, -23.85584982804179432 ) ) ;
#5976 = ORIENTED_EDGE ( 'NONE', *, *, #1870, .T. ) ;
#5977 = DIRECTION ( 'NONE',  ( 1.000000000000000000, 0.000000000000000000, 0.000000000000000000 ) ) ;
#5978 = ORIENTED_EDGE ( 'NONE', *, *, #37651, .F. ) ;
#5980 = PLANE ( 'NONE',  #33511 ) ;
#5979 = CARTESIAN_POINT ( 'NONE',  ( -11.19568584489086049, 18.12681501478423840, -24.99883673433283704 ) ) ;
#5981 = CARTESIAN_POINT ( 'NONE',  ( -15.59933896205200377, -26.64557334028585345, -6.883330346584703108 ) ) ;
#5982 = CARTESIAN_POINT ( 'NONE',  ( -10.10646936306323340, 32.94553861768095970, 9.500000000000000000 ) ) ;
#5983 = CARTESIAN_POINT ( 'NONE',  ( -22.44268735423172245, -12.63924686016724941, -19.62614582209359426 ) ) ;
#5984 = CARTESIAN_POINT ( 'NONE',  ( -7.472041749460323068, -19.13836991950213928, -29.38556132742408877 ) ) ;
#5985 = CARTESIAN_POINT ( 'NONE',  ( -11.74460609746112461, 31.83082137946488643, 7.365559175140416137 ) ) ;
#5986 = CARTESIAN_POINT ( 'NONE',  ( 16.18953844785700724, 23.66664093688779857, -7.370953813631154539 ) ) ;
#5987 = ORIENTED_EDGE ( 'NONE', *, *, #34171, .F. ) ;
#5988 = CARTESIAN_POINT ( 'NONE',  ( 19.95141399716809971, 5.213180036295102404, -27.65625233026011642 ) ) ;
#5989 = CARTESIAN_POINT ( 'NONE',  ( -7.824485034907249670, 10.87986945260456295, 9.500000000000000000 ) ) ;
#5990 = AXIS2_PLACEMENT_3D ( 'NONE', #38978, #23342, #19893 ) ;
#5991 = CARTESIAN_POINT ( 'NONE',  ( 10.54146960747273987, 17.40487552589537401, 13.00000000000000178 ) ) ;
#5992 = CYLINDRICAL_SURFACE ( 'NONE', #496, 16.00000000000000000 ) ;
#5993 = EDGE_LOOP ( 'NONE', ( #18579, #29785 ) ) ;
#5994 = CARTESIAN_POINT ( 'NONE',  ( -29.19917547237594135, -0.9871674563434781335, -12.44351941946414186 ) ) ;
#5995 = B_SPLINE_CURVE_WITH_KNOTS ( 'NONE', 3,
 ( #7903, #20716, #33110, #20308, #14204, #32706 ),
 .UNSPECIFIED., .F., .F.,
 ( 4, 2, 4 ),
 ( 0.000000000000000000, 0.5000000000000000000, 1.000000000000000000 ),
 .UNSPECIFIED. ) ;
#5996 = CARTESIAN_POINT ( 'NONE',  ( 27.19236210036768853, 0.1635435777650698363, -14.46877011068446883 ) ) ;
#5997 = AXIS2_PLACEMENT_3D ( 'NONE', #38569, #8450, #20848 ) ;
#5998 = LINE ( 'NONE', #2371, #35164 ) ;
#5999 = CARTESIAN_POINT ( 'NONE',  ( 20.14416558653905298, -20.32661669692072692, 20.50957957746028626 ) ) ;
#6000 = ORIENTED_EDGE ( 'NONE', *, *, #36372, .T. ) ;
#6001 = FACE_OUTER_BOUND ( 'NONE', #32292, .T. ) ;
#6002 = DIRECTION ( 'NONE',  ( 0.000000000000000000, 0.000000000000000000, 1.000000000000000000 ) ) ;
#6003 = VECTOR ( 'NONE', #28500, 1000.000000000000000 ) ;
#6004 = ORIENTED_EDGE ( 'NONE', *, *, #13959, .F. ) ;
#6005 = CARTESIAN_POINT ( 'NONE',  ( 1.485571585149874529, -11.25000000000009415, 6.000000000000000000 ) ) ;
#6006 = CIRCLE ( 'NONE', #4060, 20.00000000000002842 ) ;
#6007 = AXIS2_PLACEMENT_3D ( 'NONE', #33427, #27309, #30366 ) ;
#6008 = CARTESIAN_POINT ( 'NONE',  ( -9.559512017365660697, 19.71884705062586107, 6.000000000000000000 ) ) ;
#6009 = CARTESIAN_POINT ( 'NONE',  ( 19.48557158514982746, -11.25000000000009415, 0.000000000000000000 ) ) ;
#6010 = CARTESIAN_POINT ( 'NONE',  ( 2.480770198683128314, 34.31368165843753104, -11.97966601863191727 ) ) ;
#6011 = DIRECTION ( 'NONE',  ( 0.9135454576426004225, -0.4067366430758009854, 0.000000000000000000 ) ) ;
#6012 = EDGE_CURVE ( 'NONE', #13640, #31127, #17073, .T. ) ;
#6013 = CARTESIAN_POINT ( 'NONE',  ( 15.41558956984165363, 26.78481017248027740, -5.000000000000000000 ) ) ;
#6014 = AXIS2_PLACEMENT_3D ( 'NONE', #23190, #17715, #30090 ) ;
#6015 = CARTESIAN_POINT ( 'NONE',  ( 5.564982403289711499, 13.56448261984367676, 10.74999999999999822 ) ) ;
#6016 = CARTESIAN_POINT ( 'NONE',  ( 6.557822374958318434, 35.99981354310111925, 10.50000000000000000 ) ) ;
#6017 = CARTESIAN_POINT ( 'NONE',  ( 14.11133924723984379, 27.61078317377175750, 7.000000000000000000 ) ) ;
#6018 = CARTESIAN_POINT ( 'NONE',  ( -9.762440214479841671, -29.39637225272702281, 11.00000000000000000 ) ) ;
#6019 = CARTESIAN_POINT ( 'NONE',  ( 12.50798833650853581, 22.32269140556257625, -17.34734744980223553 ) ) ;
#6020 = DIRECTION ( 'NONE',  ( -0.000000000000000000, -0.000000000000000000, -1.000000000000000000 ) ) ;
#6021 = ORIENTED_EDGE ( 'NONE', *, *, #37534, .T. ) ;
#6023 = DIRECTION ( 'NONE',  ( 0.000000000000000000, -0.000000000000000000, 1.000000000000000000 ) ) ;
#6022 = CARTESIAN_POINT ( 'NONE',  ( -15.42551642139064327, 13.50153766309080616, -29.41782492588997400 ) ) ;
#6024 = EDGE_CURVE ( 'NONE', #22329, #33038, #19546, .T. ) ;
#6025 = DIRECTION ( 'NONE',  ( 0.000000000000000000, 0.000000000000000000, 1.000000000000000000 ) ) ;
#6026 = CARTESIAN_POINT ( 'NONE',  ( 9.980411694245088228, -18.80811517553802403, -25.01294378247454731 ) ) ;
#6027 = EDGE_CURVE ( 'NONE', #14918, #32909, #20868, .T. ) ;
#6028 = CARTESIAN_POINT ( 'NONE',  ( -19.01564406110544780, -23.98128217660448769, -13.15021722355371558 ) ) ;
#6029 = CARTESIAN_POINT ( 'NONE',  ( 15.41558956916362000, 26.78481017491965233, -5.474206059968302895 ) ) ;
#6030 = CARTESIAN_POINT ( 'NONE',  ( 13.20015681812674835, 22.25288346174406939, -16.44192407539625478 ) ) ;
#6031 = ORIENTED_EDGE ( 'NONE', *, *, #15748, .F. ) ;
#6032 = DIRECTION ( 'NONE',  ( 1.000000000000000000, 0.000000000000000000, 0.000000000000000000 ) ) ;
#6033 = CARTESIAN_POINT ( 'NONE',  ( -9.477158523855607086, -18.22807322462275437, -28.70867440543207749 ) ) ;
#6034 = AXIS2_PLACEMENT_3D ( 'NONE', #31011, #34260, #30813 ) ;
#6035 = CARTESIAN_POINT ( 'NONE',  ( -36.79828514077309620, -9.052677438811558730, 13.92931973827808712 ) ) ;
#6036 = CARTESIAN_POINT ( 'NONE',  ( -29.27466627731137905, -22.93577986743095209, -7.990066130726534155 ) ) ;
#6037 = VECTOR ( 'NONE', #21169, 999.9999999999998863 ) ;
#6038 = CARTESIAN_POINT ( 'NONE',  ( -0.2746841415255591445, -20.81937890219735010, -25.51001604958610969 ) ) ;
#6039 = CARTESIAN_POINT ( 'NONE',  ( 13.97835894188113670, 22.95206721622837520, -14.50284002566557895 ) ) ;
#6040 = CARTESIAN_POINT ( 'NONE',  ( 21.44614852998417831, 11.94023807127892489, -8.409193133933671405 ) ) ;
#6041 = CARTESIAN_POINT ( 'NONE',  ( 11.60262927932680554, 31.67393310092480618, 10.49999999999999467 ) ) ;
#6042 = CARTESIAN_POINT ( 'NONE',  ( -5.242313593671260818, 36.85818054513828912, -7.989178582980050791 ) ) ;
#6043 = ORIENTED_EDGE ( 'NONE', *, *, #2575, .T. ) ;
#6044 = CARTESIAN_POINT ( 'NONE',  ( -26.02705243619845632, -4.035687289529959365, -17.97140994698204253 ) ) ;
#6045 = VECTOR ( 'NONE', #36098, 1000.000000000000000 ) ;
#6046 = CARTESIAN_POINT ( 'NONE',  ( -28.36971490935763640, 4.612181732483940699, 13.92931973828524406 ) ) ;
#6047 = ORIENTED_EDGE ( 'NONE', *, *, #11888, .T. ) ;
#6048 = DIRECTION ( 'NONE',  ( 0.000000000000000000, 0.000000000000000000, 1.000000000000000000 ) ) ;
#6049 = EDGE_CURVE ( 'NONE', #6207, #28039, #3968, .T. ) ;
#6050 = AXIS2_PLACEMENT_3D ( 'NONE', #6566, #34218, #37063 ) ;
#6051 = DIRECTION ( 'NONE',  ( 0.000000000000000000, 0.000000000000000000, 1.000000000000000000 ) ) ;
#6052 = EDGE_CURVE ( 'NONE', #39554, #28465, #37737, .T. ) ;
#6053 = CARTESIAN_POINT ( 'NONE',  ( -26.86592998902107254, 0.6294921843772121051, -14.50286829985886605 ) ) ;
#6054 = CARTESIAN_POINT ( 'NONE',  ( 35.02898577490625343, -14.10520536695887017, -6.707743114419838726 ) ) ;
#6055 = VERTEX_POINT ( 'NONE', #32715 ) ;
#6056 = CARTESIAN_POINT ( 'NONE',  ( -5.440908595777636414, 35.94977745735568675, 9.000000000000001776 ) ) ;
#6057 = ORIENTED_EDGE ( 'NONE', *, *, #26265, .F. ) ;
#6058 = DIRECTION ( 'NONE',  ( 0.000000000000000000, 0.000000000000000000, -1.000000000000000000 ) ) ;
#6059 = CARTESIAN_POINT ( 'NONE',  ( 4.817371740575477013, 23.83900317890016751, 23.00000000000000000 ) ) ;
#6060 = AXIS2_PLACEMENT_3D ( 'NONE', #34650, #19608, #6800 ) ;
#6061 = DIRECTION ( 'NONE',  ( -0.000000000000000000, -0.000000000000000000, -1.000000000000000000 ) ) ;
#6062 = ORIENTED_EDGE ( 'NONE', *, *, #24737, .F. ) ;
#6063 = CARTESIAN_POINT ( 'NONE',  ( -2.610469631123839118, 32.22098028545256199, -13.81657025006366446 ) ) ;
#6064 = DIRECTION ( 'NONE',  ( 0.000000000000000000, 0.000000000000000000, 1.000000000000000000 ) ) ;
#6065 = CARTESIAN_POINT ( 'NONE',  ( -12.30736835487442882, 14.81698729810789672, 7.000000000000000000 ) ) ;
#6066 = CARTESIAN_POINT ( 'NONE',  ( -6.706342468480190000, 20.64589803375067945, 12.00000000000000000 ) ) ;
#6067 = EDGE_CURVE ( 'NONE', #400, #28502, #13608, .T. ) ;
#6068 = CARTESIAN_POINT ( 'NONE',  ( 28.23949170197633052, -23.12056504026590886, -8.871261226031361247 ) ) ;
#6069 = CARTESIAN_POINT ( 'NONE',  ( 19.81566870575805694, 14.74257314966800081, -8.893701821489321091 ) ) ;
#6070 = CARTESIAN_POINT ( 'NONE',  ( 9.295215493701698861, 20.08986732679136011, -23.53424964172802092 ) ) ;
#6071 = ORIENTED_EDGE ( 'NONE', *, *, #9109, .F. ) ;
#6072 = CARTESIAN_POINT ( 'NONE',  ( -20.87549224088685662, 12.48772020076265754, -9.890582243910099436 ) ) ;
#6073 = CARTESIAN_POINT ( 'NONE',  ( 2.594149110900750177, 26.80855565015185249, 23.00000000000000000 ) ) ;
#6074 = PRODUCT_DEFINITION_FORMATION_WITH_SPECIFIED_SOURCE ( 'ANY', '', #13249, .NOT_KNOWN. ) ;
#6075 = CARTESIAN_POINT ( 'NONE',  ( 14.47998696515340100, -25.09368029485889906, -11.59030300758524135 ) ) ;
#6076 = DIRECTION ( 'NONE',  ( -0.000000000000000000, -0.000000000000000000, 1.000000000000000000 ) ) ;
#6077 = CARTESIAN_POINT ( 'NONE',  ( 5.636483973512840251, -22.01575377102106046, -21.50719306941234876 ) ) ;
#6078 = CARTESIAN_POINT ( 'NONE',  ( -15.08663340856853452, 26.18740194786823494, -8.765449597887428723 ) ) ;
#6079 = CIRCLE ( 'NONE', #15799, 6.000000000000005329 ) ;
#6080 = CARTESIAN_POINT ( 'NONE',  ( -24.80212611030263758, -26.15951744203449181, -6.747544335008610616 ) ) ;
#6081 = CARTESIAN_POINT ( 'NONE',  ( 8.268557591513960858, -18.75831942629880444, -29.37103518859555606 ) ) ;
#6082 = CARTESIAN_POINT ( 'NONE',  ( 11.17899463792469561, 31.89279561836804433, 10.99387789255783332 ) ) ;
#6083 = B_SPLINE_CURVE_WITH_KNOTS ( 'NONE', 3,
 ( #10890, #14528, #23672, #26922 ),
 .UNSPECIFIED., .F., .F.,
 ( 4, 4 ),
 ( 0.000000000000000000, 1.000000000000000000 ),
 .UNSPECIFIED. ) ;
#6084 = VERTEX_POINT ( 'NONE', #25994 ) ;
#6085 = CARTESIAN_POINT ( 'NONE',  ( -7.081591661052613951, 19.23835092891137322, -29.99999999999998579 ) ) ;
#6086 = CARTESIAN_POINT ( 'NONE',  ( 0.5000000000000000000, 37.50000000000000711, 10.59344459855570086 ) ) ;
#6087 = DIRECTION ( 'NONE',  ( 1.000000000000000000, 0.000000000000000000, 0.000000000000000000 ) ) ;
#6088 = VECTOR ( 'NONE', #31346, 1000.000000000000114 ) ;
#6089 = CARTESIAN_POINT ( 'NONE',  ( -9.428145666828269711, 11.00786382055651202, 10.49999999999999822 ) ) ;
#6090 = EDGE_LOOP ( 'NONE', ( #14692, #24896, #25411, #13591 ) ) ;
#6091 = CARTESIAN_POINT ( 'NONE',  ( 29.58630078773897054, 0.06066663492363379151, -10.18067296547992129 ) ) ;
#6092 = DIRECTION ( 'NONE',  ( 0.000000000000000000, 0.000000000000000000, 1.000000000000000000 ) ) ;
#6093 = FACE_OUTER_BOUND ( 'NONE', #6287, .T. ) ;
#6094 = EDGE_CURVE ( 'NONE', #19619, #37255, #31242, .T. ) ;
#6095 = B_SPLINE_SURFACE_WITH_KNOTS ( 'NONE', 1, 3, ( 
 ( #32576, #23012, #19977, #26870, #32375, #20385, #23224, #17141, #17543, #35414 ),
 ( #7777, #14277, #39259, #27072, #14070, #2097, #20786, #11438, #32985, #36023 ) ),
 .UNSPECIFIED., .F., .F., .F.,
 ( 2, 2 ),
 ( 4, 2, 2, 2, 4 ),
 ( 0.000000000000000000, 1.000000000000000000 ),
 ( 4.486555270693061814, 4.879254352391789951, 5.271953434090517199, 5.664652515789244447, 6.057351597487972583 ),
 .UNSPECIFIED. ) ;
#6096 = ORIENTED_EDGE ( 'NONE', *, *, #22508, .T. ) ;
#6097 = CARTESIAN_POINT ( 'NONE',  ( -24.53661879515770750, 0.4792651036289722333, -18.45743660045788559 ) ) ;
#6098 = CARTESIAN_POINT ( 'NONE',  ( 14.98890121934609532, -28.67928442654220333, 23.00000000000000000 ) ) ;
#6099 = ORIENTED_EDGE ( 'NONE', *, *, #33633, .T. ) ;
#6100 = CARTESIAN_POINT ( 'NONE',  ( 34.20650232967010851, -6.142903936528047559, -7.652713872589724353 ) ) ;
#6101 = ORIENTED_EDGE ( 'NONE', *, *, #14599, .T. ) ;
#6102 = CARTESIAN_POINT ( 'NONE',  ( 10.68781676061647978, 36.56370694841956492, 13.32518128616609054 ) ) ;
#6103 = CARTESIAN_POINT ( 'NONE',  ( 4.336808689942017736E-14, -13.77689918168226235, 20.99999999999999645 ) ) ;
#6104 = DIRECTION ( 'NONE',  ( 0.000000000000000000, 0.000000000000000000, 1.000000000000000000 ) ) ;
#6105 = CARTESIAN_POINT ( 'NONE',  ( -10.34254640628272348, 25.37474234119852667, 19.99202127657103389 ) ) ;
#6106 = CIRCLE ( 'NONE', #28817, 1.000000000000000000 ) ;
#6107 = CARTESIAN_POINT ( 'NONE',  ( 11.19134295108988830, 14.88397459621551100, 9.500000000000000000 ) ) ;
#6108 = ORIENTED_EDGE ( 'NONE', *, *, #8165, .F. ) ;
#6109 = DIRECTION ( 'NONE',  ( 1.000000000000000000, 0.000000000000000000, 0.000000000000000000 ) ) ;
#6110 = FACE_OUTER_BOUND ( 'NONE', #20420, .T. ) ;
#6111 = CARTESIAN_POINT ( 'NONE',  ( 12.56321727241651764, 14.36790371874248606, 10.49999999999999822 ) ) ;
#6112 = ADVANCED_FACE ( 'NONE', ( #20318 ), #4867, .T. ) ;
#6113 = CARTESIAN_POINT ( 'NONE',  ( 9.588950291932912151, 33.22059306543958712, -9.825194817494050881 ) ) ;
#6114 = CIRCLE ( 'NONE', #6687, 1.000000000000000888 ) ;
#6115 = EDGE_CURVE ( 'NONE', #16240, #30744, #35148, .T. ) ;
#6116 = DIRECTION ( 'NONE',  ( 0.000000000000000000, 0.000000000000000000, -1.000000000000000000 ) ) ;
#6117 = CARTESIAN_POINT ( 'NONE',  ( 17.48038917147502147, -27.01406049274763177, -6.846127207748655685 ) ) ;
#6118 = FACE_OUTER_BOUND ( 'NONE', #22718, .T. ) ;
#6119 = FACE_OUTER_BOUND ( 'NONE', #15682, .T. ) ;
#6120 = CARTESIAN_POINT ( 'NONE',  ( 1.400691654708310141, 37.43445890845833901, 7.000000000000000000 ) ) ;
#6121 = VECTOR ( 'NONE', #34118, 1000.000000000000000 ) ;
#6122 = ORIENTED_EDGE ( 'NONE', *, *, #21193, .F. ) ;
#6123 = CARTESIAN_POINT ( 'NONE',  ( -15.18846824274939245, 26.23493944448462045, -8.298081003141406953 ) ) ;
#6124 = EDGE_CURVE ( 'NONE', #13841, #26783, #37069, .T. ) ;
#6125 = CARTESIAN_POINT ( 'NONE',  ( -32.10122455788158646, -20.47530094824154645, 16.87380292611404897 ) ) ;
#6126 = CARTESIAN_POINT ( 'NONE',  ( 9.421039322076820710, -18.20697522973744498, -30.00000000000000000 ) ) ;
#6127 = DIRECTION ( 'NONE',  ( -0.7071067811865531239, 0.000000000000000000, -0.7071067811865417996 ) ) ;
#6128 = ORIENTED_EDGE ( 'NONE', *, *, #15043, .T. ) ;
#6129 = ORIENTED_EDGE ( 'NONE', *, *, #38612, .T. ) ;
#6130 = CARTESIAN_POINT ( 'NONE',  ( -13.84628348882036875, 30.44941459812471862, -5.912304033329754738 ) ) ;
#6131 = CARTESIAN_POINT ( 'NONE',  ( -18.93965825742197850, -26.62254513501367015, -8.625561435589691683 ) ) ;
#6132 = FACE_BOUND ( 'NONE', #19679, .T. ) ;
#6133 = AXIS2_PLACEMENT_3D ( 'NONE', #20317, #22950, #20520 ) ;
#6134 = ORIENTED_EDGE ( 'NONE', *, *, #22755, .F. ) ;
#6135 = CARTESIAN_POINT ( 'NONE',  ( -32.71841739113132519, -9.086232289925607830, -11.15351681095390113 ) ) ;
#6136 = UNCERTAINTY_MEASURE_WITH_UNIT (LENGTH_MEASURE( 1.000000000000000082E-05 ), #10558, 'distance_accuracy_value', 'NONE');
#6137 = CARTESIAN_POINT ( 'NONE',  ( -9.245064759184387526, -18.29713783020200424, -29.35345081433765202 ) ) ;
#6138 = CARTESIAN_POINT ( 'NONE',  ( 25.22779562677136767, -30.53001673900894630, 11.00000000000000000 ) ) ;
#6139 = ORIENTED_EDGE ( 'NONE', *, *, #26697, .F. ) ;
#6140 = CARTESIAN_POINT ( 'NONE',  ( 22.97385260750274227, 1.506209697923000634, -20.65583506744320985 ) ) ;
#6141 = CARTESIAN_POINT ( 'NONE',  ( 6.980762143445869761, 14.59310681135549537, 10.50000000000000000 ) ) ;
#6142 = DIRECTION ( 'NONE',  ( -0.000000000000000000, -0.000000000000000000, -1.000000000000000000 ) ) ;
#6143 = ADVANCED_FACE ( 'NONE', ( #1229 ), #10975, .F. ) ;
#6144 = VERTEX_POINT ( 'NONE', #4059 ) ;
#6145 = EDGE_CURVE ( 'NONE', #33348, #17668, #11118, .T. ) ;
#6146 = CARTESIAN_POINT ( 'NONE',  ( -30.64193714844549632, -0.04498350152496895238, -7.356955191584997777 ) ) ;
#6148 = ADVANCED_FACE ( 'NONE', ( #28849 ), #1025, .T. ) ;
#6147 = ORIENTED_EDGE ( 'NONE', *, *, #3550, .T. ) ;
#6149 = CARTESIAN_POINT ( 'NONE',  ( 27.27533884161622524, -0.9703114432050143900, -15.30757276055655858 ) ) ;
#6150 = DIRECTION ( 'NONE',  ( -1.000000000000000000, 0.000000000000000000, 0.000000000000000000 ) ) ;
#6151 = CARTESIAN_POINT ( 'NONE',  ( 17.31264644460116031, -26.16430884515622424, 17.42190598798342194 ) ) ;
#6152 = ORIENTED_EDGE ( 'NONE', *, *, #25524, .F. ) ;
#6153 = CARTESIAN_POINT ( 'NONE',  ( -20.18092276982249444, 3.603208870470906433, -29.38994685194823830 ) ) ;
#6154 = DIRECTION ( 'NONE',  ( 0.000000000000000000, 0.000000000000000000, 1.000000000000000000 ) ) ;
#6155 = VECTOR ( 'NONE', #18873, 1000.000000000000000 ) ;
#6156 = CARTESIAN_POINT ( 'NONE',  ( 4.706335727061685681, 24.35410196624994583, 12.00000000000000000 ) ) ;
#6157 = DIRECTION ( 'NONE',  ( -0.3535533905932657373, 0.6123724356957934711, 0.7071067811865525687 ) ) ;
#6158 = LINE ( 'NONE', #39882, #20167 ) ;
#6159 = PRESENTATION_LAYER_ASSIGNMENT (  '', '', ( #976 ) ) ;
#6160 = EDGE_CURVE ( 'NONE', #33983, #30328, #10567, .T. ) ;
#6161 = ADVANCED_FACE ( 'NONE', ( #35553 ), #4471, .F. ) ;
#6162 = AXIS2_PLACEMENT_3D ( 'NONE', #15361, #23708, #21261 ) ;
#6163 = DIRECTION ( 'NONE',  ( 0.000000000000000000, 0.000000000000000000, 1.000000000000000000 ) ) ;
#6164 = EDGE_CURVE ( 'NONE', #1059, #10078, #16669, .T. ) ;
#6165 = CARTESIAN_POINT ( 'NONE',  ( 18.50792845150514765, 22.38468038560473872, 12.73282698322912410 ) ) ;
#6166 = ORIENTED_EDGE ( 'NONE', *, *, #22769, .F. ) ;
#6167 = CARTESIAN_POINT ( 'NONE',  ( -22.41340355653765570, 7.689513575958383029, -14.86466521002182617 ) ) ;
#6168 = DIRECTION ( 'NONE',  ( 0.000000000000000000, 0.000000000000000000, 1.000000000000000000 ) ) ;
#6169 = LINE ( 'NONE', #9626, #29196 ) ;
#6170 = CARTESIAN_POINT ( 'NONE',  ( 17.99568451041676553, -19.86586605508433934, -17.85764876952420011 ) ) ;
#6171 = PLANE ( 'NONE',  #27412 ) ;
#6172 = CARTESIAN_POINT ( 'NONE',  ( 15.07891375406595458, 26.59690363730253893, -8.285697586515082591 ) ) ;
#6173 = ORIENTED_EDGE ( 'NONE', *, *, #6760, .F. ) ;
#6174 = CARTESIAN_POINT ( 'NONE',  ( -16.02335522834232506, 24.64807312034000120, -5.947261321558910296 ) ) ;
#6175 = CARTESIAN_POINT ( 'NONE',  ( -27.31543141964105104, -5.069059863655038356, 20.25080042701567606 ) ) ;
#6176 = LINE ( 'NONE', #40101, #39919 ) ;
#6177 = CARTESIAN_POINT ( 'NONE',  ( 11.10763664444189658, 17.47915243980666844, -27.45047991706941559 ) ) ;
#6178 = ORIENTED_EDGE ( 'NONE', *, *, #18412, .F. ) ;
#6179 = CARTESIAN_POINT ( 'NONE',  ( 11.44473057578109199, 31.45924896672603310, 7.499999999999997335 ) ) ;
#6180 = ORIENTED_EDGE ( 'NONE', *, *, #33279, .F. ) ;
#6182 = CARTESIAN_POINT ( 'NONE',  ( 6.686869517299636634, 14.99761530854296865, 10.49999999999999822 ) ) ;
#6181 = CARTESIAN_POINT ( 'NONE',  ( -14.63305198900928517, 25.70517243738389368, -10.63317628927790537 ) ) ;
#6183 = CARTESIAN_POINT ( 'NONE',  ( -13.84764258250596747, -24.13586365878463624, -13.50143806034850513 ) ) ;
#6184 = CARTESIAN_POINT ( 'NONE',  ( -13.26585111513660031, 17.86474508437623143, 6.000000000000000000 ) ) ;
#6185 = AXIS2_PLACEMENT_3D ( 'NONE', #14640, #8134, #26222 ) ;
#6186 = ORIENTED_EDGE ( 'NONE', *, *, #14285, .F. ) ;
#6187 = CARTESIAN_POINT ( 'NONE',  ( -18.80552062130275459, -9.155266005175258570, -26.97371384924871407 ) ) ;
#6188 = CARTESIAN_POINT ( 'NONE',  ( -9.109430062626294955, -21.71362431508917012, -18.71139059627909162 ) ) ;
#6189 = CARTESIAN_POINT ( 'NONE',  ( -11.94467491591058916, 31.57458037628605041, 7.130601027986743112 ) ) ;
#6190 = CARTESIAN_POINT ( 'NONE',  ( 12.12791028434681628, 17.37686543642602288, -25.11892433193763097 ) ) ;
#6191 = ORIENTED_EDGE ( 'NONE', *, *, #19850, .T. ) ;
#6192 = CARTESIAN_POINT ( 'NONE',  ( 19.64403038794415224, 5.908213622717613411, -30.00000000000000355 ) ) ;
#6193 = LINE ( 'NONE', #18599, #12831 ) ;
#6194 = CARTESIAN_POINT ( 'NONE',  ( 6.724523273151019609, 35.90846648263063656, 7.485699520496983617 ) ) ;
#6195 = CARTESIAN_POINT ( 'NONE',  ( -17.60052849889713400, -23.51059660007622298, -14.14515744745198056 ) ) ;
#6196 = ORIENTED_EDGE ( 'NONE', *, *, #36702, .T. ) ;
#6197 = CARTESIAN_POINT ( 'NONE',  ( -20.54774503203363878, -0.4733492751199910309, -28.65983527903481942 ) ) ;
#6198 = EDGE_CURVE ( 'NONE', #855, #4170, #8324, .T. ) ;
#6199 = CARTESIAN_POINT ( 'NONE',  ( 31.03926838894173557, -0.2887660594600527375, -6.411557450838987648 ) ) ;
#6200 = AXIS2_PLACEMENT_3D ( 'NONE', #21066, #36504, #18221 ) ;
#6201 = CIRCLE ( 'NONE', #9458, 0.5000000000000004441 ) ;
#6202 = CARTESIAN_POINT ( 'NONE',  ( -14.48927117870122316, -30.61587158504648087, 11.00000000000000000 ) ) ;
#6203 = CARTESIAN_POINT ( 'NONE',  ( 19.19128484611995944, -19.55740768895475767, 20.69868183039780618 ) ) ;
#6204 = ORIENTED_EDGE ( 'NONE', *, *, #5914, .F. ) ;
#6205 = DIRECTION ( 'NONE',  ( 0.000000000000000000, 0.000000000000000000, 1.000000000000000000 ) ) ;
#6206 = DIRECTION ( 'NONE',  ( 0.9781476007338042455, -0.2079116908177664480, 0.000000000000000000 ) ) ;
#6207 = VERTEX_POINT ( 'NONE', #33118 ) ;
#6208 = DIRECTION ( 'NONE',  ( 0.000000000000000000, 0.000000000000000000, 1.000000000000000000 ) ) ;
#6209 = APPLICATION_CONTEXT ( 'automotive_design' ) ;
#6210 = CYLINDRICAL_SURFACE ( 'NONE', #22090, 0.4999999999999989453 ) ;
#6211 = CARTESIAN_POINT ( 'NONE',  ( -9.541476348891238857, 27.59512447410525127, 13.00000000000000178 ) ) ;
#6212 = CARTESIAN_POINT ( 'NONE',  ( 1.681520345111361392, 23.68660416203806918, -21.85099733736959138 ) ) ;
#6213 = EDGE_CURVE ( 'NONE', #16505, #20763, #18074, .T. ) ;
#6214 = CARTESIAN_POINT ( 'NONE',  ( -6.658969205967785854, 35.40746193325465185, 10.66666666666666607 ) ) ;
#6215 = CARTESIAN_POINT ( 'NONE',  ( 5.187504188494417079, 36.60991850771481637, 11.00000000000000000 ) ) ;
#6216 = LINE ( 'NONE', #6999, #1947 ) ;
#6217 = DIRECTION ( 'NONE',  ( -0.4067366430758009299, -0.9135454576426005335, 0.000000000000000000 ) ) ;
#6218 = FACE_OUTER_BOUND ( 'NONE', #29570, .T. ) ;
#6219 = DIRECTION ( 'NONE',  ( 0.000000000000000000, 0.000000000000000000, 1.000000000000000000 ) ) ;
#6220 = CARTESIAN_POINT ( 'NONE',  ( 14.41569929962465046, 26.78900097671579772, -10.11187186520563053 ) ) ;
#6222 = VECTOR ( 'NONE', #25550, 1000.000000000000000 ) ;
#6221 = DIRECTION ( 'NONE',  ( 1.000000000000000000, 6.938893903907197612E-15, 0.000000000000000000 ) ) ;
#6223 = ORIENTED_EDGE ( 'NONE', *, *, #12112, .T. ) ;
#6226 = CIRCLE ( 'NONE', #20510, 1.000000000000000888 ) ;
#6225 = PLANE ( 'NONE',  #22630 ) ;
#6224 = CARTESIAN_POINT ( 'NONE',  ( -15.18347379343816961, 14.40797193047226621, -25.41007734764195902 ) ) ;
#6227 = CARTESIAN_POINT ( 'NONE',  ( -14.96930490892015797, 21.54088032874991399, 7.000000000000000000 ) ) ;
#6228 = AXIS2_PLACEMENT_3D ( 'NONE', #11133, #32477, #23521 ) ;
#6229 = CARTESIAN_POINT ( 'NONE',  ( 9.581194254144730138, -18.26805462278531778, -28.07681392454611213 ) ) ;
#6230 = CARTESIAN_POINT ( 'NONE',  ( -15.01668844516655099, -20.19012064364629566, -19.09890700679492426 ) ) ;
#6231 = CARTESIAN_POINT ( 'NONE',  ( 27.71565130972689772, -3.171757977843684628, 19.66345542862528717 ) ) ;
#6232 = CARTESIAN_POINT ( 'NONE',  ( 15.39471021437465659, 26.76682412655927124, -5.945909211790922910 ) ) ;
#6233 = VERTEX_POINT ( 'NONE', #5269 ) ;
#6234 = LINE ( 'NONE', #27968, #16615 ) ;
#6235 = CARTESIAN_POINT ( 'NONE',  ( -12.55455296433269297, -22.55646857384590120, -16.45145699756288593 ) ) ;
#6236 = CARTESIAN_POINT ( 'NONE',  ( -34.34163329534256803, -19.82715122747743308, 14.53008259254010959 ) ) ;
#6237 = CARTESIAN_POINT ( 'NONE',  ( -22.95124643118037611, -15.83345570903163946, -17.61049383489315900 ) ) ;
#6238 = CARTESIAN_POINT ( 'NONE',  ( -0.3452383396824790784, -23.23425136565043658, -14.92058295406784296 ) ) ;
#6239 = CARTESIAN_POINT ( 'NONE',  ( 15.62693799746092971, 26.04132429419060557, -5.474062535042302002 ) ) ;
#6240 = CARTESIAN_POINT ( 'NONE',  ( 18.23997498585743671, 9.357756550322328337, -29.99999999999999645 ) ) ;
#6241 = FACE_OUTER_BOUND ( 'NONE', #29455, .T. ) ;
#6242 = CARTESIAN_POINT ( 'NONE',  ( -2.977953329932500726, 21.20713377630406526, -25.62141012599427725 ) ) ;
#6243 = VERTEX_POINT ( 'NONE', #30465 ) ;
#6244 = CARTESIAN_POINT ( 'NONE',  ( -20.68522708307276048, -3.774204554019940705, -26.49279175686798382 ) ) ;
#6245 = CARTESIAN_POINT ( 'NONE',  ( -25.26292323897049030, 8.700328014641360852, 13.92931973827939096 ) ) ;
#6246 = VERTEX_POINT ( 'NONE', #39595 ) ;
#6247 = CARTESIAN_POINT ( 'NONE',  ( 7.917734535019441466, 14.47043272369397116, 12.00000000000000000 ) ) ;
#6248 = EDGE_CURVE ( 'NONE', #9203, #34232, #39391, .T. ) ;
#6249 = CARTESIAN_POINT ( 'NONE',  ( 0.000000000000000000, 22.50000000000000355, 6.000000000000000000 ) ) ;
#6250 = AXIS2_PLACEMENT_3D ( 'NONE', #15232, #27226, #15031 ) ;
#6251 = CARTESIAN_POINT ( 'NONE',  ( -30.08948457124776255, 0.6343089663011560742, -6.889917026222691199 ) ) ;
#6252 = B_SPLINE_CURVE_WITH_KNOTS ( 'NONE', 3,
 ( #27422, #5884, #18289, #6873, #25768, #10336, #3837, #3438, #37967, #6674 ),
 .UNSPECIFIED., .F., .F.,
 ( 4, 2, 2, 2, 4 ),
 ( 0.7014326804499604329, 0.7760745103374703247, 0.8507163402249802164, 0.9253581701124901082, 1.000000000000000000 ),
 .UNSPECIFIED. ) ;
#6253 = CARTESIAN_POINT ( 'NONE',  ( 31.79918597258268775, -11.65814279501285533, -12.01434721810185202 ) ) ;
#6254 = CIRCLE ( 'NONE', #14708, 1.000000000000000000 ) ;
#6255 = EDGE_LOOP ( 'NONE', ( #9151, #11650, #28622, #3994 ) ) ;
#6256 = CARTESIAN_POINT ( 'NONE',  ( 0.000000000000000000, 22.50000000000000355, 11.00000000000000178 ) ) ;
#6257 = VERTEX_POINT ( 'NONE', #2035 ) ;
#6258 = ADVANCED_FACE ( 'NONE', ( #11769 ), #11376, .T. ) ;
#6259 = LINE ( 'NONE', #6645, #7377 ) ;
#6260 = DIRECTION ( 'NONE',  ( 0.000000000000000000, 0.000000000000000000, 1.000000000000000000 ) ) ;
#6261 = DIRECTION ( 'NONE',  ( 0.000000000000000000, 0.000000000000000000, -1.000000000000000000 ) ) ;
#6262 = EDGE_LOOP ( 'NONE', ( #37176, #10694, #29267, #10179 ) ) ;
#6263 = CARTESIAN_POINT ( 'NONE',  ( -2.983151718949377695, 36.88695972035834103, -8.849962576356613653 ) ) ;
#6264 = CARTESIAN_POINT ( 'NONE',  ( 4.984135866956514782, 36.15314577889351000, 7.000000000000000000 ) ) ;
#6265 = DIRECTION ( 'NONE',  ( 0.000000000000000000, 0.000000000000000000, 1.000000000000000000 ) ) ;
#6266 = LINE ( 'NONE', #24957, #26673 ) ;
#6267 = CARTESIAN_POINT ( 'NONE',  ( 29.98328813315935193, -23.06114190392259289, -6.706346631438581340 ) ) ;
#6268 = CARTESIAN_POINT ( 'NONE',  ( 19.13006845375997500, 15.51315894313477983, -10.36673289579281310 ) ) ;
#6269 = CARTESIAN_POINT ( 'NONE',  ( 11.98624204988562880, 26.50047453519442087, -14.18334459157481220 ) ) ;
#6270 = ORIENTED_EDGE ( 'NONE', *, *, #12514, .F. ) ;
#6271 = CARTESIAN_POINT ( 'NONE',  ( -20.57814701393325763, 13.58265700682677135, -7.917366862160838181 ) ) ;
#6272 = LINE ( 'NONE', #27413, #2988 ) ;
#6273 = ADVANCED_FACE ( 'NONE', ( #33722 ), #33521, .T. ) ;
#6274 = CARTESIAN_POINT ( 'NONE',  ( 15.57999310324684394, -26.64107673304671664, -6.883736562959432703 ) ) ;
#6275 = DIRECTION ( 'NONE',  ( 0.000000000000000000, 0.000000000000000000, 1.000000000000000000 ) ) ;
#6276 = CARTESIAN_POINT ( 'NONE',  ( -20.55563217186184133, -29.52600041847739476, -4.999999999999992006 ) ) ;
#6277 = DIRECTION ( 'NONE',  ( 0.9135454576426050854, 0.4067366430757904938, 0.000000000000000000 ) ) ;
#6278 = CARTESIAN_POINT ( 'NONE',  ( -14.52059246409109328, 25.00446786749478179, -11.59653688421371065 ) ) ;
#6279 = CARTESIAN_POINT ( 'NONE',  ( -13.17255477323779544, -15.81076920432264110, -28.55881255893810078 ) ) ;
#6280 = CARTESIAN_POINT ( 'NONE',  ( 8.830897544850476066, -18.97134069234825304, -26.30954933935015916 ) ) ;
#6281 = CARTESIAN_POINT ( 'NONE',  ( -12.49038105676665644, 14.13397459621567798, 7.000000000000000000 ) ) ;
#6282 = ORIENTED_EDGE ( 'NONE', *, *, #22434, .F. ) ;
#6283 = CARTESIAN_POINT ( 'NONE',  ( -11.09255391874927099, 33.80179150524796228, -6.759096040517531989 ) ) ;
#6284 = CARTESIAN_POINT ( 'NONE',  ( 1.000000000000000222, 37.13089969389957901, 10.49999999999999822 ) ) ;
#6285 = LINE ( 'NONE', #3249, #4897 ) ;
#6286 = CARTESIAN_POINT ( 'NONE',  ( -8.954580980757368636, 11.02572744104269375, 10.99999999999999289 ) ) ;
#6287 = EDGE_LOOP ( 'NONE', ( #29533, #16880, #23140 ) ) ;
#6288 = CARTESIAN_POINT ( 'NONE',  ( 29.77530023422455230, 0.07316830583486964856, -9.709745822606079102 ) ) ;
#6289 = CARTESIAN_POINT ( 'NONE',  ( 14.95151364724920207, 28.45442998384968547, -4.999999999999999112 ) ) ;
#6290 = DIRECTION ( 'NONE',  ( 1.000000000000000000, 0.000000000000000000, 0.000000000000000000 ) ) ;
#6291 = ORIENTED_EDGE ( 'NONE', *, *, #1589, .F. ) ;
#6292 = CARTESIAN_POINT ( 'NONE',  ( -25.19426195496336263, 0.4106078367068997648, -17.44179917993732332 ) ) ;
#6293 = FACE_OUTER_BOUND ( 'NONE', #25742, .T. ) ;
#6294 = ORIENTED_EDGE ( 'NONE', *, *, #7647, .F. ) ;
#6295 = CARTESIAN_POINT ( 'NONE',  ( 22.74347250796713027, -4.688569809066241767, -22.15124392207232873 ) ) ;
#6296 = ORIENTED_EDGE ( 'NONE', *, *, #12097, .F. ) ;
#6297 = CARTESIAN_POINT ( 'NONE',  ( 14.84499459426748835, 32.56974970312070639, 12.14047268033098348 ) ) ;
#6298 = ADVANCED_FACE ( 'NONE', ( #11968 ), #26805, .F. ) ;
#6299 = CARTESIAN_POINT ( 'NONE',  ( 4.678013043399745996, 44.50832101651059958, 7.000000000000000000 ) ) ;
#6300 = CARTESIAN_POINT ( 'NONE',  ( -10.54147634889124063, 27.59512447410525127, 13.00000000000000178 ) ) ;
#6301 = CARTESIAN_POINT ( 'NONE',  ( 3.426866961292364788, 32.67295397237175081, 19.99202127657103034 ) ) ;
#6302 = VECTOR ( 'NONE', #25874, 1000.000000000000000 ) ;
#6303 = CONICAL_SURFACE ( 'NONE', #21252, 1.000000000000003553, 0.7853981633974514986 ) ;
#6304 = CARTESIAN_POINT ( 'NONE',  ( -13.63581098909220479, 27.45627467658446008, 11.00000000000000000 ) ) ;
#6305 = ORIENTED_EDGE ( 'NONE', *, *, #38945, .F. ) ;
#6306 = CARTESIAN_POINT ( 'NONE',  ( -2.247473515615844075, 16.63111439559750693, 6.000000000000000000 ) ) ;
#6307 = CARTESIAN_POINT ( 'NONE',  ( -10.10646936306323518, 32.94553861768095970, 10.49999999999999822 ) ) ;
#6308 = DIRECTION ( 'NONE',  ( 0.000000000000000000, 0.000000000000000000, 1.000000000000000000 ) ) ;
#6309 = AXIS2_PLACEMENT_3D ( 'NONE', #34637, #7396, #6789 ) ;
#6310 = DIRECTION ( 'NONE',  ( -0.5254827454987477386, 0.4731467892558253729, -0.7071067811865489050 ) ) ;
#6311 = AXIS2_PLACEMENT_3D ( 'NONE', #6799, #35051, #37891 ) ;
#6312 = CARTESIAN_POINT ( 'NONE',  ( 6.027897580125727295, 26.69635721636051073, -17.72624810141741492 ) ) ;
#6313 = EDGE_CURVE ( 'NONE', #8554, #32472, #760, .T. ) ;
#6314 = EDGE_CURVE ( 'NONE', #5046, #33648, #34492, .T. ) ;
#6315 = CARTESIAN_POINT ( 'NONE',  ( 12.89270566647465444, -19.40238606651385211, -21.34760501390315213 ) ) ;
#6316 = CARTESIAN_POINT ( 'NONE',  ( -11.11016527260153808, 31.83082137946488643, 9.000000000000001776 ) ) ;
#6317 = EDGE_LOOP ( 'NONE', ( #9893, #1133, #28953 ) ) ;
#6318 = CARTESIAN_POINT ( 'NONE',  ( -13.22900060383164522, 22.20087300463323743, -16.44710350152914557 ) ) ;
#6319 = CARTESIAN_POINT ( 'NONE',  ( -22.18736851772318275, -26.07761132199846443, 17.42190598798353562 ) ) ;
#6320 = CARTESIAN_POINT ( 'NONE',  ( 11.08661522344922190, -20.48618510043472085, -20.55290280245016632 ) ) ;
#6321 = DIRECTION ( 'NONE',  ( -0.000000000000000000, -0.000000000000000000, -1.000000000000000000 ) ) ;
#6322 = ORIENTED_EDGE ( 'NONE', *, *, #20212, .T. ) ;
#6323 = VERTEX_POINT ( 'NONE', #27010 ) ;
#6324 = CARTESIAN_POINT ( 'NONE',  ( -14.22743693889722394, 29.09337559512570692, -7.745675218731769007 ) ) ;
#6325 = CARTESIAN_POINT ( 'NONE',  ( -19.06118249889109606, -26.77635033892090632, -8.172094255800319118 ) ) ;
#6326 = FACE_BOUND ( 'NONE', #8981, .T. ) ;
#6327 = CIRCLE ( 'NONE', #25794, 0.5000000000000006661 ) ;
#6328 = AXIS2_PLACEMENT_3D ( 'NONE', #23887, #29787, #39121 ) ;
#6329 = VERTEX_POINT ( 'NONE', #11573 ) ;
#6330 = CARTESIAN_POINT ( 'NONE',  ( -33.38602273161038170, -9.282055417215806514, -10.25250355813210845 ) ) ;
#6331 = CARTESIAN_POINT ( 'NONE',  ( -15.26010364459756552, -26.56150138407807404, -6.888153286160101807 ) ) ;
#6332 = DIRECTION ( 'NONE',  ( -0.2079116908177518763, 0.9781476007338072431, -0.000000000000000000 ) ) ;
#6333 = VERTEX_POINT ( 'NONE', #23961 ) ;
#6334 = CARTESIAN_POINT ( 'NONE',  ( 30.29183792527964059, 0.1916456675836968604, -7.829246360666628490 ) ) ;
#6335 = DIRECTION ( 'NONE',  ( -1.000000000000000000, 0.000000000000000000, 0.000000000000000000 ) ) ;
#6336 = DIRECTION ( 'NONE',  ( -0.000000000000000000, -0.000000000000000000, -1.000000000000000000 ) ) ;
#6337 = VERTEX_POINT ( 'NONE', #36756 ) ;
#6338 = CARTESIAN_POINT ( 'NONE',  ( -30.81836931999540852, -0.05788259138545252813, -6.416469516946182949 ) ) ;
#6339 = B_SPLINE_CURVE_WITH_KNOTS ( 'NONE', 3,
 ( #34038, #37079, #25083, #700 ),
 .UNSPECIFIED., .F., .F.,
 ( 4, 4 ),
 ( 0.000000000000000000, 0.3333333336416847703 ),
 .UNSPECIFIED. ) ;
#6340 = ADVANCED_FACE ( 'NONE', ( #5468 ), #2626, .T. ) ;
#6341 = ORIENTED_EDGE ( 'NONE', *, *, #14642, .F. ) ;
#6342 = CARTESIAN_POINT ( 'NONE',  ( 28.89050959737125623, -1.486091803545947387, -13.35079000493364632 ) ) ;
#6343 = AXIS2_PLACEMENT_3D ( 'NONE', #33055, #14347, #11506 ) ;
#6344 = CARTESIAN_POINT ( 'NONE',  ( 11.64820663778509058, -16.88399544672437358, -29.99999999999998579 ) ) ;
#6345 = CARTESIAN_POINT ( 'NONE',  ( 31.84188463419212312, -5.263436490337560336, 18.42518152272108978 ) ) ;
#6346 = ORIENTED_EDGE ( 'NONE', *, *, #37332, .F. ) ;
#6347 = CARTESIAN_POINT ( 'NONE',  ( -26.73099083996467584, 4.407957416117326055, -7.387802156515522967 ) ) ;
#6348 = CARTESIAN_POINT ( 'NONE',  ( -16.77267017368471258, -29.13948811608345935, -5.000000000000002665 ) ) ;
#6349 = DIRECTION ( 'NONE',  ( 0.8660254037844425934, 0.4999999999999933942, 0.000000000000000000 ) ) ;
#6350 = FACE_OUTER_BOUND ( 'NONE', #26028, .T. ) ;
#6351 = CARTESIAN_POINT ( 'NONE',  ( -10.16521142134453548, 24.66068167190384841, 6.000000000000000000 ) ) ;
#6352 = B_SPLINE_CURVE_WITH_KNOTS ( 'NONE', 3,
 ( #9726, #19254, #22699, #3819, #22107, #37353 ),
 .UNSPECIFIED., .F., .F.,
 ( 4, 2, 4 ),
 ( 0.000000000000000000, 0.5000000000000000000, 1.000000000000000000 ),
 .UNSPECIFIED. ) ;
#6353 = CIRCLE ( 'NONE', #10933, 1.000000000000000888 ) ;
#6354 = CIRCLE ( 'NONE', #11569, 0.4999999999999995559 ) ;
#6355 = DIRECTION ( 'NONE',  ( 0.000000000000000000, 0.000000000000000000, 1.000000000000000000 ) ) ;
#6356 = FACE_OUTER_BOUND ( 'NONE', #12359, .T. ) ;
#6357 = CARTESIAN_POINT ( 'NONE',  ( -21.91272648427093372, 6.709759433590156696, -17.91613236003459519 ) ) ;
#6358 = FACE_OUTER_BOUND ( 'NONE', #3103, .T. ) ;
#6359 = CARTESIAN_POINT ( 'NONE',  ( 13.37378135583786332, 20.59160479820248923, 10.50000000000000000 ) ) ;
#6360 = CARTESIAN_POINT ( 'NONE',  ( 21.71680379357236745, -25.33241256410994069, -10.33255673083395543 ) ) ;
#6361 = AXIS2_PLACEMENT_3D ( 'NONE', #16965, #23454, #19805 ) ;
#6362 = FACE_OUTER_BOUND ( 'NONE', #34950, .T. ) ;
#6363 = ADVANCED_FACE ( 'NONE', ( #15217 ), #23758, .T. ) ;
#6364 = CARTESIAN_POINT ( 'NONE',  ( 15.00644039686974551, 26.44642701462099410, -8.754054474938953945 ) ) ;
#6365 = AXIS2_PLACEMENT_3D ( 'NONE', #23136, #35535, #4849 ) ;
#6366 = EDGE_LOOP ( 'NONE', ( #15007, #2713 ) ) ;
#6367 = CARTESIAN_POINT ( 'NONE',  ( -15.99501842261168427, 24.59332436110834408, -6.420401403374273563 ) ) ;
#6368 = CARTESIAN_POINT ( 'NONE',  ( -27.36681752352253127, -15.80023946406859636, 20.50957957746028626 ) ) ;
#6369 = DIRECTION ( 'NONE',  ( -0.000000000000000000, -0.000000000000000000, -1.000000000000000000 ) ) ;
#6370 = CARTESIAN_POINT ( 'NONE',  ( 14.85818005886212667, 25.55460827346378139, -10.18136880024061952 ) ) ;
#6371 = ORIENTED_EDGE ( 'NONE', *, *, #7043, .T. ) ;
#6372 = FACE_OUTER_BOUND ( 'NONE', #15095, .T. ) ;
#6373 = EDGE_LOOP ( 'NONE', ( #21439, #39227 ) ) ;
#6375 = PLANE ( 'NONE',  #9510 ) ;
#6374 = CARTESIAN_POINT ( 'NONE',  ( -11.79361442241011027, 19.48717355318980538, -21.59818088168338690 ) ) ;
#6376 = CARTESIAN_POINT ( 'NONE',  ( -9.782119759365757616, -18.39785806163243720, -26.82258960566558059 ) ) ;
#6377 = CARTESIAN_POINT ( 'NONE',  ( 14.96930490892014731, 21.54088032874976832, 7.000000000000000000 ) ) ;
#6378 = ORIENTED_EDGE ( 'NONE', *, *, #2425, .F. ) ;
#6379 = CARTESIAN_POINT ( 'NONE',  ( -31.29495162020109333, -14.00799367487466185, -11.98689060328322142 ) ) ;
#6380 = CARTESIAN_POINT ( 'NONE',  ( -8.378134998683849588, -20.54869970867327567, -21.89539286573533161 ) ) ;
#6381 = DIRECTION ( 'NONE',  ( -0.5254827454987652802, -0.4731467892558137156, -0.7071067811865435759 ) ) ;
#6382 = CARTESIAN_POINT ( 'NONE',  ( 13.09240611201286519, 16.96975280483636084, -24.07475001065767017 ) ) ;
#6383 = ORIENTED_EDGE ( 'NONE', *, *, #34050, .F. ) ;
#6384 = CARTESIAN_POINT ( 'NONE',  ( 26.01521168343815305, 5.578082495604143709, -5.000000000000002665 ) ) ;
#6385 = DIRECTION ( 'NONE',  ( -0.3090169943749465631, 0.9510565162951538642, 0.000000000000000000 ) ) ;
#6386 = CARTESIAN_POINT ( 'NONE',  ( 11.30736835487432224, 14.81698729810772619, 7.000000000000000000 ) ) ;
#6387 = CARTESIAN_POINT ( 'NONE',  ( 2.229431105722923245, 20.49260818092372460, 13.00000000000000178 ) ) ;
#6388 = VERTEX_POINT ( 'NONE', #39792 ) ;
#6389 = CARTESIAN_POINT ( 'NONE',  ( -24.72616565644901243, 0.08492666307556424876, -18.40537585932330700 ) ) ;
#6390 = ADVANCED_FACE ( 'NONE', ( #33320 ), #27605, .T. ) ;
#6392 = CARTESIAN_POINT ( 'NONE',  ( 21.30732809765730806, 0.5481137214583843287, -24.98958552468036132 ) ) ;
#6391 = VECTOR ( 'NONE', #16705, 1000.000000000000000 ) ;
#6393 = AXIS2_PLACEMENT_3D ( 'NONE', #19333, #35383, #7541 ) ;
#6394 = EDGE_CURVE ( 'NONE', #33574, #19822, #5950, .T. ) ;
#6395 = CARTESIAN_POINT ( 'NONE',  ( 24.27776115474282648, -18.04224162735242842, 20.69868183039762854 ) ) ;
#6396 = VERTEX_POINT ( 'NONE', #2429 ) ;
#6397 = AXIS2_PLACEMENT_3D ( 'NONE', #6056, #36945, #21497 ) ;
#6398 = CARTESIAN_POINT ( 'NONE',  ( 11.41987377193677489, -19.41918266173338026, -30.00000000000000000 ) ) ;
#6399 = DIRECTION ( 'NONE',  ( 1.000000000000000000, 0.000000000000000000, 0.000000000000000000 ) ) ;
#6400 = EDGE_CURVE ( 'NONE', #9314, #12011, #14818, .T. ) ;
#6401 = VERTEX_POINT ( 'NONE', #22297 ) ;
#6402 = CARTESIAN_POINT ( 'NONE',  ( -11.77091082532341204, 29.60251629318183575, 6.000000000000000000 ) ) ;
#6403 = DIRECTION ( 'NONE',  ( 0.000000000000000000, 0.000000000000000000, -1.000000000000000000 ) ) ;
#6404 = CARTESIAN_POINT ( 'NONE',  ( 9.734896950324680276, 32.61097331450140047, 9.500000000000000000 ) ) ;
#6405 = CARTESIAN_POINT ( 'NONE',  ( 1.554709515727994651, 21.96439674343446669, -24.23040823157819545 ) ) ;
#6406 = FACE_OUTER_BOUND ( 'NONE', #7619, .T. ) ;
#6407 = CARTESIAN_POINT ( 'NONE',  ( 8.910254037844365982, 17.93301270189218855, 10.50000000000000000 ) ) ;
#6408 = CARTESIAN_POINT ( 'NONE',  ( -13.63581098909220479, 27.45627467658446008, 9.000000000000001776 ) ) ;
#6409 = EDGE_CURVE ( 'NONE', #39958, #30975, #19060, .T. ) ;
#6410 = CYLINDRICAL_SURFACE ( 'NONE', #30311, 0.5000000000000011102 ) ;
#6411 = CARTESIAN_POINT ( 'NONE',  ( 12.80736835487433289, 15.68301270189216545, 7.000000000000000000 ) ) ;
#6412 = FACE_OUTER_BOUND ( 'NONE', #12569, .T. ) ;
#6413 = EDGE_CURVE ( 'NONE', #11960, #8101, #16215, .T. ) ;
#6414 = CIRCLE ( 'NONE', #34330, 1.000000000000000000 ) ;
#6415 = CARTESIAN_POINT ( 'NONE',  ( 11.65847521008705812, 20.47009998216675797, -20.44825086755248122 ) ) ;
#6416 = CARTESIAN_POINT ( 'NONE',  ( 13.28401428800400197, 15.85743772853274969, 10.49999999999999467 ) ) ;
#6417 = AXIS2_PLACEMENT_3D ( 'NONE', #31407, #12716, #33872 ) ;
#6418 = ORIENTED_EDGE ( 'NONE', *, *, #11517, .F. ) ;
#6420 = DIRECTION ( 'NONE',  ( 0.000000000000000000, 0.000000000000000000, 1.000000000000000000 ) ) ;
#6419 = CARTESIAN_POINT ( 'NONE',  ( -15.43930883336586035, 13.51924180792083519, -28.84025985046385898 ) ) ;
#6421 = PLANE ( 'NONE',  #27633 ) ;
#6422 = CARTESIAN_POINT ( 'NONE',  ( 12.28289708515961642, -22.02286693616888158, -17.43820040517785941 ) ) ;
#6423 = CARTESIAN_POINT ( 'NONE',  ( -12.22510872812234339, -16.67830574990779624, -27.92440097068585203 ) ) ;
#6424 = CARTESIAN_POINT ( 'NONE',  ( 12.13852697037936323, 19.91481632497913168, -20.54250373147018749 ) ) ;
#6425 = CARTESIAN_POINT ( 'NONE',  ( 11.10429069022538151, 17.62735859018268059, -26.82846151514053901 ) ) ;
#6426 = AXIS2_PLACEMENT_3D ( 'NONE', #10817, #22591, #35190 ) ;
#6427 = PRODUCT_DEFINITION_SHAPE ( 'NONE', 'NONE',  #32870 ) ;
#6428 = VERTEX_POINT ( 'NONE', #6851 ) ;
#6429 = DIRECTION ( 'NONE',  ( 0.5877852522924796874, 0.8090169943749426773, -0.000000000000000000 ) ) ;
#6430 = CARTESIAN_POINT ( 'NONE',  ( -10.78160465641473031, -20.00368079376380948, -21.62412776798347736 ) ) ;
#6431 = CARTESIAN_POINT ( 'NONE',  ( -16.90387162101869478, -28.96785393638790396, 12.73282698324800499 ) ) ;
#6432 = CARTESIAN_POINT ( 'NONE',  ( -25.08679319729055734, -18.48182376974868646, -14.75278769208404839 ) ) ;
#6433 = CARTESIAN_POINT ( 'NONE',  ( -0.2923764691290959283, -21.41221548788711360, -22.24809644302292710 ) ) ;
#6434 = CARTESIAN_POINT ( 'NONE',  ( 15.50648612925562375, 25.79783529730770653, -7.360586758651527006 ) ) ;
#6435 = CARTESIAN_POINT ( 'NONE',  ( 22.06023045062189425, 11.03359190991180938, -7.916614531392779597 ) ) ;
#6436 = LINE ( 'NONE', #9703, #36160 ) ;
#6437 = ORIENTED_EDGE ( 'NONE', *, *, #3414, .T. ) ;
#6438 = CARTESIAN_POINT ( 'NONE',  ( -27.56931151251565026, -3.500274113982246860, -16.06196160150427588 ) ) ;
#6439 = EDGE_CURVE ( 'NONE', #6492, #25420, #28198, .T. ) ;
#6440 = CARTESIAN_POINT ( 'NONE',  ( -18.23687175285704853, 10.52906281568731472, 19.27171037444156454 ) ) ;
#6441 = VERTEX_POINT ( 'NONE', #18666 ) ;
#6442 = ADVANCED_FACE ( 'NONE', ( #15413 ), #18469, .T. ) ;
#6443 = PLANE ( 'NONE',  #30410 ) ;
#6444 = DIRECTION ( 'NONE',  ( -0.6345370204114130219, -0.5138379476002922219, 0.5773502691896190697 ) ) ;
#6445 = CARTESIAN_POINT ( 'NONE',  ( -20.76830098884414966, 1.334683384510298110, -26.86827762553903298 ) ) ;
#6446 = CARTESIAN_POINT ( 'NONE',  ( 19.60222645149177367, -7.245507050130505888, -27.01638570009309248 ) ) ;
#6447 = CARTESIAN_POINT ( 'NONE',  ( 36.59387134601873726, -14.69446750445110794, 13.92931973827808712 ) ) ;
#6448 = AXIS2_PLACEMENT_3D ( 'NONE', #4161, #13706, #32414 ) ;
#6449 = ORIENTED_EDGE ( 'NONE', *, *, #8283, .F. ) ;
#6450 = DIRECTION ( 'NONE',  ( -0.000000000000000000, -0.000000000000000000, -1.000000000000000000 ) ) ;
#6451 = ORIENTED_EDGE ( 'NONE', *, *, #11413, .F. ) ;
#6452 = VECTOR ( 'NONE', #7909, 1000.000000000000000 ) ;
#6453 = CARTESIAN_POINT ( 'NONE',  ( -2.494943660522439099, 10.76222879119470832, 13.00000000000000178 ) ) ;
#6454 = DIRECTION ( 'NONE',  ( 0.000000000000000000, 0.000000000000000000, -1.000000000000000000 ) ) ;
#6455 = CARTESIAN_POINT ( 'NONE',  ( -9.331903152615899089, 11.35703883385581037, 10.50000000000000533 ) ) ;
#6456 = ORIENTED_EDGE ( 'NONE', *, *, #9882, .T. ) ;
#6457 = CARTESIAN_POINT ( 'NONE',  ( -4.095232911848371238, 36.67075768270702696, -8.855017135934939887 ) ) ;
#6458 = DIRECTION ( 'NONE',  ( 1.000000000000000000, 0.000000000000000000, -0.000000000000000000 ) ) ;
#6459 = DIRECTION ( 'NONE',  ( -0.000000000000000000, -0.000000000000000000, -1.000000000000000000 ) ) ;
#6460 = DIRECTION ( 'NONE',  ( 1.000000000000000000, 0.000000000000000000, 0.000000000000000000 ) ) ;
#6461 = DIRECTION ( 'NONE',  ( -1.000000000000000000, 0.000000000000000000, 0.000000000000000000 ) ) ;
#6462 = CARTESIAN_POINT ( 'NONE',  ( 2.525645716490524606, 8.212903943950921715, 11.00000000000000000 ) ) ;
#6463 = CARTESIAN_POINT ( 'NONE',  ( 8.682226116870198851, 18.58302833326690262, -29.30013558004020524 ) ) ;
#6464 = ORIENTED_EDGE ( 'NONE', *, *, #12704, .T. ) ;
#6465 = CARTESIAN_POINT ( 'NONE',  ( -17.67601262323927713, 10.51340875361112559, -28.30043818710294801 ) ) ;
#6466 = CARTESIAN_POINT ( 'NONE',  ( -13.82587226055908758, 37.11292026377122255, 11.00000000000000000 ) ) ;
#6467 = CARTESIAN_POINT ( 'NONE',  ( 9.643767478264347659, -18.09000205506835712, -30.00000000000000000 ) ) ;
#6468 = LINE ( 'NONE', #31461, #14608 ) ;
#6469 = EDGE_CURVE ( 'NONE', #28502, #34986, #3224, .T. ) ;
#6470 = CARTESIAN_POINT ( 'NONE',  ( 13.45860491773726153, 22.88270912621719688, -15.44303183026240944 ) ) ;
#6471 = CARTESIAN_POINT ( 'NONE',  ( -15.72991998290134141, -16.18894361744923316, -30.00000000000001421 ) ) ;
#6472 = DIRECTION ( 'NONE',  ( 0.000000000000000000, 0.000000000000000000, 1.000000000000000000 ) ) ;
#6473 = AXIS2_PLACEMENT_3D ( 'NONE', #1032, #2926, #34405 ) ;
#6474 = CARTESIAN_POINT ( 'NONE',  ( -14.52190046171712368, -14.48203382165085529, -30.00000000000001421 ) ) ;
#6475 = CARTESIAN_POINT ( 'NONE',  ( 13.11109743797562466, -26.17839091903269733, -5.000000000000000888 ) ) ;
#6476 = CARTESIAN_POINT ( 'NONE',  ( 13.81932564897710769, 23.28965451441122170, -14.48244069928644606 ) ) ;
#6477 = CARTESIAN_POINT ( 'NONE',  ( 30.98351270641326138, -22.36505350041220197, -5.858347467683552523 ) ) ;
#6478 = CARTESIAN_POINT ( 'NONE',  ( 7.773262162581151991, 10.11013643092540448, 10.49999999999999822 ) ) ;
#6479 = DIRECTION ( 'NONE',  ( -0.9945218953682745111, -0.1045284632676436454, 0.000000000000000000 ) ) ;
#6480 = ORIENTED_EDGE ( 'NONE', *, *, #17021, .F. ) ;
#6481 = CARTESIAN_POINT ( 'NONE',  ( -10.13300055019763235, 34.07230637579879584, -8.053685743483509185 ) ) ;
#6482 = CYLINDRICAL_SURFACE ( 'NONE', #22483, 1.000000000000000000 ) ;
#6483 = DIRECTION ( 'NONE',  ( 0.000000000000000000, 0.000000000000000000, 1.000000000000000000 ) ) ;
#6484 = DIRECTION ( 'NONE',  ( -1.000000000000000000, 0.000000000000000000, 0.000000000000000000 ) ) ;
#6485 = VERTEX_POINT ( 'NONE', #12957 ) ;
#6486 = CARTESIAN_POINT ( 'NONE',  ( 21.27281131302195760, 0.8015103380762446106, -25.01733364797255632 ) ) ;
#6487 = CARTESIAN_POINT ( 'NONE',  ( 14.51912675677730391, 26.26827554364630402, 7.381627713044570882 ) ) ;
#6488 = LINE ( 'NONE', #33549, #14790 ) ;
#6489 = ORIENTED_EDGE ( 'NONE', *, *, #39999, .F. ) ;
#6490 = CARTESIAN_POINT ( 'NONE',  ( -30.84974397859977557, 0.01335361837341110004, -5.474185262456348511 ) ) ;
#6491 = DIRECTION ( 'NONE',  ( 0.8090169943749497827, 0.5877852522924698064, 0.000000000000000000 ) ) ;
#6492 = VERTEX_POINT ( 'NONE', #34504 ) ;
#6493 = CARTESIAN_POINT ( 'NONE',  ( 24.37211768435814108, -5.035534140336434206, -19.93691038785375369 ) ) ;
#6494 = ORIENTED_EDGE ( 'NONE', *, *, #30912, .F. ) ;
#6495 = CARTESIAN_POINT ( 'NONE',  ( -3.887054626305479932, 40.11907545043342083, 12.14047268033113802 ) ) ;
#6496 = EDGE_CURVE ( 'NONE', #25213, #17512, #15666, .T. ) ;
#6497 = DIRECTION ( 'NONE',  ( -0.000000000000000000, -0.000000000000000000, -1.000000000000000000 ) ) ;
#6498 = PLANE ( 'NONE',  #29302 ) ;
#6499 = CARTESIAN_POINT ( 'NONE',  ( -8.489237591500351954, 31.47375793095005037, 19.27171037444226798 ) ) ;
#6500 = PLANE ( 'NONE',  #38891 ) ;
#6501 = ORIENTED_EDGE ( 'NONE', *, *, #905, .F. ) ;
#6502 = CARTESIAN_POINT ( 'NONE',  ( 4.006135375494214834, 8.432903524120153094, 10.49999999999999822 ) ) ;
#6503 = CARTESIAN_POINT ( 'NONE',  ( -19.31259245582888084, 6.905577324211579437, -30.00000000000000355 ) ) ;
#6504 = DIRECTION ( 'NONE',  ( 1.000000000000000000, 0.000000000000000000, 0.000000000000000000 ) ) ;
#6505 = VECTOR ( 'NONE', #6793, 999.9999999999998863 ) ;
#6506 = DIRECTION ( 'NONE',  ( 1.000000000000000000, 0.000000000000000000, 0.000000000000000000 ) ) ;
#6507 = CARTESIAN_POINT ( 'NONE',  ( 13.79510298735225859, 15.29130589365389703, -28.21449070774182388 ) ) ;
#6508 = CARTESIAN_POINT ( 'NONE',  ( 4.803761294507334689, 21.37012296307172932, -24.35659395119734683 ) ) ;
#6509 = EDGE_CURVE ( 'NONE', #36470, #18790, #36440, .T. ) ;
#6510 = CARTESIAN_POINT ( 'NONE',  ( 10.66098508067554995, -17.52284468788354843, -29.32387687725450220 ) ) ;
#6511 = CARTESIAN_POINT ( 'NONE',  ( 0.5000000000000000000, 37.50000000000000711, 10.50000000000000000 ) ) ;
#6512 = CARTESIAN_POINT ( 'NONE',  ( -4.100643064501314328, 15.70406341247269211, 12.00000000000000000 ) ) ;
#6513 = ORIENTED_EDGE ( 'NONE', *, *, #10295, .T. ) ;
#6514 = CARTESIAN_POINT ( 'NONE',  ( -14.85706654925435366, 25.55795220932581202, -10.18130676548022606 ) ) ;
#6515 = CIRCLE ( 'NONE', #15003, 21.00000000000002842 ) ;
#6516 = CARTESIAN_POINT ( 'NONE',  ( -32.69618749603004915, -17.08296528845537665, 17.92354375535288469 ) ) ;
#6517 = CARTESIAN_POINT ( 'NONE',  ( 14.69203212197494324, -25.92680292136585862, -9.241851185403270108 ) ) ;
#6518 = ADVANCED_FACE ( 'NONE', ( #28598 ), #24769, .T. ) ;
#6519 = AXIS2_PLACEMENT_3D ( 'NONE', #1525, #26307, #6998 ) ;
#6520 = DIRECTION ( 'NONE',  ( 1.000000000000000000, 0.000000000000000000, 0.000000000000000000 ) ) ;
#6521 = EDGE_CURVE ( 'NONE', #257, #11836, #31451, .T. ) ;
#6522 = ORIENTED_EDGE ( 'NONE', *, *, #28780, .T. ) ;
#6523 = ORIENTED_EDGE ( 'NONE', *, *, #39393, .T. ) ;
#6524 = CARTESIAN_POINT ( 'NONE',  ( -10.01402912130534162, 17.90039694996872655, -29.99999999999999645 ) ) ;
#6525 = CARTESIAN_POINT ( 'NONE',  ( -19.16096150374591289, -26.90160068996506126, -7.719816727323686401 ) ) ;
#6526 = FACE_BOUND ( 'NONE', #20907, .T. ) ;
#6527 = ORIENTED_EDGE ( 'NONE', *, *, #23233, .F. ) ;
#6528 = CARTESIAN_POINT ( 'NONE',  ( -26.11057960447877946, -8.126273745962151906, -17.72871576020790130 ) ) ;
#6529 = CARTESIAN_POINT ( 'NONE',  ( -15.16468140352661997, -26.46607220469503474, -7.358403229616178542 ) ) ;
#6530 = DIRECTION ( 'NONE',  ( -0.9135454576425988682, 0.4067366430758048157, 0.000000000000000000 ) ) ;
#6531 = VERTEX_POINT ( 'NONE', #3023 ) ;
#6532 = CARTESIAN_POINT ( 'NONE',  ( 20.47266963615838264, 1.058032431983775723, -30.00000000000000355 ) ) ;
#6533 = CYLINDRICAL_SURFACE ( 'NONE', #37520, 1.000000000000000000 ) ;
#6534 = CARTESIAN_POINT ( 'NONE',  ( 3.813962023474615215, 32.29559562678520024, 10.50000000000000000 ) ) ;
#6535 = AXIS2_PLACEMENT_3D ( 'NONE', #39291, #11468, #32409 ) ;
#6536 = ORIENTED_EDGE ( 'NONE', *, *, #18115, .F. ) ;
#6537 = CARTESIAN_POINT ( 'NONE',  ( -29.61695854582710297, 0.02674555327310050579, -10.17862021117223037 ) ) ;
#6538 = ORIENTED_EDGE ( 'NONE', *, *, #16006, .F. ) ;
#6539 = CARTESIAN_POINT ( 'NONE',  ( 21.05791172284567025, -0.3372447964882535620, -26.12359182236599864 ) ) ;
#6540 = CARTESIAN_POINT ( 'NONE',  ( 13.28052513718836458, -15.63203832709782581, -29.99999999999999645 ) ) ;
#6541 = CARTESIAN_POINT ( 'NONE',  ( 34.71804043165853670, -14.31680059899166757, 16.87380292611441845 ) ) ;
#6542 = EDGE_CURVE ( 'NONE', #37934, #25787, #2078, .T. ) ;
#6543 = VERTEX_POINT ( 'NONE', #574 ) ;
#6544 = CARTESIAN_POINT ( 'NONE',  ( -22.31696031899349464, 4.303969307314124748, -19.86790886566943470 ) ) ;
#6545 = EDGE_CURVE ( 'NONE', #19499, #18941, #40191, .T. ) ;
#6546 = DIRECTION ( 'NONE',  ( -0.000000000000000000, -0.000000000000000000, -1.000000000000000000 ) ) ;
#6547 = CARTESIAN_POINT ( 'NONE',  ( 2.109373541296156063, 27.06550157850343652, 21.00000000000000355 ) ) ;
#6548 = AXIS2_PLACEMENT_3D ( 'NONE', #32357, #16919, #8162 ) ;
#6549 = DIRECTION ( 'NONE',  ( -0.1045284632676437842, 0.9945218953682744001, -0.000000000000000000 ) ) ;
#6550 = AXIS2_PLACEMENT_3D ( 'NONE', #29298, #13855, #7953 ) ;
#6551 = CARTESIAN_POINT ( 'NONE',  ( 10.78893975237932956, 23.27376113029817617, 6.000000000000000000 ) ) ;
#6552 = FACE_OUTER_BOUND ( 'NONE', #5160, .T. ) ;
#6553 = CARTESIAN_POINT ( 'NONE',  ( 13.94482798346721353, 26.50521816028912525, 9.000000000000001776 ) ) ;
#6554 = CARTESIAN_POINT ( 'NONE',  ( -24.70587413898208951, 7.101647862693369007, -7.408522823150167191 ) ) ;
#6555 = CYLINDRICAL_SURFACE ( 'NONE', #9904, 1.000000000000000000 ) ;
#6556 = CARTESIAN_POINT ( 'NONE',  ( 23.35460752408678786, -25.71782482220768173, -8.953985723103441430 ) ) ;
#6557 = DIRECTION ( 'NONE',  ( 0.000000000000000000, 0.000000000000000000, 1.000000000000000000 ) ) ;
#6558 = EDGE_CURVE ( 'NONE', #17265, #4972, #17662, .T. ) ;
#6559 = CARTESIAN_POINT ( 'NONE',  ( 14.43041895983224343, 25.25700966609383258, -11.57758239486862983 ) ) ;
#6560 = ORIENTED_EDGE ( 'NONE', *, *, #9500, .F. ) ;
#6561 = CARTESIAN_POINT ( 'NONE',  ( -12.99709060340919820, 16.32919408374584691, -26.39889406728086030 ) ) ;
#6562 = CARTESIAN_POINT ( 'NONE',  ( -29.18902924043318237, -8.936254945823375095, 20.25080042701515737 ) ) ;
#6563 = CARTESIAN_POINT ( 'NONE',  ( 10.44367147699342091, 33.07775263288196754, 10.49999999999999822 ) ) ;
#6564 = CARTESIAN_POINT ( 'NONE',  ( 15.38907305648967139, 26.61214354874361021, -6.417068104208305535 ) ) ;
#6565 = ORIENTED_EDGE ( 'NONE', *, *, #17365, .T. ) ;
#6566 = CARTESIAN_POINT ( 'NONE',  ( 0.000000000000000000, 22.50000000000000355, 12.00000000000000000 ) ) ;
#6567 = EDGE_LOOP ( 'NONE', ( #15473, #19399, #10602, #29322, #37817, #21965, #14497 ) ) ;
#6569 = DIRECTION ( 'NONE',  ( 1.000000000000000000, 0.000000000000000000, 0.000000000000000000 ) ) ;
#6568 = CARTESIAN_POINT ( 'NONE',  ( -14.85275514143794062, 26.05732730074270620, -9.694811670314079421 ) ) ;
#6570 = CARTESIAN_POINT ( 'NONE',  ( -15.63755959170095089, -26.78052150289263622, -5.473470747264984837 ) ) ;
#6571 = CARTESIAN_POINT ( 'NONE',  ( 10.04974741695038354, 22.44923726269170672, 10.50000000000000533 ) ) ;
#6572 = AXIS2_PLACEMENT_3D ( 'NONE', #20726, #36551, #17481 ) ;
#6573 = ORIENTED_EDGE ( 'NONE', *, *, #17735, .T. ) ;
#6574 = CARTESIAN_POINT ( 'NONE',  ( -28.14503232587697923, -13.65727403788577377, -14.73885408196157343 ) ) ;
#6575 = CARTESIAN_POINT ( 'NONE',  ( -9.042639598297487424, -18.73478658976852529, -26.88259372887121756 ) ) ;
#6576 = FACE_OUTER_BOUND ( 'NONE', #26094, .T. ) ;
#6577 = CARTESIAN_POINT ( 'NONE',  ( 15.99681398212475081, 22.41394734825504997, -10.24358248442191943 ) ) ;
#6578 = ORIENTED_EDGE ( 'NONE', *, *, #38722, .F. ) ;
#6579 = CARTESIAN_POINT ( 'NONE',  ( 22.61667714053060863, 4.539058822887956701, -18.82962114486994665 ) ) ;
#6580 = VECTOR ( 'NONE', #25387, 1000.000000000000000 ) ;
#6581 = FACE_OUTER_BOUND ( 'NONE', #14752, .T. ) ;
#6582 = DIRECTION ( 'NONE',  ( 1.000000000000000000, 0.000000000000000000, 0.000000000000000000 ) ) ;
#6583 = CARTESIAN_POINT ( 'NONE',  ( -12.01838097023000529, 23.73363068877903359, 13.00000000000000178 ) ) ;
#6584 = B_SPLINE_CURVE_WITH_KNOTS ( 'NONE', 3,
 ( #36806, #24809, #21367, #27457 ),
 .UNSPECIFIED., .F., .F.,
 ( 4, 4 ),
 ( 0.0005941180652377696467, 0.0009459474155737164318 ),
 .UNSPECIFIED. ) ;
#6585 = ORIENTED_EDGE ( 'NONE', *, *, #34125, .T. ) ;
#6586 = CARTESIAN_POINT ( 'NONE',  ( -28.63560929655779219, -0.2296132274206826862, -12.51332363996011310 ) ) ;
#6587 = CARTESIAN_POINT ( 'NONE',  ( 28.61027353976883347, -0.1971735349054578590, -12.51648547223809160 ) ) ;
#6588 = CARTESIAN_POINT ( 'NONE',  ( 29.65273330788082262, -7.615246293903670249, 19.99202127657073902 ) ) ;
#6589 = ORIENTED_EDGE ( 'NONE', *, *, #1844, .T. ) ;
#6590 = VECTOR ( 'NONE', #20939, 1000.000000000000000 ) ;
#6591 = EDGE_CURVE ( 'NONE', #8118, #10191, #28016, .T. ) ;
#6592 = CARTESIAN_POINT ( 'NONE',  ( 7.289639608743136989, -27.06962010326278545, -13.42901749168595593 ) ) ;
#6593 = CYLINDRICAL_SURFACE ( 'NONE', #3102, 1.000000000000000000 ) ;
#6594 = ORIENTED_EDGE ( 'NONE', *, *, #28271, .T. ) ;
#6595 = DIRECTION ( 'NONE',  ( 0.000000000000000000, 0.000000000000000000, 1.000000000000000000 ) ) ;
#6596 = CARTESIAN_POINT ( 'NONE',  ( 12.03640989728592459, 29.14264673470096767, 12.00000000000000000 ) ) ;
#6597 = DIRECTION ( 'NONE',  ( -1.000000000000000000, 0.000000000000000000, 0.000000000000000000 ) ) ;
#6598 = CARTESIAN_POINT ( 'NONE',  ( 0.8480541672973396228, 20.90088328258439887, -26.96762484265282112 ) ) ;
#6599 = DIRECTION ( 'NONE',  ( 0.000000000000000000, 0.000000000000000000, 1.000000000000000000 ) ) ;
#6600 = CYLINDRICAL_SURFACE ( 'NONE', #1270, 1.000000000000000888 ) ;
#6601 = DIRECTION ( 'NONE',  ( 0.4067366430758010964, 0.9135454576426005335, 0.000000000000000000 ) ) ;
#6602 = CYLINDRICAL_SURFACE ( 'NONE', #20974, 0.4999999999999995559 ) ;
#6603 = EDGE_CURVE ( 'NONE', #342, #22756, #9324, .T. ) ;
#6604 = DIRECTION ( 'NONE',  ( 1.000000000000000000, 0.000000000000000000, 0.000000000000000000 ) ) ;
#6605 = CARTESIAN_POINT ( 'NONE',  ( 10.28246022096949908, 18.16882197377053032, -26.75189561797980531 ) ) ;
#6606 = CARTESIAN_POINT ( 'NONE',  ( -14.51390269127088928, 5.102206419419879957, 7.000000000000000000 ) ) ;
#6607 = EDGE_LOOP ( 'NONE', ( #27878, #30510 ) ) ;
#6609 = CARTESIAN_POINT ( 'NONE',  ( -5.400683141673551013, 15.91724817395922997, 9.000000000000001776 ) ) ;
#6608 = CARTESIAN_POINT ( 'NONE',  ( -18.68025062537304493, 17.59719118396984072, -6.925800422574094561 ) ) ;
#6610 = CYLINDRICAL_SURFACE ( 'NONE', #29603, 1.000000000000000888 ) ;
#6611 = EDGE_CURVE ( 'NONE', #12248, #12299, #33859, .T. ) ;
#6612 = AXIS2_PLACEMENT_3D ( 'NONE', #32238, #8659, #20661 ) ;
#6613 = CARTESIAN_POINT ( 'NONE',  ( 15.34965201500932785, -26.58387937520311084, -6.887971616833333144 ) ) ;
#6614 = CARTESIAN_POINT ( 'NONE',  ( -20.58361896323833307, -25.87753243228978661, -9.918039572038674478 ) ) ;
#6615 = CARTESIAN_POINT ( 'NONE',  ( 13.21227310165477320, 22.23035794993680270, -16.44475469494696540 ) ) ;
#6616 = CARTESIAN_POINT ( 'NONE',  ( 11.67513080692914151, 18.92206925029848108, -22.73326350911885285 ) ) ;
#6617 = ORIENTED_EDGE ( 'NONE', *, *, #29099, .F. ) ;
#6618 = DIRECTION ( 'NONE',  ( -1.000000000000000000, 0.000000000000000000, 0.000000000000000000 ) ) ;
#6619 = CARTESIAN_POINT ( 'NONE',  ( -14.85743854809297737, -25.96320633999491179, -9.239818057270476004 ) ) ;
#6620 = CARTESIAN_POINT ( 'NONE',  ( -32.18944385490189575, 1.219497045964027748, 12.73282698324853079 ) ) ;
#6621 = ADVANCED_FACE ( 'NONE', ( #28396 ), #15614, .F. ) ;
#6622 = CARTESIAN_POINT ( 'NONE',  ( -31.09129472269700756, -21.46021889108168779, -7.549027889585831375 ) ) ;
#6623 = CARTESIAN_POINT ( 'NONE',  ( -1.777045556556341888, -20.53114539011956197, -28.29789199099749908 ) ) ;
#6624 = CARTESIAN_POINT ( 'NONE',  ( 12.21857019178368020, 19.03452810332261080, -21.67269469152422445 ) ) ;
#6625 = ORIENTED_EDGE ( 'NONE', *, *, #22530, .T. ) ;
#6626 = CARTESIAN_POINT ( 'NONE',  ( 22.75140569375547983, 10.14465275586799997, -6.451765741814347699 ) ) ;
#6627 = CARTESIAN_POINT ( 'NONE',  ( -6.176557290856002247, -13.77694981160526844, 23.00000000000000355 ) ) ;
#6628 = CARTESIAN_POINT ( 'NONE',  ( 3.246717519899792403, 37.21789761807038133, 17.42190598798394774 ) ) ;
#6629 = VERTEX_POINT ( 'NONE', #37552 ) ;
#6630 = CARTESIAN_POINT ( 'NONE',  ( -32.38786556318342491, -4.220081569580368175, -9.945407286558161530 ) ) ;
#6631 = CARTESIAN_POINT ( 'NONE',  ( -21.46287209667396922, 12.39159498259534686, 16.30093088680190405 ) ) ;
#6632 = VECTOR ( 'NONE', #40044, 1000.000000000000000 ) ;
#6633 = ORIENTED_EDGE ( 'NONE', *, *, #18111, .T. ) ;
#6634 = CARTESIAN_POINT ( 'NONE',  ( 2.229970528062776403, 7.666518487011187766, 7.381627713044564665 ) ) ;
#6635 = CARTESIAN_POINT ( 'NONE',  ( 2.525645716490518389, 8.212903943950921715, 7.000000000000000000 ) ) ;
#6636 = EDGE_CURVE ( 'NONE', #22937, #19894, #9723, .T. ) ;
#6637 = CARTESIAN_POINT ( 'NONE',  ( -30.25911448991262276, 0.6236314785230304691, -5.474043737439959756 ) ) ;
#6638 = EDGE_CURVE ( 'NONE', #18932, #2112, #16333, .T. ) ;
#6639 = CARTESIAN_POINT ( 'NONE',  ( 19.31437624530733643, -7.140418407204370155, -28.47186176483214837 ) ) ;
#6640 = EDGE_CURVE ( 'NONE', #26114, #19442, #12446, .T. ) ;
#6641 = CARTESIAN_POINT ( 'NONE',  ( 33.82738586796132552, -21.73727074213809729, 13.32518128616604791 ) ) ;
#6642 = VERTEX_POINT ( 'NONE', #22896 ) ;
#6643 = VECTOR ( 'NONE', #18502, 1000.000000000000000 ) ;
#6644 = EDGE_LOOP ( 'NONE', ( #10715, #17713, #3208, #32996, #32591 ) ) ;
#6645 = CARTESIAN_POINT ( 'NONE',  ( -14.98890121934603314, -28.67928442654204346, 23.00000000000000000 ) ) ;
#6646 = CARTESIAN_POINT ( 'NONE',  ( 23.05386822411319159, -7.747535282638377652, 23.00000000000000000 ) ) ;
#6647 = AXIS2_PLACEMENT_3D ( 'NONE', #1299, #37863, #12880 ) ;
#6648 = LINE ( 'NONE', #31447, #22034 ) ;
#6649 = ORIENTED_EDGE ( 'NONE', *, *, #11291, .T. ) ;
#6650 = CARTESIAN_POINT ( 'NONE',  ( -2.423886253481512210, 30.01527867101077973, -15.69239631665445422 ) ) ;
#6651 = DIRECTION ( 'NONE',  ( -0.000000000000000000, -0.000000000000000000, 1.000000000000000000 ) ) ;
#6652 = DIRECTION ( 'NONE',  ( 0.4067366430758009299, 0.9135454576426005335, 0.000000000000000000 ) ) ;
#6653 = CARTESIAN_POINT ( 'NONE',  ( 6.440829913680675034, 10.60893893836775348, 6.000000000000000000 ) ) ;
#6654 = FACE_OUTER_BOUND ( 'NONE', #3146, .T. ) ;
#6655 = ADVANCED_FACE ( 'NONE', ( #10313 ), #7457, .T. ) ;
#6656 = CARTESIAN_POINT ( 'NONE',  ( 2.579909280894411516, 7.957613945008743528, 10.94611345180490858 ) ) ;
#6657 = CARTESIAN_POINT ( 'NONE',  ( 12.24878116420049068, 29.33560266281129358, -11.31652717080035231 ) ) ;
#6658 = EDGE_LOOP ( 'NONE', ( #33741, #1092, #6997 ) ) ;
#6659 = CARTESIAN_POINT ( 'NONE',  ( -21.25484840722362279, 12.72181903587277318, -5.483107197446321024 ) ) ;
#6660 = CARTESIAN_POINT ( 'NONE',  ( 8.437494165185171369, 40.76200631401452767, 11.00000000000000000 ) ) ;
#6661 = ADVANCED_FACE ( 'NONE', ( #20267 ), #34899, .T. ) ;
#6662 = CARTESIAN_POINT ( 'NONE',  ( 14.92053913355477590, -25.84391472125183498, -9.706504376371448473 ) ) ;
#6663 = CARTESIAN_POINT ( 'NONE',  ( 6.354454053420411697, 35.54304081427980577, 7.000000000000000000 ) ) ;
#6664 = CARTESIAN_POINT ( 'NONE',  ( 11.64760469399007725, 18.94855002001494171, -22.72844738028206635 ) ) ;
#6665 = CARTESIAN_POINT ( 'NONE',  ( 31.47283671532267846, -25.12609584734865464, -5.000000000000006217 ) ) ;
#6666 = DIRECTION ( 'NONE',  ( -0.5000000000000038858, -0.8660254037844363761, 0.000000000000000000 ) ) ;
#6667 = AXIS2_PLACEMENT_3D ( 'NONE', #39498, #2533, #17786 ) ;
#6668 = CARTESIAN_POINT ( 'NONE',  ( -23.35727036480124852, -23.34227582478836993, -12.07518644368831850 ) ) ;
#6669 = CARTESIAN_POINT ( 'NONE',  ( 11.11180036078298272, -23.01599423131538558, -15.57141518415062720 ) ) ;
#6670 = CARTESIAN_POINT ( 'NONE',  ( 12.26164114550799944, 19.76946988966989949, -20.56397771860881107 ) ) ;
#6671 = CARTESIAN_POINT ( 'NONE',  ( 29.43405427299785515, -21.28324550421933381, -9.736337039119780101 ) ) ;
#6672 = VECTOR ( 'NONE', #16058, 1000.000000000000114 ) ;
#6673 = FACE_OUTER_BOUND ( 'NONE', #12882, .T. ) ;
#6674 = CARTESIAN_POINT ( 'NONE',  ( -33.75875814100324845, 2.759858869446484064, 11.00000000000000000 ) ) ;
#6675 = ORIENTED_EDGE ( 'NONE', *, *, #6509, .T. ) ;
#6676 = CARTESIAN_POINT ( 'NONE',  ( -5.620579596833452207, 21.10756638118547457, -24.41133304458605124 ) ) ;
#6677 = CARTESIAN_POINT ( 'NONE',  ( -7.910872327081295730, 10.00199400870863187, 10.49999999999999822 ) ) ;
#6678 = VECTOR ( 'NONE', #39300, 1000.000000000000000 ) ;
#6679 = CYLINDRICAL_SURFACE ( 'NONE', #35807, 15.00000000000000000 ) ;
#6680 = VERTEX_POINT ( 'NONE', #4823 ) ;
#6681 = CARTESIAN_POINT ( 'NONE',  ( 30.83224212302263822, -0.07211122296361122119, -6.416159285224059872 ) ) ;
#6682 = CARTESIAN_POINT ( 'NONE',  ( -14.44975846301057310, 26.39485539169832506, 10.49999999999999467 ) ) ;
#6683 = CYLINDRICAL_SURFACE ( 'NONE', #34940, 6.000000000000003553 ) ;
#6684 = VERTEX_POINT ( 'NONE', #17227 ) ;
#6685 = CARTESIAN_POINT ( 'NONE',  ( -25.83958759730864685, 0.3586317713515524974, -16.44731683257352373 ) ) ;
#6686 = CARTESIAN_POINT ( 'NONE',  ( -20.57926082973601822, -27.21289976943432265, -4.999999999999998224 ) ) ;
#6687 = AXIS2_PLACEMENT_3D ( 'NONE', #30011, #35908, #11528 ) ;
#6688 = ORIENTED_EDGE ( 'NONE', *, *, #16721, .F. ) ;
#6689 = CARTESIAN_POINT ( 'NONE',  ( 20.94073701540919075, -3.630281487320123457, -25.85615716460149827 ) ) ;
#6690 = CIRCLE ( 'NONE', #29413, 1.000000000000000444 ) ;
#6691 = VERTEX_POINT ( 'NONE', #16621 ) ;
#6692 = CARTESIAN_POINT ( 'NONE',  ( 9.308285395644954718, 37.95628792398655094, 12.14047268033102256 ) ) ;
#6693 = DIRECTION ( 'NONE',  ( -0.7431448254773862505, 0.6691306063588672304, -0.000000000000000000 ) ) ;
#6694 = CARTESIAN_POINT ( 'NONE',  ( -23.05386822411323422, -7.747535282638357224, 23.00000000000000000 ) ) ;
#6695 = CARTESIAN_POINT ( 'NONE',  ( -1.329271672591240128, 34.78122644969442945, 19.27171037444156454 ) ) ;
#6696 = CIRCLE ( 'NONE', #35243, 1.000000000000000000 ) ;
#6697 = DIRECTION ( 'NONE',  ( 1.000000000000000000, 0.000000000000000000, 0.000000000000000000 ) ) ;
#6698 = EDGE_LOOP ( 'NONE', ( #641, #11607 ) ) ;
#6699 = DIRECTION ( 'NONE',  ( -0.000000000000000000, -0.000000000000000000, -1.000000000000000000 ) ) ;
#6700 = CARTESIAN_POINT ( 'NONE',  ( -19.98575265377075993, -4.745023977884823552, -30.00000000000000355 ) ) ;
#6701 = MECHANICAL_DESIGN_GEOMETRIC_PRESENTATION_REPRESENTATION (  '', ( #5414 ), #8666 ) ;
#6702 = DIRECTION ( 'NONE',  ( 0.000000000000000000, 0.000000000000000000, 1.000000000000000000 ) ) ;
#6703 = CARTESIAN_POINT ( 'NONE',  ( -3.000488737322915878, 30.46850471150003159, 9.000000000000001776 ) ) ;
#6704 = CARTESIAN_POINT ( 'NONE',  ( 17.65119513763062287, 19.95841547798437077, -6.914159246569045791 ) ) ;
#6705 = CARTESIAN_POINT ( 'NONE',  ( 9.937273488330333748, 34.60605125810194949, -7.177303487740063659 ) ) ;
#6706 = VECTOR ( 'NONE', #20516, 1000.000000000000000 ) ;
#6707 = CARTESIAN_POINT ( 'NONE',  ( 13.44315901770257682, -21.33295835193786516, -18.26921127929339050 ) ) ;
#6708 = CARTESIAN_POINT ( 'NONE',  ( 9.997483185316555776, 21.95197631500756685, 10.50000000000000000 ) ) ;
#6709 = CARTESIAN_POINT ( 'NONE',  ( -14.52509594610762456, 21.97885917798744870, 10.49999999999999467 ) ) ;
#6710 = ORIENTED_EDGE ( 'NONE', *, *, #39152, .T. ) ;
#6711 = CARTESIAN_POINT ( 'NONE',  ( -14.85137426362708624, 25.57504807805499070, -10.18098964417948693 ) ) ;
#6712 = AXIS2_PLACEMENT_3D ( 'NONE', #36212, #14463, #2084 ) ;
#6713 = CARTESIAN_POINT ( 'NONE',  ( -23.78889779961598450, -25.69434382178283371, 17.42190598798429590 ) ) ;
#6714 = CARTESIAN_POINT ( 'NONE',  ( 11.69482082898245956, -21.50151594381998166, -18.47287864288130876 ) ) ;
#6715 = DIRECTION ( 'NONE',  ( 0.000000000000000000, 0.000000000000000000, 1.000000000000000000 ) ) ;
#6716 = ORIENTED_EDGE ( 'NONE', *, *, #15796, .T. ) ;
#6717 = ORIENTED_EDGE ( 'NONE', *, *, #30221, .T. ) ;
#6718 = CARTESIAN_POINT ( 'NONE',  ( -13.11788538660038306, 24.75960143229000110, -14.33734891237946130 ) ) ;
#6719 = CARTESIAN_POINT ( 'NONE',  ( -12.40276990898003895, -16.90054566293658667, -26.59307398587640137 ) ) ;
#6720 = FACE_BOUND ( 'NONE', #22288, .T. ) ;
#6721 = AXIS2_PLACEMENT_3D ( 'NONE', #14574, #11925, #39353 ) ;
#6722 = CARTESIAN_POINT ( 'NONE',  ( -25.24452815043373022, -7.038082672387002248, -18.79164011408699153 ) ) ;
#6723 = CARTESIAN_POINT ( 'NONE',  ( -15.01606105974973104, -26.24525916788589086, -8.298880598885562065 ) ) ;
#6724 = DIRECTION ( 'NONE',  ( 0.6459741880212575005, 0.2876062384759433543, -0.7071067811865445751 ) ) ;
#6725 = EDGE_LOOP ( 'NONE', ( #31565, #9056, #32529, #5697, #3716, #29240, #31276 ) ) ;
#6726 = CARTESIAN_POINT ( 'NONE',  ( 30.16006263997094550, 0.2005578054670466015, -8.299689423995275206 ) ) ;
#6727 = CARTESIAN_POINT ( 'NONE',  ( 11.30648189679965654, 18.04080162749803407, -25.01410075632841412 ) ) ;
#6728 = FACE_OUTER_BOUND ( 'NONE', #9714, .T. ) ;
#6729 = B_SPLINE_CURVE_WITH_KNOTS ( 'NONE', 3,
 ( #15470, #16068, #15670, #15872, #9377, #31113 ),
 .UNSPECIFIED., .F., .F.,
 ( 4, 2, 4 ),
 ( 0.000000000000000000, 0.5000000000000000000, 1.000000000000000000 ),
 .UNSPECIFIED. ) ;
#6730 = B_SPLINE_CURVE_WITH_KNOTS ( 'NONE', 3,
 ( #6307, #27852, #21552, #36999 ),
 .UNSPECIFIED., .F., .F.,
 ( 4, 4 ),
 ( 0.000000000000000000, 1.000000000000000000 ),
 .UNSPECIFIED. ) ;
#6731 = ORIENTED_EDGE ( 'NONE', *, *, #20895, .F. ) ;
#6732 = CARTESIAN_POINT ( 'NONE',  ( -21.27998365777518330, 0.7502355399091473753, -25.01178682489351601 ) ) ;
#6733 = VERTEX_POINT ( 'NONE', #4215 ) ;
#6734 = CARTESIAN_POINT ( 'NONE',  ( 31.94105064681168571, -2.205082878242727862, -8.660796739423290092 ) ) ;
#6735 = AXIS2_PLACEMENT_3D ( 'NONE', #26555, #17220, #38743 ) ;
#6736 = CARTESIAN_POINT ( 'NONE',  ( -3.357890496178010054, -20.26885263950605420, -30.00000000000000000 ) ) ;
#6737 = CARTESIAN_POINT ( 'NONE',  ( 31.01938180032263048, -21.79666295253546338, 16.87380292611479859 ) ) ;
#6738 = EDGE_CURVE ( 'NONE', #31599, #20519, #26717, .T. ) ;
#6739 = ORIENTED_EDGE ( 'NONE', *, *, #14132, .F. ) ;
#6740 = DIRECTION ( 'NONE',  ( 1.000000000000000000, 0.000000000000000000, 0.000000000000000000 ) ) ;
#6741 = CARTESIAN_POINT ( 'NONE',  ( -4.441848239913461782, 24.85865334748894284, 20.99999999999999645 ) ) ;
#6742 = VECTOR ( 'NONE', #20071, 1000.000000000000000 ) ;
#6743 = CARTESIAN_POINT ( 'NONE',  ( 8.559505275947156377, 25.28115294937476065, 6.000000000000000000 ) ) ;
#6744 = ADVANCED_FACE ( 'NONE', ( #10929 ), #5895, .T. ) ;
#6745 = FACE_OUTER_BOUND ( 'NONE', #12798, .T. ) ;
#6746 = EDGE_CURVE ( 'NONE', #32554, #32493, #7054, .T. ) ;
#6747 = B_SPLINE_SURFACE_WITH_KNOTS ( 'NONE', 1, 3, ( 
 ( #36340, #5456, #27191, #23138, #11153, #35740, #38780, #4652, #10958, #32698 ),
 ( #23345, #20099, #8504, #29835, #33102, #8308, #11557, #29635, #20901, #14194 ) ),
 .UNSPECIFIED., .F., .F., .F.,
 ( 2, 2 ),
 ( 4, 2, 2, 2, 4 ),
 ( 0.000000000000000000, 1.000000000000000000 ),
 ( -1.096214744126243978, -0.7035156624275198389, -0.3108165807287956994, 0.08188250096992841232, 0.4745815826686525241 ),
 .UNSPECIFIED. ) ;
#6748 = VECTOR ( 'NONE', #18722, 1000.000000000000000 ) ;
#6749 = FACE_BOUND ( 'NONE', #21386, .T. ) ;
#6750 = CARTESIAN_POINT ( 'NONE',  ( 23.18947492591164661, 13.38844959084105568, 11.55979286843934872 ) ) ;
#6751 = CARTESIAN_POINT ( 'NONE',  ( -18.95922262551748361, 7.795319610833783663, -30.00000000000000000 ) ) ;
#6752 = CARTESIAN_POINT ( 'NONE',  ( 18.71898351499973145, -19.47505160051558448, -17.80877851765054132 ) ) ;
#6753 = CARTESIAN_POINT ( 'NONE',  ( -20.71630303010418572, -29.20803740758281464, -4.999999999999997335 ) ) ;
#6754 = CARTESIAN_POINT ( 'NONE',  ( 15.23567902583548417, 26.71743813441107207, -7.352606933093872144 ) ) ;
#6755 = VERTEX_POINT ( 'NONE', #26356 ) ;
#6756 = AXIS2_PLACEMENT_3D ( 'NONE', #30904, #24402, #30706 ) ;
#6757 = CARTESIAN_POINT ( 'NONE',  ( -15.60993106802417252, 25.69096736691974669, -6.890080393197788311 ) ) ;
#6758 = CARTESIAN_POINT ( 'NONE',  ( -23.32346807013534828, -20.39486175172809013, 20.25080042701566541 ) ) ;
#6759 = ADVANCED_FACE ( 'NONE', ( #28999 ), #26562, .F. ) ;
#6760 = EDGE_CURVE ( 'NONE', #39486, #14121, #11103, .T. ) ;
#6761 = CARTESIAN_POINT ( 'NONE',  ( -3.357189294653179612, 32.49896394832315849, 10.50000000000000000 ) ) ;
#6762 = CARTESIAN_POINT ( 'NONE',  ( 15.31233209253673699, 26.45408978173025005, -7.358089053015683945 ) ) ;
#6763 = ORIENTED_EDGE ( 'NONE', *, *, #19306, .T. ) ;
#6764 = DIRECTION ( 'NONE',  ( 1.000000000000000000, 0.000000000000000000, 0.000000000000000000 ) ) ;
#6765 = ORIENTED_EDGE ( 'NONE', *, *, #11156, .F. ) ;
#6767 = CARTESIAN_POINT ( 'NONE',  ( -14.60301432615393047, 21.46791548645777326, 11.00000000000000000 ) ) ;
#6766 = CARTESIAN_POINT ( 'NONE',  ( -14.91657227004425934, 26.29114371075054990, -9.222413299652547636 ) ) ;
#6768 = CARTESIAN_POINT ( 'NONE',  ( -14.82334245325438538, -25.50166360968241719, -10.64068735651913578 ) ) ;
#6769 = CARTESIAN_POINT ( 'NONE',  ( 0.000000000000000000, 22.50000000000000355, 7.000000000000000000 ) ) ;
#6770 = ORIENTED_EDGE ( 'NONE', *, *, #17421, .T. ) ;
#6771 = CARTESIAN_POINT ( 'NONE',  ( -34.86194987718285176, -15.64482351731836474, -5.858316081785087448 ) ) ;
#6772 = CARTESIAN_POINT ( 'NONE',  ( -14.14861525076418580, -26.29469343071681209, -6.890863552359059341 ) ) ;
#6773 = DIRECTION ( 'NONE',  ( -0.000000000000000000, -0.000000000000000000, -1.000000000000000000 ) ) ;
#6774 = CARTESIAN_POINT ( 'NONE',  ( 12.68075659042399117, 16.15066152451087689, -28.76951523894423701 ) ) ;
#6775 = ORIENTED_EDGE ( 'NONE', *, *, #24897, .F. ) ;
#6776 = CARTESIAN_POINT ( 'NONE',  ( 25.68561304534730283, 5.556133728777049363, -8.363004190235322710 ) ) ;
#6777 = DIRECTION ( 'NONE',  ( 0.000000000000000000, 0.000000000000000000, 1.000000000000000000 ) ) ;
#6778 = CYLINDRICAL_SURFACE ( 'NONE', #34814, 18.00000000000000000 ) ;
#6779 = CARTESIAN_POINT ( 'NONE',  ( -13.16028273094462975, 27.30176617939698147, 7.499999999999994671 ) ) ;
#6780 = ORIENTED_EDGE ( 'NONE', *, *, #3316, .T. ) ;
#6781 = CARTESIAN_POINT ( 'NONE',  ( -25.58894034025924213, -0.3267592592326616363, -17.34686670204293435 ) ) ;
#6782 = AXIS2_PLACEMENT_3D ( 'NONE', #34962, #631, #16474 ) ;
#6783 = CARTESIAN_POINT ( 'NONE',  ( 31.11181571040396321, -0.2945068792762812193, -5.942526464314708434 ) ) ;
#6784 = CARTESIAN_POINT ( 'NONE',  ( 29.77970073067787027, -14.50783476829474594, 19.99202127657104811 ) ) ;
#6785 = ORIENTED_EDGE ( 'NONE', *, *, #8064, .F. ) ;
#6786 = AXIS2_PLACEMENT_3D ( 'NONE', #21074, #36910, #14577 ) ;
#6787 = EDGE_CURVE ( 'NONE', #36443, #31380, #10327, .T. ) ;
#6788 = CARTESIAN_POINT ( 'NONE',  ( -37.49625565938783467, -14.69322820095469240, -5.000000000000006217 ) ) ;
#6789 = DIRECTION ( 'NONE',  ( 0.3090169943749448977, -0.9510565162951543083, 0.000000000000000000 ) ) ;
#6790 = CIRCLE ( 'NONE', #7464, 1.000000000000000000 ) ;
#6791 = ORIENTED_EDGE ( 'NONE', *, *, #4610, .T. ) ;
#6792 = LINE ( 'NONE', #518, #10640 ) ;
#6793 = DIRECTION ( 'NONE',  ( -0.7431448254773863615, 0.6691306063588671194, 0.000000000000000000 ) ) ;
#6794 = CARTESIAN_POINT ( 'NONE',  ( 16.17302619178590462, 24.05975780865501790, -4.999999999999999112 ) ) ;
#6795 = CARTESIAN_POINT ( 'NONE',  ( 4.921717144059290838, 36.96778581912766271, -7.986823970829891373 ) ) ;
#6796 = CARTESIAN_POINT ( 'NONE',  ( -6.811226782241547539, 35.33967249274200384, 10.50000000000000355 ) ) ;
#6797 = DIRECTION ( 'NONE',  ( 0.6123724356957939152, -0.3535533905932699561, -0.7071067811865499042 ) ) ;
#6798 = DIRECTION ( 'NONE',  ( -0.5000000000000038858, -0.8660254037844363761, 0.000000000000000000 ) ) ;
#6799 = CARTESIAN_POINT ( 'NONE',  ( -7.014595103779441843, 35.79644522156330311, 11.00000000000000000 ) ) ;
#6800 = DIRECTION ( 'NONE',  ( -0.1045284632676415082, 0.9945218953682745111, 0.000000000000000000 ) ) ;
#6801 = CARTESIAN_POINT ( 'NONE',  ( -1.623738443162547007, 19.56555719779890978, 12.00000000000000000 ) ) ;
#6802 = VECTOR ( 'NONE', #10528, 1000.000000000000000 ) ;
#6803 = CARTESIAN_POINT ( 'NONE',  ( 15.22299664760056537, 27.42699395385487904, -5.000000000000000000 ) ) ;
#6804 = CARTESIAN_POINT ( 'NONE',  ( 0.000000000000000000, 22.50000000000000355, 7.000000000000000000 ) ) ;
#6805 = VERTEX_POINT ( 'NONE', #4623 ) ;
#6807 = DIRECTION ( 'NONE',  ( -0.2876062384759714985, -0.6459741880212498399, -0.7071067811865401342 ) ) ;
#6806 = CARTESIAN_POINT ( 'NONE',  ( -16.30574288886405654, 14.63324257956979224, -21.08092481694252029 ) ) ;
#6808 = CARTESIAN_POINT ( 'NONE',  ( 37.58754968649119377, -10.91577297561529036, 10.99999999999992717 ) ) ;
#6809 = ADVANCED_FACE ( 'NONE', ( #29403 ), #10117, .T. ) ;
#6810 = CARTESIAN_POINT ( 'NONE',  ( 9.486164890912217373, -18.17313361576023212, -30.00000000000000000 ) ) ;
#6811 = EDGE_CURVE ( 'NONE', #14009, #7, #10416, .T. ) ;
#6812 = CARTESIAN_POINT ( 'NONE',  ( -1.204925152852743597, 12.02153850147729486, 10.50000000000000355 ) ) ;
#6813 = CARTESIAN_POINT ( 'NONE',  ( 11.89393184209717624, 19.38028970819429020, -21.61737904418150436 ) ) ;
#6814 = ORIENTED_EDGE ( 'NONE', *, *, #6738, .F. ) ;
#6815 = CARTESIAN_POINT ( 'NONE',  ( 10.96874445820387223, 17.31868006298826046, -30.00000000000000000 ) ) ;
#6816 = EDGE_LOOP ( 'NONE', ( #18602, #26748 ) ) ;
#6817 = CIRCLE ( 'NONE', #29544, 1.000000000000004441 ) ;
#6818 = LINE ( 'NONE', #4182, #9483 ) ;
#6819 = CARTESIAN_POINT ( 'NONE',  ( -11.84263605179389778, -21.48980687254330846, -18.45847382795814795 ) ) ;
#6820 = CARTESIAN_POINT ( 'NONE',  ( -32.28722999652134007, 1.315479119631538074, 12.14047268033097282 ) ) ;
#6821 = VECTOR ( 'NONE', #36454, 1000.000000000000000 ) ;
#6822 = AXIS2_PLACEMENT_3D ( 'NONE', #17949, #2305, #5538 ) ;
#6823 = CARTESIAN_POINT ( 'NONE',  ( -28.89889151792434063, -21.30051352786605179, -10.18607909959966840 ) ) ;
#6824 = CARTESIAN_POINT ( 'NONE',  ( -4.782499769022778402, -24.84304998847331092, -6.931069079744395012 ) ) ;
#6825 = CARTESIAN_POINT ( 'NONE',  ( 12.08418194466055695, 18.52621323336339287, -22.79847468729924742 ) ) ;
#6826 = ORIENTED_EDGE ( 'NONE', *, *, #31867, .F. ) ;
#6827 = CARTESIAN_POINT ( 'NONE',  ( 18.77593942704109509, 8.755078447771618144, -26.61273691426299592 ) ) ;
#6828 = CARTESIAN_POINT ( 'NONE',  ( 11.44473057578109199, 31.45924896672603310, 10.50000000000000178 ) ) ;
#6829 = CARTESIAN_POINT ( 'NONE',  ( 1.621626408465995040, 37.48425883190013508, 17.42190598798392642 ) ) ;
#6830 = ORIENTED_EDGE ( 'NONE', *, *, #5808, .F. ) ;
#6831 = CARTESIAN_POINT ( 'NONE',  ( -33.48494503266941535, -3.494085805712010107, -5.909783893160384771 ) ) ;
#6832 = CARTESIAN_POINT ( 'NONE',  ( -19.27886458632313094, 17.11073565397887819, 15.72805884748862404 ) ) ;
#6833 = VERTEX_POINT ( 'NONE', #28799 ) ;
#6834 = FACE_OUTER_BOUND ( 'NONE', #3650, .T. ) ;
#6835 = CARTESIAN_POINT ( 'NONE',  ( 10.29511041547405625, 24.79362192464176573, 10.50000000000000000 ) ) ;
#6836 = CARTESIAN_POINT ( 'NONE',  ( -28.42036332966587509, 2.623993810986072095, -5.000000000000000000 ) ) ;
#6837 = ADVANCED_FACE ( 'NONE', ( #975 ), #13356, .T. ) ;
#6838 = CARTESIAN_POINT ( 'NONE',  ( 19.38136568836685925, -7.835196129137437460, -26.99971740741212756 ) ) ;
#6839 = CARTESIAN_POINT ( 'NONE',  ( 29.80853493429485468, -25.87953118561181753, 12.73282698324837092 ) ) ;
#6840 = ORIENTED_EDGE ( 'NONE', *, *, #9229, .T. ) ;
#6841 = ORIENTED_EDGE ( 'NONE', *, *, #18962, .F. ) ;
#6842 = DIRECTION ( 'NONE',  ( -0.6691306063588569053, 0.7431448254773954654, 0.000000000000000000 ) ) ;
#6843 = VECTOR ( 'NONE', #6127, 1000.000000000000114 ) ;
#6844 = CARTESIAN_POINT ( 'NONE',  ( 18.74997338758756271, -3.362744936767421589, 23.00000000000000000 ) ) ;
#6845 = AXIS2_PLACEMENT_3D ( 'NONE', #18228, #27760, #11531 ) ;
#6846 = CIRCLE ( 'NONE', #12717, 1.000000000000000888 ) ;
#6847 = CARTESIAN_POINT ( 'NONE',  ( 7.530592408760851342, 11.28437794979193853, 7.000000000000000000 ) ) ;
#6848 = ORIENTED_EDGE ( 'NONE', *, *, #31935, .F. ) ;
#6849 = CARTESIAN_POINT ( 'NONE',  ( -0.7383155542429340468, 37.49228970066121747, -8.404103827552029671 ) ) ;
#6850 = PLANE ( 'NONE',  #13291 ) ;
#6851 = CARTESIAN_POINT ( 'NONE',  ( -9.427394655428429360, 11.06314620770957013, 7.500000000000000888 ) ) ;
#6852 = CARTESIAN_POINT ( 'NONE',  ( -10.73859285986284640, 31.49625607628545154, 7.000000000000000000 ) ) ;
#6853 = PLANE ( 'NONE',  #2223 ) ;
#6854 = CARTESIAN_POINT ( 'NONE',  ( 13.94482798346721353, 26.50521816028912525, 7.500000000000000888 ) ) ;
#6855 = CARTESIAN_POINT ( 'NONE',  ( 10.39566615896967683, 22.74892090402041944, -19.14879625716820044 ) ) ;
#6856 = CARTESIAN_POINT ( 'NONE',  ( -11.87435565298220475, 15.06698729810788961, 7.499999999999993783 ) ) ;
#6857 = EDGE_LOOP ( 'NONE', ( #26177, #27169, #14502, #32129 ) ) ;
#6859 = CARTESIAN_POINT ( 'NONE',  ( -8.843266739736657556, 16.81698729810786830, 10.50000000000000000 ) ) ;
#6858 = CARTESIAN_POINT ( 'NONE',  ( -19.27084013280208197, 11.49840606477986071, -18.02072584537811650 ) ) ;
#6860 = CARTESIAN_POINT ( 'NONE',  ( -4.331888854854716975, 42.14502281367647640, 23.00000000000000000 ) ) ;
#6861 = CARTESIAN_POINT ( 'NONE',  ( 9.609346625839055633, -18.25387553414934771, -28.07524107909567590 ) ) ;
#6862 = CARTESIAN_POINT ( 'NONE',  ( 1.500000000000000888, 37.00000000000000711, 7.000000000000000000 ) ) ;
#6863 = CARTESIAN_POINT ( 'NONE',  ( 14.91174806184727153, 25.87366738573922120, -9.704845141577239431 ) ) ;
#6864 = EDGE_CURVE ( 'NONE', #16240, #18297, #15654, .T. ) ;
#6865 = CARTESIAN_POINT ( 'NONE',  ( 5.636483973512839363, -22.01575377102105691, -30.00000000000001421 ) ) ;
#6866 = CARTESIAN_POINT ( 'NONE',  ( 7.713869163865850531, 10.18146832927074996, 9.500000000000000000 ) ) ;
#6867 = ADVANCED_FACE ( 'NONE', ( #24109 ), #2383, .T. ) ;
#6868 = CARTESIAN_POINT ( 'NONE',  ( -14.97360822305132722, -15.86213100947220944, -24.45481922633826599 ) ) ;
#6869 = CARTESIAN_POINT ( 'NONE',  ( 7.307221220942812678, -22.95671206205766524, -15.78720648459951192 ) ) ;
#6870 = CARTESIAN_POINT ( 'NONE',  ( 15.49934645862682103, 26.48612375915841710, -5.474131244744144809 ) ) ;
#6871 = CARTESIAN_POINT ( 'NONE',  ( 16.96937371531925365, -12.22095849417253532, -26.98299665146808834 ) ) ;
#6872 = CARTESIAN_POINT ( 'NONE',  ( -6.811226782241547539, 35.33967249274200384, 10.50000000000000355 ) ) ;
#6873 = CARTESIAN_POINT ( 'NONE',  ( -38.86091370594022010, -6.124650435543221860, 11.00000000000000000 ) ) ;
#6874 = ORIENTED_EDGE ( 'NONE', *, *, #24797, .T. ) ;
#6875 = CARTESIAN_POINT ( 'NONE',  ( -6.226819983209127329, 23.40422832001528519, -20.90460070830227224 ) ) ;
#6876 = AXIS2_PLACEMENT_3D ( 'NONE', #35570, #5089, #19931 ) ;
#6877 = VECTOR ( 'NONE', #35474, 1000.000000000000114 ) ;
#6878 = CARTESIAN_POINT ( 'NONE',  ( 14.81003276707481575, 21.44615697153870570, 10.87262190629277825 ) ) ;
#6879 = ORIENTED_EDGE ( 'NONE', *, *, #25880, .F. ) ;
#6880 = CARTESIAN_POINT ( 'NONE',  ( 21.71290527652266888, 0.7082383630531658980, -23.85174149327086113 ) ) ;
#6881 = DIRECTION ( 'NONE',  ( -0.3090169943749574988, -0.9510565162951503115, 0.000000000000000000 ) ) ;
#6882 = AXIS2_PLACEMENT_3D ( 'NONE', #18084, #12175, #27215 ) ;
#6883 = DIRECTION ( 'NONE',  ( -0.9986295347545744994, -0.05233595624293203852, 0.000000000000000000 ) ) ;
#6884 = ORIENTED_EDGE ( 'NONE', *, *, #15345, .T. ) ;
#6885 = CARTESIAN_POINT ( 'NONE',  ( -23.92393967644365915, 0.5257180683408601007, -19.50104800721178577 ) ) ;
#6886 = DIRECTION ( 'NONE',  ( -0.9135454576426059736, -0.4067366430757887730, 0.000000000000000000 ) ) ;
#6887 = EDGE_CURVE ( 'NONE', #6898, #7015, #30560, .T. ) ;
#6888 = ORIENTED_EDGE ( 'NONE', *, *, #20284, .F. ) ;
#6889 = CARTESIAN_POINT ( 'NONE',  ( 20.09314088254942021, -4.111701498484372053, -29.99999999999998579 ) ) ;
#6890 = EDGE_CURVE ( 'NONE', #959, #2993, #25984, .T. ) ;
#6891 = ORIENTED_EDGE ( 'NONE', *, *, #18373, .F. ) ;
#6892 = CARTESIAN_POINT ( 'NONE',  ( -12.44178368932711543, 35.65276919562048619, 11.55979286843954057 ) ) ;
#6893 = CARTESIAN_POINT ( 'NONE',  ( 16.72075857324119141, 7.444561356925491147, 7.000000000000000000 ) ) ;
#6894 = CARTESIAN_POINT ( 'NONE',  ( 6.864468484318075880, 35.45925531351068116, 10.49999999999999822 ) ) ;
#6895 = CARTESIAN_POINT ( 'NONE',  ( -10.16357496796715054, 29.39421982382238596, 19.27171037444156454 ) ) ;
#6896 = EDGE_CURVE ( 'NONE', #40197, #1489, #23414, .T. ) ;
#6897 = LINE ( 'NONE', #13402, #13589 ) ;
#6898 = VERTEX_POINT ( 'NONE', #29806 ) ;
#6899 = CARTESIAN_POINT ( 'NONE',  ( 3.553336972204391042, 8.187731063815824939, 10.94387467463491959 ) ) ;
#6900 = CARTESIAN_POINT ( 'NONE',  ( -10.25710140050888519, 17.79863391756059698, -30.00000000000000000 ) ) ;
#6901 = DIRECTION ( 'NONE',  ( 0.000000000000000000, 0.000000000000000000, 1.000000000000000000 ) ) ;
#6902 = DIRECTION ( 'NONE',  ( -0.9135454576426051965, -0.4067366430757904938, 0.000000000000000000 ) ) ;
#6903 = CARTESIAN_POINT ( 'NONE',  ( 18.00529160253907079, 18.80124742017171968, -7.886222486033878099 ) ) ;
#6904 = CARTESIAN_POINT ( 'NONE',  ( 5.103355680224398228, 19.86390335519187289, -30.00000000000000355 ) ) ;
#6905 = VECTOR ( 'NONE', #22817, 1000.000000000000000 ) ;
#6906 = VERTEX_POINT ( 'NONE', #5022 ) ;
#6907 = CARTESIAN_POINT ( 'NONE',  ( 10.39682445600779026, -18.27815074178298360, -26.16533906555415356 ) ) ;
#6908 = CARTESIAN_POINT ( 'NONE',  ( -3.456468065140303025, 26.15323006594351440, 21.00000000000000000 ) ) ;
#6909 = ADVANCED_FACE ( 'NONE', ( #20873 ), #18222, .T. ) ;
#6910 = CARTESIAN_POINT ( 'NONE',  ( 0.7624269476132105039, 37.48077593123142748, 7.455539900862801161 ) ) ;
#6911 = EDGE_CURVE ( 'NONE', #2141, #22956, #30007, .T. ) ;
#6912 = EDGE_LOOP ( 'NONE', ( #36040, #6765 ) ) ;
#6913 = CARTESIAN_POINT ( 'NONE',  ( -13.49222746860650624, 22.81367680405242382, -15.45099856532659643 ) ) ;
#6914 = CARTESIAN_POINT ( 'NONE',  ( -31.75251099004362132, -1.565804367082550996, 16.87380292611436872 ) ) ;
#6915 = CARTESIAN_POINT ( 'NONE',  ( 13.01178723928756575, -23.59175502374137778, -14.49606265435651764 ) ) ;
#6916 = FACE_OUTER_BOUND ( 'NONE', #14736, .T. ) ;
#6917 = ORIENTED_EDGE ( 'NONE', *, *, #26253, .F. ) ;
#6918 = VERTEX_POINT ( 'NONE', #36505 ) ;
#6919 = CARTESIAN_POINT ( 'NONE',  ( -13.17720483057398972, 28.77380982630769424, -10.45774930547776904 ) ) ;
#6920 = CARTESIAN_POINT ( 'NONE',  ( -14.51034694435784722, -19.54383023510037276, -20.13759940241521207 ) ) ;
#6921 = FACE_BOUND ( 'NONE', #18921, .T. ) ;
#6922 = CARTESIAN_POINT ( 'NONE',  ( -27.13658926588106723, -5.861905960888289080, -16.87029009801329593 ) ) ;
#6923 = DIRECTION ( 'NONE',  ( 0.9781476007338042455, -0.2079116908177663647, 0.000000000000000000 ) ) ;
#6924 = ORIENTED_EDGE ( 'NONE', *, *, #19107, .F. ) ;
#6925 = CARTESIAN_POINT ( 'NONE',  ( 20.47688798105681940, 0.9740165025114797537, -29.35045312999529799 ) ) ;
#6926 = LINE ( 'NONE', #650, #18727 ) ;
#6927 = CARTESIAN_POINT ( 'NONE',  ( -12.03641663870442713, 15.85735326529964873, 13.00000000000000178 ) ) ;
#6928 = VERTEX_POINT ( 'NONE', #30614 ) ;
#6929 = CARTESIAN_POINT ( 'NONE',  ( -30.92750986253986767, -0.06599190286722676768, -5.474045238037080985 ) ) ;
#6930 = CARTESIAN_POINT ( 'NONE',  ( -25.01235460169770519, -30.53116334361912365, 10.99999999999999822 ) ) ;
#6931 = EDGE_CURVE ( 'NONE', #9898, #751, #37044, .T. ) ;
#6932 = EDGE_LOOP ( 'NONE', ( #8435, #35748, #18153, #18927 ) ) ;
#6933 = CARTESIAN_POINT ( 'NONE',  ( 20.88296681861968551, -0.3172434910415447007, -26.74114674371728029 ) ) ;
#6934 = AXIS2_PLACEMENT_3D ( 'NONE', #14750, #21046, #27139 ) ;
#6935 = LINE ( 'NONE', #34784, #26533 ) ;
#6936 = CARTESIAN_POINT ( 'NONE',  ( 35.58257249438514691, -10.95300747732849977, 16.30093088680188629 ) ) ;
#6937 = EDGE_CURVE ( 'NONE', #1084, #24976, #23355, .T. ) ;
#6938 = ORIENTED_EDGE ( 'NONE', *, *, #34399, .F. ) ;
#6939 = CARTESIAN_POINT ( 'NONE',  ( -13.63376536442988396, 31.74814110635680464, 15.72805884748939143 ) ) ;
#6940 = AXIS2_PLACEMENT_3D ( 'NONE', #17424, #2174, #29592 ) ;
#6941 = CARTESIAN_POINT ( 'NONE',  ( 5.537946624086020009, 36.44027069998191593, 7.000000000000000000 ) ) ;
#6942 = CARTESIAN_POINT ( 'NONE',  ( -2.787905735463278134, 28.53453732066314430, 20.94377226548378701 ) ) ;
#6943 = CARTESIAN_POINT ( 'NONE',  ( 10.36702044712426840, 31.16169077310587809, 10.00000000000000000 ) ) ;
#6944 = CARTESIAN_POINT ( 'NONE',  ( 11.69134295108989008, 15.74999999999995204, 7.000000000000000000 ) ) ;
#6945 = FACE_BOUND ( 'NONE', #37491, .T. ) ;
#6946 = CARTESIAN_POINT ( 'NONE',  ( 28.78471548569376282, -2.122417091767359931, 18.87996532025784546 ) ) ;
#6947 = CARTESIAN_POINT ( 'NONE',  ( -22.14118475150960563, 9.614454132667919595, -11.87011620208269314 ) ) ;
#6948 = CARTESIAN_POINT ( 'NONE',  ( 20.22886225973998719, -23.64398365531091528, -13.09675354266916258 ) ) ;
#6949 = CARTESIAN_POINT ( 'NONE',  ( 11.20572440089081390, 18.11902114148211851, -25.00021980855870396 ) ) ;
#6950 = VECTOR ( 'NONE', #38679, 999.9999999999998863 ) ;
#6951 = ORIENTED_EDGE ( 'NONE', *, *, #6248, .F. ) ;
#6953 = CIRCLE ( 'NONE', #3750, 6.000000000000003553 ) ;
#6952 = CARTESIAN_POINT ( 'NONE',  ( -12.63699674669057949, 17.97954234152161490, -22.88184407339303661 ) ) ;
#6954 = CARTESIAN_POINT ( 'NONE',  ( -26.19533169775672476, -16.15700992729037466, 20.69868183039762144 ) ) ;
#6955 = CARTESIAN_POINT ( 'NONE',  ( 10.61811999842815801, 32.73341455422742285, 10.94387467463499242 ) ) ;
#6956 = CARTESIAN_POINT ( 'NONE',  ( 11.71173409423554190, 18.88690681544503391, -22.73936493488036703 ) ) ;
#6957 = VERTEX_POINT ( 'NONE', #5616 ) ;
#6958 = CARTESIAN_POINT ( 'NONE',  ( 33.01650362960521079, -18.20503022527935855, -7.971919029728472772 ) ) ;
#6959 = ADVANCED_FACE ( 'NONE', ( #11327 ), #31188, .T. ) ;
#6960 = DIRECTION ( 'NONE',  ( 0.7431448254773862505, -0.6691306063588670083, 0.000000000000000000 ) ) ;
#6961 = ORIENTED_EDGE ( 'NONE', *, *, #26501, .F. ) ;
#6962 = CIRCLE ( 'NONE', #25801, 1.000000000000000000 ) ;
#6964 = DIRECTION ( 'NONE',  ( 0.6459741880212486187, -0.2876062384759502932, -0.7071067811865500152 ) ) ;
#6963 = CARTESIAN_POINT ( 'NONE',  ( -15.09307680312074140, 26.86446856943478423, -7.812756861724547974 ) ) ;
#6965 = CARTESIAN_POINT ( 'NONE',  ( -14.00048334364361402, -23.68480630221392147, -14.41671907191942559 ) ) ;
#6966 = CARTESIAN_POINT ( 'NONE',  ( 12.60100158617205857, 14.64745807297493663, 10.87262190629442671 ) ) ;
#6967 = AXIS2_PLACEMENT_3D ( 'NONE', #8856, #21047, #8653 ) ;
#6968 = ORIENTED_EDGE ( 'NONE', *, *, #290, .F. ) ;
#6969 = CARTESIAN_POINT ( 'NONE',  ( -23.12572148637181257, -11.24311462695209585, -19.64121234349231315 ) ) ;
#6970 = CARTESIAN_POINT ( 'NONE',  ( -12.26289438224282158, -23.05663733951990935, -15.49923916903545340 ) ) ;
#6971 = DIRECTION ( 'NONE',  ( 0.000000000000000000, 0.000000000000000000, 1.000000000000000000 ) ) ;
#6972 = CARTESIAN_POINT ( 'NONE',  ( 15.87663021223514548, 23.08495078608549633, -9.753722227093680530 ) ) ;
#6973 = EDGE_LOOP ( 'NONE', ( #20708, #30992, #5057, #11296 ) ) ;
#6974 = CARTESIAN_POINT ( 'NONE',  ( 27.02756462025498152, 2.904459085774969473, -10.73325283292277099 ) ) ;
#6975 = CARTESIAN_POINT ( 'NONE',  ( 9.183240348400453001, 28.21559575157615996, 13.00000000000000178 ) ) ;
#6976 = CARTESIAN_POINT ( 'NONE',  ( -23.43324262027536875, -8.134040356058614307, 23.00000000000000000 ) ) ;
#6977 = FACE_OUTER_BOUND ( 'NONE', #20264, .T. ) ;
#6978 = ORIENTED_EDGE ( 'NONE', *, *, #29239, .F. ) ;
#6979 = CARTESIAN_POINT ( 'NONE',  ( -22.92914194212210788, -0.07278265280095547185, -21.52489520804394019 ) ) ;
#6980 = CARTESIAN_POINT ( 'NONE',  ( 22.27536895993342014, 0.4410975482186068053, -22.70620645469208654 ) ) ;
#6981 = CARTESIAN_POINT ( 'NONE',  ( 17.81343984362198540, -22.72844136247426761, 19.66345542862503137 ) ) ;
#6982 = ORIENTED_EDGE ( 'NONE', *, *, #19398, .T. ) ;
#6983 = CIRCLE ( 'NONE', #29709, 0.5000000000000004441 ) ;
#6984 = CARTESIAN_POINT ( 'NONE',  ( -35.84808252048276955, -3.038699442442200027, -5.000000000000002665 ) ) ;
#6985 = CARTESIAN_POINT ( 'NONE',  ( 0.5000000000000012212, 31.00000000000000355, 9.000000000000001776 ) ) ;
#6986 = AXIS2_PLACEMENT_3D ( 'NONE', #35586, #25423, #7134 ) ;
#6987 = AXIS2_PLACEMENT_3D ( 'NONE', #24039, #1710, #5153 ) ;
#6988 = VERTEX_POINT ( 'NONE', #18026 ) ;
#6989 = EDGE_CURVE ( 'NONE', #9581, #39411, #3948, .T. ) ;
#6990 = CARTESIAN_POINT ( 'NONE',  ( -7.951799764322637465, 28.98701630243970229, 10.74999999999999467 ) ) ;
#6991 = AXIS2_PLACEMENT_3D ( 'NONE', #17674, #30048, #27393 ) ;
#6992 = AXIS2_PLACEMENT_3D ( 'NONE', #7490, #19283, #1006 ) ;
#6993 = CARTESIAN_POINT ( 'NONE',  ( -11.44473057578097475, 31.45924896672618587, 10.49999999999999822 ) ) ;
#6994 = CARTESIAN_POINT ( 'NONE',  ( 17.06447150072999719, 21.55760828791484585, -5.000000000000003553 ) ) ;
#6995 = CARTESIAN_POINT ( 'NONE',  ( 5.880870157263162312, 35.77077879190645149, -9.310133446813710023 ) ) ;
#6996 = LINE ( 'NONE', #21651, #17235 ) ;
#6997 = ORIENTED_EDGE ( 'NONE', *, *, #37595, .T. ) ;
#6998 = DIRECTION ( 'NONE',  ( 1.000000000000000000, 0.000000000000000000, 0.000000000000000000 ) ) ;
#6999 = CARTESIAN_POINT ( 'NONE',  ( -3.610593701936590350, 31.83882289796395426, 10.50000000000000533 ) ) ;
#7000 = CARTESIAN_POINT ( 'NONE',  ( 17.14449823358358316, -14.87368394026793972, -23.09499826230010200 ) ) ;
#7001 = B_SPLINE_CURVE_WITH_KNOTS ( 'NONE', 3,
 ( #31839, #25536, #31642, #23098, #16814, #22488, #1168, #10508, #4004, #32249, #3807, #29200, #7047, #16405, #967, #13348, #32042, #25739, #22691, #35091 ),
 .UNSPECIFIED., .F., .F.,
 ( 4, 2, 1, 1, 1, 1, 1, 1, 2, 2, 2, 2, 4 ),
 ( 0.000000000000000000, 0.0009765625000000435849, 0.001953125000000087170, 0.003906250000000174340, 0.007812500000000305311, 0.01562500000000027409, 0.03125000000000020817, 0.06250000000000018041, 0.1250000000000000278, 0.2499999999999998890, 0.5000000000000000000, 0.7500000000000000000, 1.000000000000000000 ),
 .UNSPECIFIED. ) ;
#7002 = DIRECTION ( 'NONE',  ( 0.000000000000000000, 0.000000000000000000, -1.000000000000000000 ) ) ;
#7003 = LINE ( 'NONE', #4368, #211 ) ;
#7004 = CARTESIAN_POINT ( 'NONE',  ( 10.49474413300069386, 21.89971208337374264, 10.00000000000000000 ) ) ;
#7005 = CARTESIAN_POINT ( 'NONE',  ( 15.13246232760047505, 27.45171539379471781, -6.404961841383983945 ) ) ;
#7006 = DIRECTION ( 'NONE',  ( -0.5877852522924796874, -0.8090169943749426773, 0.000000000000000000 ) ) ;
#7007 = ORIENTED_EDGE ( 'NONE', *, *, #17824, .T. ) ;
#7009 = CARTESIAN_POINT ( 'NONE',  ( 2.141014423449929094, 7.887532638883552494, 10.49999999999999822 ) ) ;
#7008 = CARTESIAN_POINT ( 'NONE',  ( -16.71939040854026715, 19.69829189495437305, -11.75715933036468286 ) ) ;
#7010 = CARTESIAN_POINT ( 'NONE',  ( 32.33143948541787438, 1.358872982501792226, 2.999999999999999112 ) ) ;
#7011 = ADVANCED_FACE ( 'NONE', ( #5426 ), #7420, .T. ) ;
#7012 = CARTESIAN_POINT ( 'NONE',  ( 10.22002048505811800, -19.16611505460419806, -23.85456539383813990 ) ) ;
#7013 = CARTESIAN_POINT ( 'NONE',  ( -11.11016527260153808, 31.83082137946488643, 7.000000000000000000 ) ) ;
#7014 = CARTESIAN_POINT ( 'NONE',  ( 13.21628872672062194, 22.22346690588532425, -16.44513725962594819 ) ) ;
#7015 = VERTEX_POINT ( 'NONE', #19202 ) ;
#7016 = CARTESIAN_POINT ( 'NONE',  ( 15.33694215129142790, 26.62211003415141164, -6.887897498730079171 ) ) ;
#7017 = ORIENTED_EDGE ( 'NONE', *, *, #32946, .T. ) ;
#7019 = CARTESIAN_POINT ( 'NONE',  ( 14.26801110064894829, 26.12045026487100330, 10.49999999999999822 ) ) ;
#7018 = CARTESIAN_POINT ( 'NONE',  ( -13.75448907894945805, 23.42996800784982270, -14.47271240302549700 ) ) ;
#7020 = CARTESIAN_POINT ( 'NONE',  ( -10.82815314884593860, -19.99260957008704409, -21.61855094834904989 ) ) ;
#7021 = CARTESIAN_POINT ( 'NONE',  ( -37.52525227335131319, -10.91693234368756649, 12.14047268033150573 ) ) ;
#7022 = AXIS2_PLACEMENT_3D ( 'NONE', #1454, #34777, #10193 ) ;
#7023 = CARTESIAN_POINT ( 'NONE',  ( -30.92874242133839502, -21.35189250303394815, -7.976690102107105496 ) ) ;
#7024 = CARTESIAN_POINT ( 'NONE',  ( -3.280732279199019441, -20.30841954709158870, -28.85152870245993739 ) ) ;
#7025 = CARTESIAN_POINT ( 'NONE',  ( 15.59458766223087167, 25.74192377969740519, -6.889944325882612297 ) ) ;
#7026 = ADVANCED_FACE ( 'NONE', ( #30810 ), #26657, .T. ) ;
#7027 = VERTEX_POINT ( 'NONE', #6013 ) ;
#7028 = CARTESIAN_POINT ( 'NONE',  ( 20.04105427597066225, 10.14435442418174738, -18.01185279135228257 ) ) ;
#7029 = CARTESIAN_POINT ( 'NONE',  ( -11.69134295108998245, 15.75000000000011191, 7.000000000000000000 ) ) ;
#7030 = EDGE_CURVE ( 'NONE', #14313, #10247, #33863, .T. ) ;
#7031 = CARTESIAN_POINT ( 'NONE',  ( -11.00933375873403541, 31.84550678200677609, 17.92354375535249389 ) ) ;
#7032 = AXIS2_PLACEMENT_3D ( 'NONE', #33419, #8819, #17969 ) ;
#7033 = ORIENTED_EDGE ( 'NONE', *, *, #15425, .T. ) ;
#7034 = CARTESIAN_POINT ( 'NONE',  ( -30.79476031969355176, -3.968954442311656283, -12.24617189075128643 ) ) ;
#7035 = VECTOR ( 'NONE', #23941, 1000.000000000000000 ) ;
#7036 = CARTESIAN_POINT ( 'NONE',  ( -17.35626706996358237, 16.20628521381909337, 17.92354375535225586 ) ) ;
#7037 = ORIENTED_EDGE ( 'NONE', *, *, #39171, .T. ) ;
#7038 = CARTESIAN_POINT ( 'NONE',  ( 19.30730118283918983, -16.27608008926518579, 20.99999999999999645 ) ) ;
#7039 = CARTESIAN_POINT ( 'NONE',  ( 19.48557158514975285, -11.24999999999995737, 10.00000000000000000 ) ) ;
#7040 = CARTESIAN_POINT ( 'NONE',  ( 34.65956455088738153, -16.45432426470986798, -4.999999999999995559 ) ) ;
#7041 = CARTESIAN_POINT ( 'NONE',  ( 20.78373334066920108, -29.14101728923875356, 12.14047268033096927 ) ) ;
#7042 = ORIENTED_EDGE ( 'NONE', *, *, #28148, .T. ) ;
#7043 = EDGE_CURVE ( 'NONE', #11758, #12092, #24904, .T. ) ;
#7044 = ORIENTED_EDGE ( 'NONE', *, *, #15955, .T. ) ;
#7045 = EDGE_CURVE ( 'NONE', #37653, #6642, #12119, .T. ) ;
#7046 = DIRECTION ( 'NONE',  ( 1.000000000000000000, 0.000000000000000000, 0.000000000000000000 ) ) ;
#7047 = CARTESIAN_POINT ( 'NONE',  ( -17.56752247727831673, 20.37189381199461025, -4.999999999999999112 ) ) ;
#7048 = AXIS2_PLACEMENT_3D ( 'NONE', #25360, #34918, #9932 ) ;
#7049 = CIRCLE ( 'NONE', #23949, 1.000000000000009548 ) ;
#7050 = CYLINDRICAL_SURFACE ( 'NONE', #30485, 0.5000000000000004441 ) ;
#7051 = VERTEX_POINT ( 'NONE', #325 ) ;
#7052 = CARTESIAN_POINT ( 'NONE',  ( -0.5950768495228482280, 30.23063772115626691, -15.67701037968547872 ) ) ;
#7053 = DIRECTION ( 'NONE',  ( 1.000000000000000000, 0.000000000000000000, 0.000000000000000000 ) ) ;
#7054 = LINE ( 'NONE', #19867, #11735 ) ;
#7055 = AXIS2_PLACEMENT_3D ( 'NONE', #21154, #27447, #11419 ) ;
#7056 = CARTESIAN_POINT ( 'NONE',  ( -9.541476348891238857, 27.59512447410525127, 13.00000000000000178 ) ) ;
#7057 = CARTESIAN_POINT ( 'NONE',  ( -1.000000000000000000, 37.00000000000000711, 7.500000000000000888 ) ) ;
#7058 = CARTESIAN_POINT ( 'NONE',  ( 6.980762143445869761, 14.59310681135549537, 10.49999999999999645 ) ) ;
#7059 = CARTESIAN_POINT ( 'NONE',  ( 10.89816891502054830, 21.26322318888422558, -20.31437330493695370 ) ) ;
#7060 = DIRECTION ( 'NONE',  ( 0.6123724356958033521, 0.3535533905932687349, -0.7071067811865423547 ) ) ;
#7061 = ORIENTED_EDGE ( 'NONE', *, *, #32229, .F. ) ;
#7063 = CARTESIAN_POINT ( 'NONE',  ( -12.30736835487443415, 14.81698729810790560, 11.00000000000000000 ) ) ;
#7062 = CARTESIAN_POINT ( 'NONE',  ( -19.67958062024562338, 15.63688475377917086, -5.964679019702594509 ) ) ;
#7064 = CARTESIAN_POINT ( 'NONE',  ( 3.503793317224329851, 8.420815634768676006, 7.000000000000000000 ) ) ;
#7065 = CARTESIAN_POINT ( 'NONE',  ( 10.88014080686398977, -19.98056130176378531, -21.61155136698059209 ) ) ;
#7066 = CARTESIAN_POINT ( 'NONE',  ( -3.399837471815634338, 8.909889435135630364, 9.500000000000000000 ) ) ;
#7067 = CARTESIAN_POINT ( 'NONE',  ( 11.44734449680894350, 18.46921977093748524, -23.84809478162342700 ) ) ;
#7068 = CARTESIAN_POINT ( 'NONE',  ( 2.927345865710861972E-15, 22.57051819516765789, -19.69475445967420768 ) ) ;
#7069 = EDGE_CURVE ( 'NONE', #4297, #9720, #31591, .T. ) ;
#7070 = CARTESIAN_POINT ( 'NONE',  ( -9.559512017365660697, 19.71884705062586107, 13.00000000000000178 ) ) ;
#7071 = CARTESIAN_POINT ( 'NONE',  ( -17.16483700087839992, -17.10857606624298199, -20.90193344114118190 ) ) ;
#7072 = CARTESIAN_POINT ( 'NONE',  ( 6.178680871570535693, -24.89148437011798620, -7.894064581684323123 ) ) ;
#7073 = CARTESIAN_POINT ( 'NONE',  ( 11.32202086828915100, 17.65615535816628423, -26.23948895313833063 ) ) ;
#7074 = CARTESIAN_POINT ( 'NONE',  ( 30.42719773241262260, -20.61230597470657955, -9.287414125035716950 ) ) ;
#7075 = DIRECTION ( 'NONE',  ( 0.8090169943749505599, 0.5877852522924689183, -0.000000000000000000 ) ) ;
#7076 = CARTESIAN_POINT ( 'NONE',  ( -8.412270287199726582, 10.07085245822961994, 10.49999999999999822 ) ) ;
#7077 = EDGE_LOOP ( 'NONE', ( #13585, #2214, #19534, #37744 ) ) ;
#7078 = CARTESIAN_POINT ( 'NONE',  ( -6.993233941076627325, 29.63588997363762090, -14.83726457422114287 ) ) ;
#7079 = CIRCLE ( 'NONE', #14225, 1.000000000000000000 ) ;
#7080 = CARTESIAN_POINT ( 'NONE',  ( 14.96161608456799463, 21.61429412723660093, 10.49999999999999822 ) ) ;
#7081 = ORIENTED_EDGE ( 'NONE', *, *, #28529, .F. ) ;
#7082 = CARTESIAN_POINT ( 'NONE',  ( 25.88303574148295993, 0.2867772994816546461, -16.43952562929733219 ) ) ;
#7083 = DIRECTION ( 'NONE',  ( -0.000000000000000000, 0.000000000000000000, -1.000000000000000000 ) ) ;
#7084 = CARTESIAN_POINT ( 'NONE',  ( -0.5000000000000005551, 31.00000000000000355, 7.000000000000000000 ) ) ;
#7085 = B_SPLINE_CURVE_WITH_KNOTS ( 'NONE', 3,
 ( #25751, #22304, #16417, #9923, #40039, #36803 ),
 .UNSPECIFIED., .F., .F.,
 ( 4, 2, 4 ),
 ( 0.000000000000000000, 0.5000000000000008882, 1.000000000000000000 ),
 .UNSPECIFIED. ) ;
#7086 = VECTOR ( 'NONE', #28247, 1000.000000000000000 ) ;
#7087 = PRODUCT ( 'Detachable Washable Trimmer Head Cap', 'Detachable Washable Trimmer Head Cap', '', ( #29641 ) ) ;
#7088 = ORIENTED_EDGE ( 'NONE', *, *, #35796, .T. ) ;
#7089 = CARTESIAN_POINT ( 'NONE',  ( -20.48011438624494218, 0.9027161730473580725, -30.00000000000000000 ) ) ;
#7090 = DIRECTION ( 'NONE',  ( -0.2588190451025098593, 0.9659258262890711988, -1.387778780781446292E-17 ) ) ;
#7091 = ORIENTED_EDGE ( 'NONE', *, *, #29703, .T. ) ;
#7092 = CARTESIAN_POINT ( 'NONE',  ( 35.44138113946621615, -9.599287445864765900, -5.442910742026312754 ) ) ;
#7093 = ORIENTED_EDGE ( 'NONE', *, *, #24528, .T. ) ;
#7094 = DIRECTION ( 'NONE',  ( 0.000000000000000000, 0.000000000000000000, 1.000000000000000000 ) ) ;
#7095 = CARTESIAN_POINT ( 'NONE',  ( 3.900486991066101972, 40.17991855518010880, 11.00000000000020250 ) ) ;
#7096 = EDGE_CURVE ( 'NONE', #22335, #28046, #36903, .T. ) ;
#7097 = CARTESIAN_POINT ( 'NONE',  ( -12.82065967939308848, 40.99677499958261961, 11.00000000000000000 ) ) ;
#7098 = CARTESIAN_POINT ( 'NONE',  ( -3.860444543167080855, 8.005107441538555690, 7.455539900862796721 ) ) ;
#7099 = B_SPLINE_CURVE_WITH_KNOTS ( 'NONE', 3,
 ( #29076, #10190, #4087, #16692, #12835, #7329 ),
 .UNSPECIFIED., .F., .F.,
 ( 4, 2, 4 ),
 ( 0.0001748523089235895619, 0.0005603998622486582688, 0.0009459474155737269485 ),
 .UNSPECIFIED. ) ;
#7100 = ADVANCED_FACE ( 'NONE', ( #18815 ), #12315, .T. ) ;
#7101 = CARTESIAN_POINT ( 'NONE',  ( -9.543723562658518844, 28.97375833662206901, 19.66345542862528362 ) ) ;
#7102 = DIRECTION ( 'NONE',  ( -1.000000000000000000, 0.000000000000000000, 0.000000000000000000 ) ) ;
#7103 = EDGE_LOOP ( 'NONE', ( #15945, #38581, #792, #1542 ) ) ;
#7104 = SHAPE_REPRESENTATION_RELATIONSHIP ( 'NONE' , 'NONE' ,  #8618, #23086 ) ;
#7105 = CARTESIAN_POINT ( 'NONE',  ( 3.057012479096308688, 20.28136394534261555, -30.00000000000001066 ) ) ;
#7106 = CARTESIAN_POINT ( 'NONE',  ( 3.503793317224327186, 8.420815634768674229, 11.00000000000000000 ) ) ;
#7107 = FACE_OUTER_BOUND ( 'NONE', #7236, .T. ) ;
#7108 = CARTESIAN_POINT ( 'NONE',  ( 18.14143768169351034, 18.99352574702872687, -5.000000000000003553 ) ) ;
#7109 = CARTESIAN_POINT ( 'NONE',  ( 8.803475244830952562, 27.36709591607177572, -15.90040107698557570 ) ) ;
#7110 = ORIENTED_EDGE ( 'NONE', *, *, #15720, .T. ) ;
#7111 = DIRECTION ( 'NONE',  ( -0.000000000000000000, -0.000000000000000000, -1.000000000000000000 ) ) ;
#7112 = CARTESIAN_POINT ( 'NONE',  ( 12.87862734366817108, -22.00492508238036393, -17.36953957828150763 ) ) ;
#7113 = CARTESIAN_POINT ( 'NONE',  ( -4.441848239913464447, 24.85865334748893929, 20.99999999999999645 ) ) ;
#7114 = CIRCLE ( 'NONE', #20100, 15.00000000000000000 ) ;
#7115 = CARTESIAN_POINT ( 'NONE',  ( -12.30736835487442882, 14.81698729810789672, 11.00000000000000000 ) ) ;
#7116 = ADVANCED_FACE ( 'NONE', ( #31398 ), #3565, .T. ) ;
#7117 = ORIENTED_EDGE ( 'NONE', *, *, #18338, .T. ) ;
#7118 = CARTESIAN_POINT ( 'NONE',  ( -11.31322392688638523, 18.03553487960044777, -25.01503145050758548 ) ) ;
#7119 = CARTESIAN_POINT ( 'NONE',  ( -18.91631044952799812, -27.33967623494412535, 16.30093088680231972 ) ) ;
#7120 = CARTESIAN_POINT ( 'NONE',  ( 14.44676625670391168, -25.74302676979435134, -9.715428041659723846 ) ) ;
#7121 = EDGE_CURVE ( 'NONE', #30787, #36810, #34452, .T. ) ;
#7122 = CARTESIAN_POINT ( 'NONE',  ( -12.19134295108997890, 16.61602540378455117, 10.50000000000000000 ) ) ;
#7123 = ORIENTED_EDGE ( 'NONE', *, *, #33006, .T. ) ;
#7124 = ORIENTED_EDGE ( 'NONE', *, *, #38945, .T. ) ;
#7125 = CARTESIAN_POINT ( 'NONE',  ( -8.515539604177867261, 19.39886015949181441, -25.95454680849416462 ) ) ;
#7126 = DIRECTION ( 'NONE',  ( 0.9135454576426005335, -0.4067366430758010964, 0.000000000000000000 ) ) ;
#7127 = FACE_BOUND ( 'NONE', #36877, .T. ) ;
#7128 = EDGE_CURVE ( 'NONE', #8399, #23608, #32504, .T. ) ;
#7129 = CARTESIAN_POINT ( 'NONE',  ( -35.08557715296313262, -7.694570891656546507, -5.000000000000002665 ) ) ;
#7130 = DIRECTION ( 'NONE',  ( -0.9781476007338041345, 0.2079116908177663370, 0.000000000000000000 ) ) ;
#7131 = ORIENTED_EDGE ( 'NONE', *, *, #14106, .F. ) ;
#7132 = CARTESIAN_POINT ( 'NONE',  ( 20.95308506363175738, 0.9643035589587092282, -26.23839846377317997 ) ) ;
#7133 = CYLINDRICAL_SURFACE ( 'NONE', #6393, 1.000000000000000888 ) ;
#7134 = DIRECTION ( 'NONE',  ( 1.000000000000000000, 0.000000000000000000, 0.000000000000000000 ) ) ;
#7135 = ORIENTED_EDGE ( 'NONE', *, *, #27023, .T. ) ;
#7136 = CARTESIAN_POINT ( 'NONE',  ( -30.19800961909351855, -0.002553536262527825347, -8.766955577734158567 ) ) ;
#7137 = CARTESIAN_POINT ( 'NONE',  ( -5.644276917315534270, 36.40655018617698602, 10.49999999999999822 ) ) ;
#7138 = VERTEX_POINT ( 'NONE', #31200 ) ;
#7139 = CARTESIAN_POINT ( 'NONE',  ( 20.45006009983584860, -1.583034825077791696, -29.30351957104910809 ) ) ;
#7140 = CARTESIAN_POINT ( 'NONE',  ( 20.49802635999024147, 0.7366814822345414404, -30.00000000000001066 ) ) ;
#7141 = CARTESIAN_POINT ( 'NONE',  ( 32.97049335003973169, -4.716631976065183807, 17.42190598798392998 ) ) ;
#7142 = ORIENTED_EDGE ( 'NONE', *, *, #12587, .F. ) ;
#7143 = CARTESIAN_POINT ( 'NONE',  ( -12.27395423108443673, 32.91881889271085981, 16.30093088680193603 ) ) ;
#7144 = EDGE_CURVE ( 'NONE', #12750, #22676, #37297, .T. ) ;
#7145 = VECTOR ( 'NONE', #9265, 1000.000000000000000 ) ;
#7146 = EDGE_CURVE ( 'NONE', #22293, #2500, #36384, .T. ) ;
#7147 = CARTESIAN_POINT ( 'NONE',  ( -20.71630303010418572, -29.20803740758281464, -4.999999999999997335 ) ) ;
#7148 = ADVANCED_FACE ( 'NONE', ( #37500 ), #20016, .T. ) ;
#7149 = CARTESIAN_POINT ( 'NONE',  ( -1.848241319495560253, 27.98666583367183947, 20.99999999999999645 ) ) ;
#7150 = CARTESIAN_POINT ( 'NONE',  ( -13.32679399471724935, 28.40733119287961728, 7.000000000000000000 ) ) ;
#7151 = DIRECTION ( 'NONE',  ( 1.000000000000000000, 0.000000000000000000, 0.000000000000000000 ) ) ;
#7152 = AXIS2_PLACEMENT_3D ( 'NONE', #22889, #35294, #13752 ) ;
#7153 = FACE_BOUND ( 'NONE', #8767, .T. ) ;
#7154 = CARTESIAN_POINT ( 'NONE',  ( 21.00262217607745896, 5.738642561615682425, 19.27171037444140111 ) ) ;
#7155 = AXIS2_PLACEMENT_3D ( 'NONE', #2772, #20675, #2183 ) ;
#7156 = CARTESIAN_POINT ( 'NONE',  ( -22.51939234098515996, 9.738838319951677036, -9.880579217825056659 ) ) ;
#7157 = CARTESIAN_POINT ( 'NONE',  ( 15.50525388175314312, -18.17829242494390130, -21.05556129404982002 ) ) ;
#7158 = CARTESIAN_POINT ( 'NONE',  ( -28.16747440122964008, -24.83813135940263805, -4.999999999999999112 ) ) ;
#7159 = ORIENTED_EDGE ( 'NONE', *, *, #39641, .T. ) ;
#7160 = EDGE_CURVE ( 'NONE', #9720, #37009, #29350, .T. ) ;
#7161 = CARTESIAN_POINT ( 'NONE',  ( 14.47143598563519085, 25.14360450831679117, -11.58605191478856078 ) ) ;
#7162 = VERTEX_POINT ( 'NONE', #16771 ) ;
#7163 = CARTESIAN_POINT ( 'NONE',  ( -13.27773080846810672, 20.14855683102708284, -18.55665866639438022 ) ) ;
#7164 = CARTESIAN_POINT ( 'NONE',  ( -27.10945576260561651, -19.90266412673942398, 19.66345542862529072 ) ) ;
#7165 = EDGE_CURVE ( 'NONE', #33185, #15751, #1350, .T. ) ;
#7166 = CARTESIAN_POINT ( 'NONE',  ( 13.94482798346721353, 26.50521816028912525, 7.000000000000000000 ) ) ;
#7167 = CARTESIAN_POINT ( 'NONE',  ( 15.12875536725216463, 26.04897481050989683, -8.768510653149395040 ) ) ;
#7168 = VERTEX_POINT ( 'NONE', #4570 ) ;
#7169 = CARTESIAN_POINT ( 'NONE',  ( 24.45946707268589293, -13.48901220950923019, -17.59677725036030793 ) ) ;
#7170 = CARTESIAN_POINT ( 'NONE',  ( -12.49038105676665644, 14.13397459621567798, 11.00000000000000000 ) ) ;
#7171 = CIRCLE ( 'NONE', #12375, 1.000000000000000000 ) ;
#7172 = ORIENTED_EDGE ( 'NONE', *, *, #21690, .T. ) ;
#7174 = CARTESIAN_POINT ( 'NONE',  ( 8.070499922308650653, 9.855951069525808350, 7.381627713044574435 ) ) ;
#7173 = CARTESIAN_POINT ( 'NONE',  ( -14.54989670408210500, 25.93872036832522454, -10.61834747045229399 ) ) ;
#7175 = CARTESIAN_POINT ( 'NONE',  ( -15.30846161082977197, -25.59754758358769777, -10.61048781664426599 ) ) ;
#7176 = CARTESIAN_POINT ( 'NONE',  ( -19.48557158514985588, -11.25000000000002309, 6.000000000000000000 ) ) ;
#7177 = VERTEX_POINT ( 'NONE', #922 ) ;
#7178 = CARTESIAN_POINT ( 'NONE',  ( -34.78882160387538391, -14.36995147936751138, -7.130009219520698771 ) ) ;
#7179 = CARTESIAN_POINT ( 'NONE',  ( -14.51760670474123671, -26.47485642095533365, -5.946377559672243684 ) ) ;
#7180 = CARTESIAN_POINT ( 'NONE',  ( 4.440829913680675034, 10.60893893836775348, 13.00000000000000178 ) ) ;
#7181 = CARTESIAN_POINT ( 'NONE',  ( 13.19356601497149839, 17.97120000216638047, -21.82600956427421579 ) ) ;
#7182 = ORIENTED_EDGE ( 'NONE', *, *, #1715, .T. ) ;
#7183 = CARTESIAN_POINT ( 'NONE',  ( 27.98880052845386501, 2.891254499028016234, -7.376140888623180736 ) ) ;
#7184 = FACE_OUTER_BOUND ( 'NONE', #35137, .T. ) ;
#7185 = CARTESIAN_POINT ( 'NONE',  ( 6.404490139165910811, 34.42612703509929872, 10.50000000000000000 ) ) ;
#7186 = ORIENTED_EDGE ( 'NONE', *, *, #20126, .F. ) ;
#7187 = CARTESIAN_POINT ( 'NONE',  ( -27.95296816494704117, -0.09156375941248461048, -13.48332082428012768 ) ) ;
#7188 = CARTESIAN_POINT ( 'NONE',  ( 20.71295742291022890, 0.5317868688435807289, -27.42788539693542305 ) ) ;
#7189 = AXIS2_PLACEMENT_3D ( 'NONE', #31106, #6901, #6504 ) ;
#7190 = CARTESIAN_POINT ( 'NONE',  ( 22.79731396823020262, -22.36677566318291710, 19.66345542862563178 ) ) ;
#7191 = AXIS2_PLACEMENT_3D ( 'NONE', #23201, #29696, #7755 ) ;
#7192 = ORIENTED_EDGE ( 'NONE', *, *, #31263, .T. ) ;
#7193 = CARTESIAN_POINT ( 'NONE',  ( -8.937590682902627037, -20.71651963383551731, -21.24786896499727007 ) ) ;
#7194 = CARTESIAN_POINT ( 'NONE',  ( 13.13581098909226874, 27.45627467658428955, 9.500000000000000000 ) ) ;
#7195 = CARTESIAN_POINT ( 'NONE',  ( -11.78894649379783388, 21.72623886970244911, 6.000000000000000000 ) ) ;
#7196 = AXIS2_PLACEMENT_3D ( 'NONE', #16825, #16622, #31849 ) ;
#7197 = CARTESIAN_POINT ( 'NONE',  ( -7.962467718762158420, 24.71319220551422191, 20.69868183039781329 ) ) ;
#7198 = DIRECTION ( 'NONE',  ( 0.000000000000000000, 0.000000000000000000, 1.000000000000000000 ) ) ;
#7199 = DIRECTION ( 'NONE',  ( 0.000000000000000000, 0.000000000000000000, 1.000000000000000000 ) ) ;
#7200 = CARTESIAN_POINT ( 'NONE',  ( 13.24038105676655341, 15.43301270189216368, 10.63089969389957368 ) ) ;
#7201 = ORIENTED_EDGE ( 'NONE', *, *, #39775, .T. ) ;
#7202 = CARTESIAN_POINT ( 'NONE',  ( -15.21690460405485545, 17.55572914666943873, 13.00000000000000178 ) ) ;
#7203 = FACE_OUTER_BOUND ( 'NONE', #19291, .T. ) ;
#7204 = CARTESIAN_POINT ( 'NONE',  ( 16.36039051805071765, -13.34769688759530482, -26.31117674288608654 ) ) ;
#7205 = DIRECTION ( 'NONE',  ( 0.000000000000000000, 0.000000000000000000, -1.000000000000000000 ) ) ;
#7206 = PLANE ( 'NONE',  #6060 ) ;
#7207 = CARTESIAN_POINT ( 'NONE',  ( 14.77749770927584549, 26.69806964646038239, -9.202908815035055312 ) ) ;
#7208 = LINE ( 'NONE', #10885, #32771 ) ;
#7209 = ORIENTED_EDGE ( 'NONE', *, *, #24311, .T. ) ;
#7210 = VECTOR ( 'NONE', #14415, 1000.000000000000114 ) ;
#7211 = CARTESIAN_POINT ( 'NONE',  ( -15.32646819449677800, 15.98035180726021665, -20.99571673828884144 ) ) ;
#7212 = CARTESIAN_POINT ( 'NONE',  ( 32.33143948541787438, 1.358872982501792226, 11.00000000000000000 ) ) ;
#7213 = AXIS2_PLACEMENT_3D ( 'NONE', #39035, #19544, #32758 ) ;
#7214 = CARTESIAN_POINT ( 'NONE',  ( 15.41329945644580413, -26.72332452139117720, -5.474185070702327849 ) ) ;
#7215 = LINE ( 'NONE', #16578, #37316 ) ;
#7216 = CARTESIAN_POINT ( 'NONE',  ( 11.89771786224719285, 19.37622671090241511, -21.61810800180225911 ) ) ;
#7217 = ORIENTED_EDGE ( 'NONE', *, *, #11891, .F. ) ;
#7218 = CARTESIAN_POINT ( 'NONE',  ( 15.28841811250725868, 26.53669736298195048, -7.357800263959026310 ) ) ;
#7219 = ORIENTED_EDGE ( 'NONE', *, *, #1413, .T. ) ;
#7221 = LINE ( 'NONE', #16991, #29597 ) ;
#7220 = CARTESIAN_POINT ( 'NONE',  ( -15.26742702018640507, 26.60978498224415745, -7.355557875012173952 ) ) ;
#7222 = CARTESIAN_POINT ( 'NONE',  ( -15.45423376311904917, -26.70816042823125613, -5.946215788419346282 ) ) ;
#7223 = CARTESIAN_POINT ( 'NONE',  ( -16.92376161250139788, -28.83147800495276769, 13.32518128616562869 ) ) ;
#7224 = CARTESIAN_POINT ( 'NONE',  ( -22.04784006917977379, -13.31140231594222634, -19.62697991373520878 ) ) ;
#7225 = CARTESIAN_POINT ( 'NONE',  ( -7.052297394767913730, -25.17996142191265463, -4.999999999999999112 ) ) ;
#7226 = CARTESIAN_POINT ( 'NONE',  ( 12.76514706875002858, 19.99879491202248261, -19.56037735346854589 ) ) ;
#7227 = VERTEX_POINT ( 'NONE', #7610 ) ;
#7228 = CARTESIAN_POINT ( 'NONE',  ( 19.37711718808892769, 7.349286276001018692, -26.58382230141096159 ) ) ;
#7229 = CARTESIAN_POINT ( 'NONE',  ( 33.31689420198952689, -19.38461815459663029, -5.000000000000000000 ) ) ;
#7230 = CIRCLE ( 'NONE', #22799, 0.9999999999999997780 ) ;
#7231 = CARTESIAN_POINT ( 'NONE',  ( -13.11868842595538176, -26.17317209596299321, -5.000000000000001776 ) ) ;
#7232 = CARTESIAN_POINT ( 'NONE',  ( -1.553811836244973321, 36.85721162268941242, 17.92354375535250810 ) ) ;
#7233 = ORIENTED_EDGE ( 'NONE', *, *, #13082, .T. ) ;
#7234 = CARTESIAN_POINT ( 'NONE',  ( -31.49989133076260117, -4.076527785121538905, -11.31888596494559529 ) ) ;
#7235 = CARTESIAN_POINT ( 'NONE',  ( -19.05502067201149075, 4.384649331638460268, 20.25080042701565830 ) ) ;
#7236 = EDGE_LOOP ( 'NONE', ( #16542, #15933, #4092, #21485 ) ) ;
#7237 = CARTESIAN_POINT ( 'NONE',  ( 19.84741737732757016, -16.23688957394130838, 20.99999999999999645 ) ) ;
#7238 = CYLINDRICAL_SURFACE ( 'NONE', #37519, 1.000000000000000000 ) ;
#7239 = CARTESIAN_POINT ( 'NONE',  ( 20.85651332716498274, -9.164426480176581791, -23.02215317269795847 ) ) ;
#7240 = CARTESIAN_POINT ( 'NONE',  ( 26.45121176803958107, -27.84758587393105600, 11.55979286843934695 ) ) ;
#7241 = AXIS2_PLACEMENT_3D ( 'NONE', #6065, #34305, #21505 ) ;
#7242 = ADVANCED_FACE ( 'NONE', ( #31795 ), #19491, .T. ) ;
#7243 = ORIENTED_EDGE ( 'NONE', *, *, #17076, .T. ) ;
#7244 = ORIENTED_EDGE ( 'NONE', *, *, #17376, .T. ) ;
#7245 = DIRECTION ( 'NONE',  ( 0.000000000000000000, 0.000000000000000000, 1.000000000000000000 ) ) ;
#7246 = LINE ( 'NONE', #19646, #667 ) ;
#7247 = CARTESIAN_POINT ( 'NONE',  ( 5.494150297854179854, 36.06936027812436407, 10.99999999999999822 ) ) ;
#7248 = VERTEX_POINT ( 'NONE', #16361 ) ;
#7249 = EDGE_CURVE ( 'NONE', #5684, #8671, #39, .T. ) ;
#7250 = CARTESIAN_POINT ( 'NONE',  ( -1.858046560160577565, 36.81141413151663500, -9.283575669460820023 ) ) ;
#7251 = CARTESIAN_POINT ( 'NONE',  ( 12.80736835487433289, 15.68301270189216545, 7.000000000000000000 ) ) ;
#7252 = DIRECTION ( 'NONE',  ( -0.6691306063588670083, -0.7431448254773863615, 0.000000000000000000 ) ) ;
#7253 = EDGE_CURVE ( 'NONE', #24087, #4731, #29244, .T. ) ;
#7254 = CARTESIAN_POINT ( 'NONE',  ( 15.26584437371809955, 27.13525491562438319, 12.00000000000000000 ) ) ;
#7255 = DIRECTION ( 'NONE',  ( 0.000000000000000000, 0.000000000000000000, 1.000000000000000000 ) ) ;
#7256 = DIRECTION ( 'NONE',  ( -1.000000000000000000, 0.000000000000000000, 0.000000000000000000 ) ) ;
#7257 = CARTESIAN_POINT ( 'NONE',  ( 9.856912408380251733, 19.70089498851076470, -23.61131346103714890 ) ) ;
#7258 = CARTESIAN_POINT ( 'NONE',  ( -0.5000000000000004441, 36.00000000000000711, 9.500000000000000000 ) ) ;
#7259 = EDGE_LOOP ( 'NONE', ( #23837, #4853, #25551, #16128 ) ) ;
#7261 = DIRECTION ( 'NONE',  ( -0.3535533905932645160, 0.6123724356957913617, -0.7071067811865550112 ) ) ;
#7260 = CARTESIAN_POINT ( 'NONE',  ( -17.30414937619200799, 11.17673895782788485, -27.73534995255125324 ) ) ;
#7262 = DIRECTION ( 'NONE',  ( 1.000000000000000000, 0.000000000000000000, 0.000000000000000000 ) ) ;
#7263 = CARTESIAN_POINT ( 'NONE',  ( 15.30027160615963844, -26.40643539529997241, -7.826203141063676760 ) ) ;
#7264 = CARTESIAN_POINT ( 'NONE',  ( -5.688306800005769048, 28.52217545723006609, 12.00000000000000000 ) ) ;
#7265 = CARTESIAN_POINT ( 'NONE',  ( 12.11308143205599919, 19.94536299475516472, -20.53731574209467681 ) ) ;
#7266 = CARTESIAN_POINT ( 'NONE',  ( -22.52744239175981278, -0.1803094636421871677, -30.00000000000000000 ) ) ;
#7267 = DIRECTION ( 'NONE',  ( 1.000000000000000000, 0.000000000000000000, 0.000000000000000000 ) ) ;
#7268 = CARTESIAN_POINT ( 'NONE',  ( -21.36603670794792009, -21.34451933144417879, -14.86881065236695143 ) ) ;
#7269 = CIRCLE ( 'NONE', #18342, 1.000000000000000888 ) ;
#7270 = CARTESIAN_POINT ( 'NONE',  ( 8.200574578750897459, -24.73362697332168736, -9.819646422388172979 ) ) ;
#7271 = CARTESIAN_POINT ( 'NONE',  ( 12.74342753841739118, 20.92241134701107441, -18.46772647367177100 ) ) ;
#7272 = CARTESIAN_POINT ( 'NONE',  ( 20.33298947872574658, 13.79308491711421247, -8.897425670759471217 ) ) ;
#7273 = EDGE_CURVE ( 'NONE', #6805, #9357, #18233, .T. ) ;
#7274 = CARTESIAN_POINT ( 'NONE',  ( -8.541476348891238857, 27.59512447410525127, 12.00000000000000000 ) ) ;
#7275 = DIRECTION ( 'NONE',  ( -0.000000000000000000, -0.000000000000000000, -1.000000000000000000 ) ) ;
#7276 = ADVANCED_FACE ( 'NONE', ( #19811 ), #16565, .F. ) ;
#7277 = ORIENTED_EDGE ( 'NONE', *, *, #26619, .F. ) ;
#7278 = CARTESIAN_POINT ( 'NONE',  ( -9.263779654156028442, 34.90887495674188301, -7.602959551972078067 ) ) ;
#7279 = ORIENTED_EDGE ( 'NONE', *, *, #1565, .F. ) ;
#7280 = CARTESIAN_POINT ( 'NONE',  ( 13.36830325120611995, 20.48707633493483371, 7.000000000000000000 ) ) ;
#7281 = ORIENTED_EDGE ( 'NONE', *, *, #30104, .T. ) ;
#7282 = CARTESIAN_POINT ( 'NONE',  ( 26.51902585559564685, 0.2539472759805578295, -15.44871964324930325 ) ) ;
#7283 = LINE ( 'NONE', #29033, #22583 ) ;
#7284 = CYLINDRICAL_SURFACE ( 'NONE', #3117, 6.000000000000000000 ) ;
#7285 = ORIENTED_EDGE ( 'NONE', *, *, #22674, .F. ) ;
#7286 = CARTESIAN_POINT ( 'NONE',  ( -29.45261839425941375, 0.2115709630840172106, -10.18423039480368431 ) ) ;
#7287 = LINE ( 'NONE', #1011, #4040 ) ;
#7288 = VERTEX_POINT ( 'NONE', #32413 ) ;
#7289 = CARTESIAN_POINT ( 'NONE',  ( 28.18850087859003040, -7.572030850641755961, -15.83067351684029589 ) ) ;
#7290 = VECTOR ( 'NONE', #28122, 1000.000000000000227 ) ;
#7291 = EDGE_LOOP ( 'NONE', ( #17897, #11334, #21016, #1165 ) ) ;
#7292 = DIRECTION ( 'NONE',  ( -0.5000000000000041078, 0.8660254037844364872, 0.000000000000000000 ) ) ;
#7293 = CARTESIAN_POINT ( 'NONE',  ( -9.340438144419696442, 38.00965938231844632, 11.55979286843914799 ) ) ;
#7294 = CARTESIAN_POINT ( 'NONE',  ( 4.984135866956516558, 36.15314577889351000, 10.49999999999999822 ) ) ;
#7295 = FACE_OUTER_BOUND ( 'NONE', #39339, .T. ) ;
#7296 = ADVANCED_FACE ( 'NONE', ( #37888 ), #32203, .F. ) ;
#7297 = CARTESIAN_POINT ( 'NONE',  ( 1.248251703783664679, 34.03222469610384593, 19.66345542862528362 ) ) ;
#7298 = DIRECTION ( 'NONE',  ( 1.000000000000000000, 0.000000000000000000, 0.000000000000000000 ) ) ;
#7299 = VERTEX_POINT ( 'NONE', #7202 ) ;
#7300 =( NAMED_UNIT ( * ) SI_UNIT ( $, .STERADIAN. ) SOLID_ANGLE_UNIT ( ) );
#7301 = CARTESIAN_POINT ( 'NONE',  ( -13.45809327831024405, 15.47793591600723850, -30.00000000000001421 ) ) ;
#7302 = DIRECTION ( 'NONE',  ( 0.000000000000000000, 0.000000000000000000, 1.000000000000000000 ) ) ;
#7303 = AXIS2_PLACEMENT_3D ( 'NONE', #18524, #30916, #5811 ) ;
#7304 = DIRECTION ( 'NONE',  ( -1.000000000000000000, 0.000000000000000000, 0.000000000000000000 ) ) ;
#7305 = CARTESIAN_POINT ( 'NONE',  ( 16.84884541703955918, 18.74267451200035950, -12.76513676328720415 ) ) ;
#7306 = CIRCLE ( 'NONE', #14453, 15.00000000000000000 ) ;
#7307 = CARTESIAN_POINT ( 'NONE',  ( 10.90692232337486445, 34.26194292751238635, -5.446513464750788458 ) ) ;
#7308 = ORIENTED_EDGE ( 'NONE', *, *, #33845, .T. ) ;
#7309 = CARTESIAN_POINT ( 'NONE',  ( 10.81260707898150386, 32.90853150812155548, 10.49999999999999822 ) ) ;
#7310 = CARTESIAN_POINT ( 'NONE',  ( -4.481940917958321613, 8.628727325586488917, 7.000000000000000000 ) ) ;
#7311 = VECTOR ( 'NONE', #6699, 1000.000000000000000 ) ;
#7312 = CARTESIAN_POINT ( 'NONE',  ( 10.07140245800056633, -18.11449741766177368, -27.41507013238322088 ) ) ;
#7313 = CARTESIAN_POINT ( 'NONE',  ( 3.833852081710638071, 25.75497152300991033, 21.00000000000000355 ) ) ;
#7314 = CARTESIAN_POINT ( 'NONE',  ( 13.42604558747167687, 21.08886574588663620, 7.000000000000000000 ) ) ;
#7315 = ORIENTED_EDGE ( 'NONE', *, *, #28199, .F. ) ;
#7316 = CARTESIAN_POINT ( 'NONE',  ( -14.03908325169028615, 23.91319235039795643, -13.51416224689532086 ) ) ;
#7317 = AXIS2_PLACEMENT_3D ( 'NONE', #11846, #50, #24829 ) ;
#7318 = CARTESIAN_POINT ( 'NONE',  ( -34.21349446591933940, -17.75307084757253051, 16.30093088680225222 ) ) ;
#7319 = CARTESIAN_POINT ( 'NONE',  ( 10.79644714444348708, -20.53841121863572994, -20.58586955329300139 ) ) ;
#7320 = DIRECTION ( 'NONE',  ( 0.8090169943749426773, -0.5877852522924796874, 0.000000000000000000 ) ) ;
#7321 = EDGE_CURVE ( 'NONE', #36981, #38107, #13810, .T. ) ;
#7322 = EDGE_LOOP ( 'NONE', ( #31173, #33965, #10379 ) ) ;
#7323 = ORIENTED_EDGE ( 'NONE', *, *, #24649, .T. ) ;
#7324 = CARTESIAN_POINT ( 'NONE',  ( -13.29693570674033687, 31.40254479259449383, -5.904557403147712158 ) ) ;
#7325 = CARTESIAN_POINT ( 'NONE',  ( -9.892954722048926897, 20.95745441963943279, 10.49999999999999289 ) ) ;
#7326 = CARTESIAN_POINT ( 'NONE',  ( -8.339609403135950672, 11.87216320208450959, 10.50000000000000000 ) ) ;
#7327 = CARTESIAN_POINT ( 'NONE',  ( -34.97676071130810271, -8.686622228168268123, -7.176601743262130739 ) ) ;
#7328 = CLOSED_SHELL ( 'NONE', ( #19512, #35712, #7860, #18283, #28751, #11651, #1310, #25290, #1079, #15623, #36935, #18090, #13256, #7398, #25434, #31870, #20211, #9544, #25177, #4879, #12888, #15772, #39894, #23536, #33531, #29852, #37914, #15502, #24443, #31344, #22430, #33732, #18357, #11268, #11600, #26388, #30001, #478, #36148, #6161, #19178, #10551, #34248, #28379, #21835, #19847, #32038, #22611, #21751, #26766, #4094, #13648, #5418, #26301, #16496, #37401, #16950, #16511, #13368, #8135, #30419, #9249, #27582, #35968, #801, #31741, #5215, #1076, #36303, #1356, #33494, #10879, #14546, #32951, #31359, #39927, #18457, #37809, #3897, #21256, #10858, #32666, #15987, #5640, #36239, #8876, #1504, #20165, #7296, #13105, #21528, #5687, #17074, #7026, #11290, #34196, #22166, #20157, #25646, #26236, #869, #5116, #223, #21390, #13800, #11134, #5298, #16025, #19956, #39534, #30417, #4320, #39578, #28223, #23407, #2811, #31013, #27140, #12111, #29754, #9750, #11034, #21692, #26493, #28637, #16872, #4802, #1940, #422, #33508, #35487, #7661, #10982, #5671, #5196, #23925, #32650, #11515, #33947, #36202, #37947, #26793, #26249, #19685, #27347, #26024, #39931, #6143, #40052, #29600, #36976, #7276, #35150, #17988, #17775, #32970, #12949, #33900, #31509, #19760, #39190, #24242, #8570, #7540, #18446, #5759, #20587, #15397, #24998, #24564, #3669, #16278, #31390, #28427, #27730, #39681, #3498, #24883, #39326, #27494, #22686, #11616, #34724, #5822, #23094, #20561, #31941, #39430, #14104, #16831, #31441, #27902, #14359 ) ) ;
#7329 = CARTESIAN_POINT ( 'NONE',  ( -13.63396663385394803, 16.24580510161721847, 7.000000000000000000 ) ) ;
#7330 = ORIENTED_EDGE ( 'NONE', *, *, #3846, .F. ) ;
#7331 = CARTESIAN_POINT ( 'NONE',  ( 30.77433313779998159, 0.05499387012786746687, -5.946098457891356936 ) ) ;
#7332 = CARTESIAN_POINT ( 'NONE',  ( 8.694801740383951483, 1.741858881503469902, 11.00000000000000000 ) ) ;
#7333 = DIRECTION ( 'NONE',  ( -0.000000000000000000, -0.000000000000000000, -1.000000000000000000 ) ) ;
#7334 = EDGE_LOOP ( 'NONE', ( #13613, #26262, #9061 ) ) ;
#7335 = CARTESIAN_POINT ( 'NONE',  ( -30.87810876133901061, -0.05119658576620297191, -5.945909103480649271 ) ) ;
#7336 = DIRECTION ( 'NONE',  ( -0.000000000000000000, -0.000000000000000000, -1.000000000000000000 ) ) ;
#7337 = VERTEX_POINT ( 'NONE', #7815 ) ;
#7338 = CARTESIAN_POINT ( 'NONE',  ( 32.07230589051683722, -3.026076898309492336, -9.536960300404496493 ) ) ;
#7339 = VECTOR ( 'NONE', #16676, 1000.000000000000000 ) ;
#7340 = CARTESIAN_POINT ( 'NONE',  ( -8.401171878996500197, 21.11424711454089476, 9.000000000000001776 ) ) ;
#7341 = CARTESIAN_POINT ( 'NONE',  ( 35.11176058605620653, -10.96173827525856481, 16.87380292611440424 ) ) ;
#7342 = ORIENTED_EDGE ( 'NONE', *, *, #38826, .F. ) ;
#7343 = AXIS2_PLACEMENT_3D ( 'NONE', #16254, #4461, #19493 ) ;
#7344 = CARTESIAN_POINT ( 'NONE',  ( -11.06388406389812751, 34.19581601475828592, 16.30093088680271052 ) ) ;
#7345 = CARTESIAN_POINT ( 'NONE',  ( 0.000000000000000000, 0.000000000000000000, -30.00000000000000000 ) ) ;
#7346 = ADVANCED_FACE ( 'NONE', ( #31996 ), #24591, .T. ) ;
#7347 = CARTESIAN_POINT ( 'NONE',  ( -2.594149110900493493, 26.80855565015070852, 20.99999999999998934 ) ) ;
#7348 = CARTESIAN_POINT ( 'NONE',  ( -14.52509594610762456, 21.97885917798744515, 7.500000000000004441 ) ) ;
#7349 = EDGE_CURVE ( 'NONE', #4871, #36787, #4153, .T. ) ;
#7350 = EDGE_CURVE ( 'NONE', #27233, #21190, #2139, .T. ) ;
#7351 = DIRECTION ( 'NONE',  ( 0.000000000000000000, 0.000000000000000000, 1.000000000000000000 ) ) ;
#7352 = EDGE_CURVE ( 'NONE', #37261, #16796, #1937, .T. ) ;
#7353 = FACE_BOUND ( 'NONE', #6366, .T. ) ;
#7354 = AXIS2_PLACEMENT_3D ( 'NONE', #29756, #20621, #1729 ) ;
#7355 = CARTESIAN_POINT ( 'NONE',  ( 23.22986302874564046, 7.287013008514754198, 17.42190598798376300 ) ) ;
#7356 = CARTESIAN_POINT ( 'NONE',  ( -20.20854214045650110, 8.100511891533708209, -21.13395932336453598 ) ) ;
#7357 = CARTESIAN_POINT ( 'NONE',  ( 20.75735356854552904, -27.05917745021801224, -6.795945968575883178 ) ) ;
#7358 = CARTESIAN_POINT ( 'NONE',  ( 4.678013043399745996, 44.50832101651059958, 11.00000000000000000 ) ) ;
#7359 = EDGE_LOOP ( 'NONE', ( #8185, #25832, #31729, #9146, #13532 ) ) ;
#7360 = CARTESIAN_POINT ( 'NONE',  ( 13.11120197629568196, 22.41587477055116295, -16.42154945907974195 ) ) ;
#7361 = CIRCLE ( 'NONE', #22947, 1.000000000000004441 ) ;
#7362 = ORIENTED_EDGE ( 'NONE', *, *, #12790, .T. ) ;
#7363 = CARTESIAN_POINT ( 'NONE',  ( -11.99665585415270996, 16.62659876986841567, -29.36898932499439496 ) ) ;
#7364 = CARTESIAN_POINT ( 'NONE',  ( -28.59012753014036790, -4.062670752122675921, 19.66345542862530493 ) ) ;
#7365 = DIRECTION ( 'NONE',  ( -0.000000000000000000, -0.000000000000000000, -1.000000000000000000 ) ) ;
#7366 = CARTESIAN_POINT ( 'NONE',  ( 15.20579750689515919, 26.17738660362985570, -8.298505875400808307 ) ) ;
#7367 = ORIENTED_EDGE ( 'NONE', *, *, #27650, .F. ) ;
#7368 = CARTESIAN_POINT ( 'NONE',  ( 18.30700033879082866, -10.10138274711125916, -26.96693921537031358 ) ) ;
#7369 = CARTESIAN_POINT ( 'NONE',  ( -14.09933648065464240, 26.02968990214173317, 10.49999999999999822 ) ) ;
#7370 = VERTEX_POINT ( 'NONE', #29760 ) ;
#7372 = FACE_OUTER_BOUND ( 'NONE', #9429, .T. ) ;
#7371 = CARTESIAN_POINT ( 'NONE',  ( -15.26147044535763619, 27.21892886845185089, -5.941221209073404452 ) ) ;
#7373 = ADVANCED_FACE ( 'NONE', ( #32818 ), #1734, .T. ) ;
#7374 = CARTESIAN_POINT ( 'NONE',  ( -10.36434502333254315, -19.11546864033186566, -23.83618939619293542 ) ) ;
#7375 = CARTESIAN_POINT ( 'NONE',  ( 13.87104230352200140, 20.53934056656866147, 7.500000000000010658 ) ) ;
#7376 = ADVANCED_FACE ( 'NONE', ( #14112 ), #26137, .T. ) ;
#7377 = VECTOR ( 'NONE', #12951, 1000.000000000000000 ) ;
#7378 = ORIENTED_EDGE ( 'NONE', *, *, #5247, .T. ) ;
#7379 = CARTESIAN_POINT ( 'NONE',  ( -34.44723686885956226, -13.00661877071162209, -8.430185889806901756 ) ) ;
#7380 = CARTESIAN_POINT ( 'NONE',  ( -13.46329895589916426, -25.24432993333344655, -10.67838853379888420 ) ) ;
#7381 = DIRECTION ( 'NONE',  ( 0.000000000000000000, 0.000000000000000000, 1.000000000000000000 ) ) ;
#7382 = CARTESIAN_POINT ( 'NONE',  ( 13.21519265033025370, 15.68751749194264811, -29.39041693340186256 ) ) ;
#7383 = ORIENTED_EDGE ( 'NONE', *, *, #24165, .F. ) ;
#7384 = CARTESIAN_POINT ( 'NONE',  ( 28.17783618559230163, 2.888000139098982455, -5.949579471811276221 ) ) ;
#7385 = DIRECTION ( 'NONE',  ( 1.000000000000000000, 0.000000000000000000, 0.000000000000000000 ) ) ;
#7386 = CARTESIAN_POINT ( 'NONE',  ( 11.54666566735224364, 32.07468077621332725, 7.000000000000000000 ) ) ;
#7387 = ORIENTED_EDGE ( 'NONE', *, *, #27749, .F. ) ;
#7388 = CARTESIAN_POINT ( 'NONE',  ( -29.98028507518004915, -0.1513904216296562966, -9.695762027821260176 ) ) ;
#7389 = CARTESIAN_POINT ( 'NONE',  ( 31.12761295898370406, -0.5681698218874843276, -7.338521178719154214 ) ) ;
#7390 = CIRCLE ( 'NONE', #28826, 0.5000000000000003331 ) ;
#7391 = CARTESIAN_POINT ( 'NONE',  ( 28.07442828530308176, -16.20877872786445195, 20.25080042701566541 ) ) ;
#7392 = VERTEX_POINT ( 'NONE', #21018 ) ;
#7393 = CARTESIAN_POINT ( 'NONE',  ( -16.24796006241077961, 15.88921519459651499, -30.00000000000001421 ) ) ;
#7394 = ADVANCED_FACE ( 'NONE', ( #17977 ), #2767, .T. ) ;
#7395 = AXIS2_PLACEMENT_3D ( 'NONE', #34651, #12710, #31012 ) ;
#7396 = DIRECTION ( 'NONE',  ( -0.6724985119639504960, -0.2185080122244063561, 0.7071067811865553443 ) ) ;
#7397 = DIRECTION ( 'NONE',  ( -0.3090169943749589976, -0.9510565162951498674, 0.000000000000000000 ) ) ;
#7398 = ADVANCED_FACE ( 'NONE', ( #26909 ), #14920, .F. ) ;
#7399 = DIRECTION ( 'NONE',  ( -0.7431448254773862505, 0.6691306063588671194, 0.000000000000000000 ) ) ;
#7400 = VECTOR ( 'NONE', #10305, 1000.000000000000000 ) ;
#7401 = EDGE_CURVE ( 'NONE', #26220, #21421, #25459, .T. ) ;
#7402 = CYLINDRICAL_SURFACE ( 'NONE', #37640, 57.99999999999995737 ) ;
#7403 = CYLINDRICAL_SURFACE ( 'NONE', #33346, 5.999999999999994671 ) ;
#7404 = CARTESIAN_POINT ( 'NONE',  ( 12.03640989728592459, 29.14264673470096767, 6.000000000000000000 ) ) ;
#7405 = EDGE_LOOP ( 'NONE', ( #12610, #13437, #14609 ) ) ;
#7406 = CARTESIAN_POINT ( 'NONE',  ( -6.856644039074812014, 35.52575270032661336, 10.49999999999999822 ) ) ;
#7407 = FACE_OUTER_BOUND ( 'NONE', #36891, .T. ) ;
#7408 = CARTESIAN_POINT ( 'NONE',  ( 28.16003781345056112, -24.46727846297508790, -6.718121626700479077 ) ) ;
#7409 = DIRECTION ( 'NONE',  ( -0.9135454576426004225, 0.4067366430758009854, 0.000000000000000000 ) ) ;
#7410 = CARTESIAN_POINT ( 'NONE',  ( 11.11016527260166420, 31.83082137946473367, 9.500000000000000000 ) ) ;
#7411 = CARTESIAN_POINT ( 'NONE',  ( 11.17633995497393151, 19.38694057465163922, -22.64794263314978906 ) ) ;
#7412 = ORIENTED_EDGE ( 'NONE', *, *, #34849, .T. ) ;
#7413 = CARTESIAN_POINT ( 'NONE',  ( -14.43025776552523709, 14.57938852240508965, -29.40747009719811444 ) ) ;
#7414 = CARTESIAN_POINT ( 'NONE',  ( 1.000000000000000000, 37.00000000000000711, 9.500000000000000000 ) ) ;
#7415 = CARTESIAN_POINT ( 'NONE',  ( 15.14062276522389361, -26.27454551934281213, -8.297974524426454224 ) ) ;
#7416 = CARTESIAN_POINT ( 'NONE',  ( 8.843266739736581172, 16.81698729810774395, 11.00000000000000000 ) ) ;
#7417 = CARTESIAN_POINT ( 'NONE',  ( 15.24290316429634373, 26.37011248965962551, -7.827967277537388746 ) ) ;
#7418 = EDGE_LOOP ( 'NONE', ( #1240, #40007 ) ) ;
#7419 = CARTESIAN_POINT ( 'NONE',  ( 14.02760127444125438, 23.93997290703913805, -13.51284491737120064 ) ) ;
#7420 = B_SPLINE_SURFACE_WITH_KNOTS ( 'NONE', 1, 3, ( 
 ( #14966, #32868, #1989, #34257, #2974, #524, #12512, #3760, #9863, #19007 ),
 ( #24504, #9675, #9072, #31007, #12906, #37695, #18419, #34056, #15962, #21457 ) ),
 .UNSPECIFIED., .F., .F., .F.,
 ( 2, 2 ),
 ( 4, 2, 2, 2, 4 ),
 ( 0.000000000000000000, 1.000000000000000000 ),
 ( 1.644979861859638293, 2.037678943558364875, 2.430378025257091235, 2.823077106955818039, 3.215776188654544399 ),
 .UNSPECIFIED. ) ;
#7421 = ORIENTED_EDGE ( 'NONE', *, *, #26501, .T. ) ;
#7423 = CARTESIAN_POINT ( 'NONE',  ( 14.42035624161478324, 26.65972665747659676, 10.49999999999999822 ) ) ;
#7422 = CARTESIAN_POINT ( 'NONE',  ( -15.33535238615493235, 26.80152092193110391, -6.415128186030386814 ) ) ;
#7424 = CARTESIAN_POINT ( 'NONE',  ( -15.07294390951978791, -26.14423714609062799, -8.768195475925240956 ) ) ;
#7425 = CARTESIAN_POINT ( 'NONE',  ( -14.98890121934590347, -28.67928442654175214, 11.55979286843934872 ) ) ;
#7426 = EDGE_CURVE ( 'NONE', #24952, #36412, #20294, .T. ) ;
#7427 = CIRCLE ( 'NONE', #12622, 1.000000000000000000 ) ;
#7428 = CARTESIAN_POINT ( 'NONE',  ( -28.05941199598445834, -18.14228187561381134, -12.89353790789255783 ) ) ;
#7429 = CARTESIAN_POINT ( 'NONE',  ( -4.809173904559163937, -24.92317228705597287, -4.999999999999999112 ) ) ;
#7430 = CARTESIAN_POINT ( 'NONE',  ( 15.89036220987575376, 24.93293676434921835, -6.419745934221619876 ) ) ;
#7431 = ORIENTED_EDGE ( 'NONE', *, *, #25689, .T. ) ;
#7432 = CARTESIAN_POINT ( 'NONE',  ( 23.38135512150587658, 9.224932765178692762, -5.964625366264517226 ) ) ;
#7433 = CARTESIAN_POINT ( 'NONE',  ( -4.984135866956331817, 36.15314577889358105, 11.00000000000000000 ) ) ;
#7434 = CARTESIAN_POINT ( 'NONE',  ( -12.67417846324130259, 14.47720745114830443, 7.499999999999993783 ) ) ;
#7435 = CARTESIAN_POINT ( 'NONE',  ( -6.320269494896706419, 36.18253918181394369, 17.42190598798392287 ) ) ;
#7436 = COLOUR_RGB ( '', 0.40784314, 0.44705882, 0.49803922) ;
#7437 = B_SPLINE_CURVE_WITH_KNOTS ( 'NONE', 3,
 ( #32670, #33277, #4825, #29607, #5429, #38953 ),
 .UNSPECIFIED., .F., .F.,
 ( 4, 2, 4 ),
 ( 0.000000000000000000, 0.5000000000000000000, 1.000000000000000000 ),
 .UNSPECIFIED. ) ;
#7438 = ORIENTED_EDGE ( 'NONE', *, *, #11994, .T. ) ;
#7439 = CARTESIAN_POINT ( 'NONE',  ( -20.43418187165424982, -1.772479648697218302, -30.00000000000000000 ) ) ;
#7440 = VECTOR ( 'NONE', #35756, 1000.000000000000000 ) ;
#7441 = CARTESIAN_POINT ( 'NONE',  ( -24.79273775960036019, -6.040746354373381699, 20.82122704794079837 ) ) ;
#7442 = ORIENTED_EDGE ( 'NONE', *, *, #8372, .T. ) ;
#7443 = DIRECTION ( 'NONE',  ( -1.000000000000000000, 0.000000000000000000, 0.000000000000000000 ) ) ;
#7444 = CARTESIAN_POINT ( 'NONE',  ( -14.31603901957233660, 19.98981538725089990, 10.49999999999999467 ) ) ;
#7445 = DIRECTION ( 'NONE',  ( -0.000000000000000000, -0.000000000000000000, -1.000000000000000000 ) ) ;
#7446 = CARTESIAN_POINT ( 'NONE',  ( 18.98852328848152382, -8.348878395094288862, -27.72209281211808118 ) ) ;
#7447 = CARTESIAN_POINT ( 'NONE',  ( 14.98890121934557307, -28.67928442654207188, 11.55979286843934872 ) ) ;
#7448 = EDGE_CURVE ( 'NONE', #16860, #31812, #38901, .T. ) ;
#7449 = ORIENTED_EDGE ( 'NONE', *, *, #6052, .T. ) ;
#7450 = FACE_OUTER_BOUND ( 'NONE', #37234, .T. ) ;
#7451 = FACE_OUTER_BOUND ( 'NONE', #8880, .T. ) ;
#7452 = CIRCLE ( 'NONE', #36676, 61.99999999999998579 ) ;
#7453 = CARTESIAN_POINT ( 'NONE',  ( 1.590043107810628076, 12.61456814725305442, 10.49999999999999467 ) ) ;
#7454 = ORIENTED_EDGE ( 'NONE', *, *, #35332, .T. ) ;
#7455 = CARTESIAN_POINT ( 'NONE',  ( -1.635714998051162938, 32.39290691969485891, -13.80806220344194024 ) ) ;
#7456 = LINE ( 'NONE', #33669, #25616 ) ;
#7457 = CYLINDRICAL_SURFACE ( 'NONE', #11149, 61.99999999999997868 ) ;
#7458 = CONICAL_SURFACE ( 'NONE', #13318, 1.000000000000004441, 0.7853981633974517207 ) ;
#7459 = LINE ( 'NONE', #32257, #23428 ) ;
#7460 = LINE ( 'NONE', #11125, #30109 ) ;
#7461 = FACE_OUTER_BOUND ( 'NONE', #34326, .T. ) ;
#7462 = CARTESIAN_POINT ( 'NONE',  ( 9.616349836912345239, 18.28445365398381028, -27.99377830595204841 ) ) ;
#7464 = AXIS2_PLACEMENT_3D ( 'NONE', #35097, #26753, #1174 ) ;
#7463 = CARTESIAN_POINT ( 'NONE',  ( 32.35383858704737037, -1.519079388893764149, -4.999999999999999112 ) ) ;
#7465 = ORIENTED_EDGE ( 'NONE', *, *, #31511, .F. ) ;
#7468 = PLANE ( 'NONE',  #14843 ) ;
#7467 = VECTOR ( 'NONE', #29728, 1000.000000000000000 ) ;
#7466 = CARTESIAN_POINT ( 'NONE',  ( -17.92042771800729639, 12.70853344890674386, -20.10281234600826394 ) ) ;
#7469 = CARTESIAN_POINT ( 'NONE',  ( -13.48130249190472973, 27.93180293473202980, 10.49999999999999822 ) ) ;
#7470 = CARTESIAN_POINT ( 'NONE',  ( 15.53190721697598242, -26.72795937246275599, -5.945400711064137589 ) ) ;
#7471 = PLANE ( 'NONE',  #38605 ) ;
#7472 = CARTESIAN_POINT ( 'NONE',  ( 10.96965864260556600, 17.37149835738324910, -28.70543893499321086 ) ) ;
#7473 = CARTESIAN_POINT ( 'NONE',  ( -6.155076441694329326, 21.71698211341365337, -20.11584339644705111 ) ) ;
#7474 = CARTESIAN_POINT ( 'NONE',  ( -20.39213822642799201, -16.19729952584802035, 22.99999999999999645 ) ) ;
#7475 = CARTESIAN_POINT ( 'NONE',  ( -15.56847894655029485, -14.60930148832306763, -25.70159151419933252 ) ) ;
#7476 = CARTESIAN_POINT ( 'NONE',  ( 7.481479378253174772, -23.30152825933829774, -14.77492706919554522 ) ) ;
#7477 = CARTESIAN_POINT ( 'NONE',  ( 13.87218762615114542, 23.17697767821096377, -14.48925779226203758 ) ) ;
#7478 = CARTESIAN_POINT ( 'NONE',  ( 20.57095190365273396, 13.97674357447790250, -5.482604214182108748 ) ) ;
#7479 = EDGE_CURVE ( 'NONE', #488, #12698, #36657, .T. ) ;
#7480 = DIRECTION ( 'NONE',  ( 1.000000000000000000, 1.224646799147351235E-16, -0.000000000000000000 ) ) ;
#7481 = CARTESIAN_POINT ( 'NONE',  ( -5.330077540933487512, 17.71145523154927659, 12.00000000000000000 ) ) ;
#7482 = EDGE_CURVE ( 'NONE', #10104, #24743, #35859, .T. ) ;
#7483 = EDGE_LOOP ( 'NONE', ( #14879, #33556, #36634, #2764 ) ) ;
#7484 = CARTESIAN_POINT ( 'NONE',  ( -9.379895652603979173, 35.46246444712465973, -5.443039496959672263 ) ) ;
#7485 = ORIENTED_EDGE ( 'NONE', *, *, #996, .T. ) ;
#7486 = CARTESIAN_POINT ( 'NONE',  ( -14.21183036229989938, -25.04515749559450555, -11.60314391679283297 ) ) ;
#7487 = CARTESIAN_POINT ( 'NONE',  ( 15.00000000000000000, 22.50000000000000711, 0.000000000000000000 ) ) ;
#7488 = VERTEX_POINT ( 'NONE', #11675 ) ;
#7489 = CARTESIAN_POINT ( 'NONE',  ( 20.48245044547724447, 0.8483310608570673317, -30.00000000000000000 ) ) ;
#7490 = CARTESIAN_POINT ( 'NONE',  ( -14.36830325120615548, 20.48707633493503621, 9.500000000000000000 ) ) ;
#7491 = DIRECTION ( 'NONE',  ( 1.000000000000000000, -3.469446951953611033E-15, 0.000000000000000000 ) ) ;
#7492 = EDGE_CURVE ( 'NONE', #30242, #37387, #21212, .T. ) ;
#7493 = ORIENTED_EDGE ( 'NONE', *, *, #29461, .T. ) ;
#7494 = CARTESIAN_POINT ( 'NONE',  ( -20.48011438624494218, 0.9027161730473576284, -29.34916148302687589 ) ) ;
#7495 = ORIENTED_EDGE ( 'NONE', *, *, #31835, .T. ) ;
#7496 = CARTESIAN_POINT ( 'NONE',  ( 20.09314088254942021, -4.111701498484372053, -29.26211593337953687 ) ) ;
#7497 = CIRCLE ( 'NONE', #34738, 0.5000000000000004441 ) ;
#7498 = VECTOR ( 'NONE', #5343, 1000.000000000000000 ) ;
#7499 = EDGE_LOOP ( 'NONE', ( #25020, #12541, #12407, #11804 ) ) ;
#7500 = DIRECTION ( 'NONE',  ( 1.000000000000000000, 0.000000000000000000, 0.000000000000000000 ) ) ;
#7501 = CARTESIAN_POINT ( 'NONE',  ( 16.82090372984156801, 29.19711159930561450, 11.55979286843845877 ) ) ;
#7502 = DIRECTION ( 'NONE',  ( 1.000000000000000000, 0.000000000000000000, 0.000000000000000000 ) ) ;
#7503 = CARTESIAN_POINT ( 'NONE',  ( -10.81260707898136708, 32.90853150812170469, 11.00000000000000000 ) ) ;
#7504 = CARTESIAN_POINT ( 'NONE',  ( -12.55429062395159079, 25.98950339719647218, 18.87996532025784546 ) ) ;
#7505 = DIRECTION ( 'NONE',  ( -1.000000000000000000, 0.000000000000000000, 0.000000000000000000 ) ) ;
#7506 = ORIENTED_EDGE ( 'NONE', *, *, #34223, .F. ) ;
#7507 = CARTESIAN_POINT ( 'NONE',  ( -8.315274455032216849, 10.01576150750520888, 7.000000000000000000 ) ) ;
#7508 = DIRECTION ( 'NONE',  ( 1.000000000000000000, 0.000000000000000000, 0.000000000000000000 ) ) ;
#7509 = EDGE_CURVE ( 'NONE', #29377, #32505, #16492, .T. ) ;
#7510 = DIRECTION ( 'NONE',  ( 0.9510565162951504226, -0.3090169943749573322, -0.000000000000000000 ) ) ;
#7511 = CARTESIAN_POINT ( 'NONE',  ( 18.24376955283985424, 17.51282272560135667, -9.848228921199581265 ) ) ;
#7512 = CARTESIAN_POINT ( 'NONE',  ( 7.361316653671116761, 22.88337532404381491, -20.99261860353674436 ) ) ;
#7513 = ORIENTED_EDGE ( 'NONE', *, *, #6012, .F. ) ;
#7514 = CARTESIAN_POINT ( 'NONE',  ( 13.01837422881150452, 21.26636931122159169, 12.00000000000000000 ) ) ;
#7515 = DIRECTION ( 'NONE',  ( 0.1045284632676566766, 0.9945218953682730678, 0.000000000000000000 ) ) ;
#7516 = CARTESIAN_POINT ( 'NONE',  ( 10.29754018676950622, -18.14354158297081909, -26.77788074137142615 ) ) ;
#7517 = CARTESIAN_POINT ( 'NONE',  ( -4.672335726382761401, 24.36080358023105674, 20.99999999999999645 ) ) ;
#7518 = VECTOR ( 'NONE', #20338, 1000.000000000000114 ) ;
#7519 = CARTESIAN_POINT ( 'NONE',  ( -14.86556419889029357, 20.43481210330121556, 10.63089969389957545 ) ) ;
#7520 = ORIENTED_EDGE ( 'NONE', *, *, #4933, .T. ) ;
#7521 = CIRCLE ( 'NONE', #8166, 0.5000000000000002220 ) ;
#7522 = CARTESIAN_POINT ( 'NONE',  ( -11.70184164389253745, 18.89639632332092845, -22.73775843682962261 ) ) ;
#7523 = AXIS2_PLACEMENT_3D ( 'NONE', #26770, #29820, #23525 ) ;
#7524 = CARTESIAN_POINT ( 'NONE',  ( -22.37155630812419105, -27.08896561536066372, 16.30093088680148838 ) ) ;
#7525 = CARTESIAN_POINT ( 'NONE',  ( 14.50550552640858015, -26.01656545232359363, -8.773312412628245127 ) ) ;
#7526 = VECTOR ( 'NONE', #36516, 999.9999999999998863 ) ;
#7527 = ADVANCED_FACE ( 'NONE', ( #20625 ), #23860, .T. ) ;
#7528 = CARTESIAN_POINT ( 'NONE',  ( -9.892954722048921568, 20.95745441963943279, 10.50000000000000000 ) ) ;
#7529 = ORIENTED_EDGE ( 'NONE', *, *, #32131, .T. ) ;
#7530 = ORIENTED_EDGE ( 'NONE', *, *, #14496, .T. ) ;
#7531 = CARTESIAN_POINT ( 'NONE',  ( -13.26798563164391354, 31.32064769528049197, -6.352507814907438544 ) ) ;
#7532 = CARTESIAN_POINT ( 'NONE',  ( -15.52303001916276592, -20.83641102679212764, -18.06021460390243405 ) ) ;
#7533 = EDGE_CURVE ( 'NONE', #25736, #8130, #17582, .T. ) ;
#7534 = DIRECTION ( 'NONE',  ( 0.000000000000000000, 0.000000000000000000, 1.000000000000000000 ) ) ;
#7535 = CARTESIAN_POINT ( 'NONE',  ( -22.66259745418890859, -5.598351139313090030, -22.08065378927834388 ) ) ;
#7536 = CARTESIAN_POINT ( 'NONE',  ( -4.940908595777639967, 35.94977745735568675, 9.500000000000000000 ) ) ;
#7537 = ORIENTED_EDGE ( 'NONE', *, *, #25894, .T. ) ;
#7538 = CARTESIAN_POINT ( 'NONE',  ( 22.69409974816363729, 0.7326708127613092980, -21.63252463746919929 ) ) ;
#7539 = EDGE_CURVE ( 'NONE', #13411, #17829, #39296, .T. ) ;
#7540 = ADVANCED_FACE ( 'NONE', ( #8427 ), #3319, .F. ) ;
#7541 = DIRECTION ( 'NONE',  ( 1.000000000000000000, 0.000000000000000000, 0.000000000000000000 ) ) ;
#7542 = DIRECTION ( 'NONE',  ( 1.000000000000000000, 0.000000000000000000, 0.000000000000000000 ) ) ;
#7543 = EDGE_CURVE ( 'NONE', #24016, #22931, #15117, .T. ) ;
#7544 = EDGE_LOOP ( 'NONE', ( #38628, #27785, #36390, #16649, #8851 ) ) ;
#7545 = CARTESIAN_POINT ( 'NONE',  ( -29.82034722167092156, 0.02361265341038061225, -9.708167889285391539 ) ) ;
#7546 = DIRECTION ( 'NONE',  ( 0.000000000000000000, -0.000000000000000000, -1.000000000000000000 ) ) ;
#7547 = ORIENTED_EDGE ( 'NONE', *, *, #28007, .F. ) ;
#7548 = CARTESIAN_POINT ( 'NONE',  ( 33.36633864933632054, -3.217268494394103229, -5.458641031229113594 ) ) ;
#7549 = CARTESIAN_POINT ( 'NONE',  ( 17.25552743462859695, 11.08949724875112608, -29.99999999999998934 ) ) ;
#7550 = CARTESIAN_POINT ( 'NONE',  ( 35.45120626212618475, -5.541700984529022378, 15.13084544680181587 ) ) ;
#7551 = ORIENTED_EDGE ( 'NONE', *, *, #37220, .F. ) ;
#7552 = CARTESIAN_POINT ( 'NONE',  ( -9.684793793942127138, 35.24386573278048473, 16.30093088680190760 ) ) ;
#7553 = CARTESIAN_POINT ( 'NONE',  ( 10.60610353952458773, -24.43405348869776006, 17.42190598798185164 ) ) ;
#7554 = CARTESIAN_POINT ( 'NONE',  ( 14.36830325120613239, 20.48707633493482660, 11.00000000000000000 ) ) ;
#7555 = CARTESIAN_POINT ( 'NONE',  ( 3.998720052559921356, 27.76176938167571961, 20.94377226548378346 ) ) ;
#7556 = AXIS2_PLACEMENT_3D ( 'NONE', #35268, #23071, #32432 ) ;
#7557 = DIRECTION ( 'NONE',  ( 0.000000000000000000, 0.000000000000000000, 1.000000000000000000 ) ) ;
#7558 = CIRCLE ( 'NONE', #30279, 15.99999999999999645 ) ;
#7559 = EDGE_CURVE ( 'NONE', #24946, #8057, #28715, .T. ) ;
#7560 = DIRECTION ( 'NONE',  ( -0.2876062384759434654, 0.6459741880212587217, -0.7071067811865433539 ) ) ;
#7561 = EDGE_CURVE ( 'NONE', #12323, #35381, #22005, .T. ) ;
#7562 = CARTESIAN_POINT ( 'NONE',  ( 5.706335727061685681, 24.35410196624994583, 6.000000000000000000 ) ) ;
#7563 = CARTESIAN_POINT ( 'NONE',  ( 14.43694901004736586, 26.51279404189499900, 17.42190598798392998 ) ) ;
#7564 = CARTESIAN_POINT ( 'NONE',  ( -22.44844293511189193, 8.669737220969816249, -12.85907312109028133 ) ) ;
#7565 = CARTESIAN_POINT ( 'NONE',  ( 20.90254793926122900, -27.22588555765620555, -5.000000000000008882 ) ) ;
#7566 = DIRECTION ( 'NONE',  ( -0.7431448254773862505, 0.6691306063588672304, 0.000000000000000000 ) ) ;
#7567 = VERTEX_POINT ( 'NONE', #21803 ) ;
#7568 = CARTESIAN_POINT ( 'NONE',  ( 11.59239201401879171, 19.00133579775832615, -22.71882842871296404 ) ) ;
#7569 = EDGE_LOOP ( 'NONE', ( #816, #3331, #39784, #16057 ) ) ;
#7570 = CARTESIAN_POINT ( 'NONE',  ( -12.37225743350618146, 18.24419790101515204, -22.84300898652141854 ) ) ;
#7571 = CARTESIAN_POINT ( 'NONE',  ( -24.71109915376977284, -20.69862126830784277, 19.99202127657074612 ) ) ;
#7572 = CYLINDRICAL_SURFACE ( 'NONE', #12054, 1.000000000000000888 ) ;
#7573 = CARTESIAN_POINT ( 'NONE',  ( 13.52849422955318914, 22.74332991843149543, -15.45577255175012787 ) ) ;
#7574 = VERTEX_POINT ( 'NONE', #27506 ) ;
#7575 = CARTESIAN_POINT ( 'NONE',  ( 28.41128743669290557, -15.66287405488943740, -13.80598174040671466 ) ) ;
#7576 = DIRECTION ( 'NONE',  ( 0.000000000000000000, 0.000000000000000000, 1.000000000000000000 ) ) ;
#7577 = ORIENTED_EDGE ( 'NONE', *, *, #24739, .T. ) ;
#7579 = DIRECTION ( 'NONE',  ( -1.000000000000000000, 0.000000000000000000, 0.000000000000000000 ) ) ;
#7578 = CARTESIAN_POINT ( 'NONE',  ( -10.81707015764707691, 17.67222468787956302, -27.42788574818700553 ) ) ;
#7580 = CARTESIAN_POINT ( 'NONE',  ( -16.31051618889534893, -26.39850790843190254, -8.716711649698549280 ) ) ;
#7581 = ADVANCED_FACE ( 'NONE', ( #12066 ), #37050, .T. ) ;
#7582 = CARTESIAN_POINT ( 'NONE',  ( 12.34742388243071964, 14.79386122849051155, 11.00000000000000000 ) ) ;
#7583 = AXIS2_PLACEMENT_3D ( 'NONE', #4031, #23126, #13378 ) ;
#7584 = ORIENTED_EDGE ( 'NONE', *, *, #16442, .F. ) ;
#7585 = CARTESIAN_POINT ( 'NONE',  ( -34.18333301601428786, -12.90150185328116628, -8.870171403992342718 ) ) ;
#7586 = CARTESIAN_POINT ( 'NONE',  ( -14.75944605622549943, -26.27728134964919349, -7.830481699696290931 ) ) ;
#7587 = CYLINDRICAL_SURFACE ( 'NONE', #38419, 0.5000000000000004441 ) ;
#7588 = CARTESIAN_POINT ( 'NONE',  ( 15.94977354568814754, 20.60013326908762465, -12.70067996356593021 ) ) ;
#7589 = ORIENTED_EDGE ( 'NONE', *, *, #23139, .T. ) ;
#7590 = CARTESIAN_POINT ( 'NONE',  ( 24.80460892327041833, 3.756148522752393859, -14.69522679569688250 ) ) ;
#7591 = DIRECTION ( 'NONE',  ( -0.2079116908177663092, -0.9781476007338042455, 0.000000000000000000 ) ) ;
#7592 = CARTESIAN_POINT ( 'NONE',  ( -36.53988293555860878, -0.5802930328944716498, 22.99999999999905853 ) ) ;
#7593 = VERTEX_POINT ( 'NONE', #28098 ) ;
#7594 = CARTESIAN_POINT ( 'NONE',  ( -22.78220600028421927, 0.4401612305667206293, -21.59410079891940626 ) ) ;
#7595 = CARTESIAN_POINT ( 'NONE',  ( 29.97538051898516187, -0.6571090628178190007, -10.59662107009966547 ) ) ;
#7596 = AXIS2_PLACEMENT_3D ( 'NONE', #20269, #29606, #27162 ) ;
#7597 = CARTESIAN_POINT ( 'NONE',  ( 23.22759628179494484, -23.81077309377013762, 18.87996532025824337 ) ) ;
#7598 = EDGE_LOOP ( 'NONE', ( #10632, #18395, #19344, #39125 ) ) ;
#7599 = CARTESIAN_POINT ( 'NONE',  ( -22.77989339854785200, 2.034344915145157806, -20.71315197334980951 ) ) ;
#7600 = CARTESIAN_POINT ( 'NONE',  ( -6.023418944065157987, 39.81932404830322270, -4.999999999999988454 ) ) ;
#7601 = CARTESIAN_POINT ( 'NONE',  ( -14.57486473880221745, 26.18419839932921533, 10.50000000000000000 ) ) ;
#7602 = DIRECTION ( 'NONE',  ( -0.1045284632676570929, -0.9945218953682730678, 0.000000000000000000 ) ) ;
#7603 = EDGE_CURVE ( 'NONE', #7885, #25412, #15313, .T. ) ;
#7604 = AXIS2_PLACEMENT_3D ( 'NONE', #11658, #24040, #8601 ) ;
#7605 = AXIS2_PLACEMENT_3D ( 'NONE', #998, #19675, #25767 ) ;
#7606 = LINE ( 'NONE', #39090, #38943 ) ;
#7607 = CARTESIAN_POINT ( 'NONE',  ( 19.48557158514975285, -11.24999999999995737, 6.000000000000000000 ) ) ;
#7608 = LINE ( 'NONE', #22640, #21136 ) ;
#7609 = EDGE_LOOP ( 'NONE', ( #16733, #3805 ) ) ;
#7610 = CARTESIAN_POINT ( 'NONE',  ( 1.981960960816328887, 14.62372257652092422, 12.00000000000000000 ) ) ;
#7611 = DIRECTION ( 'NONE',  ( 0.000000000000000000, 0.000000000000000000, 1.000000000000000000 ) ) ;
#7612 = CARTESIAN_POINT ( 'NONE',  ( 25.68472818303882121, -23.76469768826056850, -10.23310688448228944 ) ) ;
#7613 = VECTOR ( 'NONE', #36894, 1000.000000000000000 ) ;
#7614 = DIRECTION ( 'NONE',  ( -0.000000000000000000, -0.000000000000000000, -1.000000000000000000 ) ) ;
#7615 = CARTESIAN_POINT ( 'NONE',  ( -11.07315816304227774, 31.12468366354675808, 9.500000000000000000 ) ) ;
#7616 = CARTESIAN_POINT ( 'NONE',  ( 14.49073764824685639, 26.09592138030880903, -10.60856989523508354 ) ) ;
#7617 = VECTOR ( 'NONE', #32443, 1000.000000000000000 ) ;
#7618 = DIRECTION ( 'NONE',  ( 0.000000000000000000, 0.000000000000000000, 1.000000000000000000 ) ) ;
#7619 = EDGE_LOOP ( 'NONE', ( #2923, #38133, #16100, #37772 ) ) ;
#7620 = CARTESIAN_POINT ( 'NONE',  ( -17.10053421514107086, 20.30440721539819648, -9.319735994576449301 ) ) ;
#7621 = CARTESIAN_POINT ( 'NONE',  ( 22.73075399258359397, -29.06185307675098883, 10.99999999999956124 ) ) ;
#7622 = CARTESIAN_POINT ( 'NONE',  ( 15.37571132048090838, -26.71368809714059722, -5.000000000000000888 ) ) ;
#7623 = DIRECTION ( 'NONE',  ( 1.000000000000000000, 0.000000000000000000, 0.000000000000000000 ) ) ;
#7624 = CARTESIAN_POINT ( 'NONE',  ( 12.66461257586694522, 21.03697436711803093, -18.45420929576124180 ) ) ;
#7625 = ORIENTED_EDGE ( 'NONE', *, *, #33229, .F. ) ;
#7626 = CARTESIAN_POINT ( 'NONE',  ( 14.02442048416569875, 23.94739483851058992, -13.51247984510621691 ) ) ;
#7627 = VERTEX_POINT ( 'NONE', #24455 ) ;
#7629 = DIRECTION ( 'NONE',  ( 1.000000000000000000, 0.000000000000000000, 0.000000000000000000 ) ) ;
#7628 = CARTESIAN_POINT ( 'NONE',  ( -14.25168967311887336, 24.57581336903061597, -12.54168332028313770 ) ) ;
#7630 = CARTESIAN_POINT ( 'NONE',  ( -9.962624055743289020, -18.81531389238340424, -25.01503139869100067 ) ) ;
#7631 = EDGE_CURVE ( 'NONE', #31950, #26852, #15519, .T. ) ;
#7632 = CARTESIAN_POINT ( 'NONE',  ( -22.71963042674493138, -29.00054972838716338, 12.14047268033060156 ) ) ;
#7633 = CARTESIAN_POINT ( 'NONE',  ( -24.40043856705758429, -15.76608764628647386, -16.63189293991312923 ) ) ;
#7634 = CARTESIAN_POINT ( 'NONE',  ( -5.781254241314485398, -22.30500674272131079, -17.88517324897596339 ) ) ;
#7635 = CARTESIAN_POINT ( 'NONE',  ( 13.51725026480668213, 20.71157673340521654, -17.53186203222074724 ) ) ;
#7637 = EDGE_CURVE ( 'NONE', #7051, #32832, #11216, .T. ) ;
#7636 = VERTEX_POINT ( 'NONE', #277 ) ;
#7638 = CARTESIAN_POINT ( 'NONE',  ( 18.90684236932249362, 8.006108384110648402, -28.85488273963430572 ) ) ;
#7639 = CARTESIAN_POINT ( 'NONE',  ( 21.52603227935954777, -27.16584173104201483, -4.999999999999999112 ) ) ;
#7640 = DIRECTION ( 'NONE',  ( 0.000000000000000000, 0.000000000000000000, 1.000000000000000000 ) ) ;
#7641 = CARTESIAN_POINT ( 'NONE',  ( 6.577540944421576441, 33.15743037285414374, 13.00000000000000178 ) ) ;
#7642 = AXIS2_PLACEMENT_3D ( 'NONE', #14384, #26771, #39161 ) ;
#7643 = VERTEX_POINT ( 'NONE', #39889 ) ;
#7644 = CARTESIAN_POINT ( 'NONE',  ( -27.39143991665605427, -1.197730116296394920, -15.28568366619224506 ) ) ;
#7645 = VECTOR ( 'NONE', #11996, 1000.000000000000000 ) ;
#7646 = CIRCLE ( 'NONE', #20008, 1.000000000000000000 ) ;
#7647 = EDGE_CURVE ( 'NONE', #14056, #33800, #29391, .T. ) ;
#7648 = CARTESIAN_POINT ( 'NONE',  ( -9.555312204555107769, 25.15592819202021246, 20.25080042701566541 ) ) ;
#7649 = ORIENTED_EDGE ( 'NONE', *, *, #7637, .T. ) ;
#7650 = CARTESIAN_POINT ( 'NONE',  ( 24.49409870379991716, -11.70597971641857526, 20.99999999999999645 ) ) ;
#7651 = CARTESIAN_POINT ( 'NONE',  ( 11.11016527260166420, 31.83082137946473367, 7.000000000000000000 ) ) ;
#7652 = VECTOR ( 'NONE', #38988, 1000.000000000000000 ) ;
#7653 = CARTESIAN_POINT ( 'NONE',  ( -4.440836655099179353, 34.39106106163288246, 12.00000000000000000 ) ) ;
#7654 = CARTESIAN_POINT ( 'NONE',  ( 19.01366704504291150, -7.688495684904651739, -29.22164179442962606 ) ) ;
#7656 = AXIS2_PLACEMENT_3D ( 'NONE', #31480, #21730, #37581 ) ;
#7655 = CARTESIAN_POINT ( 'NONE',  ( 36.53369576860747259, -5.154516326609281052, 11.55979286843935760 ) ) ;
#7657 = ORIENTED_EDGE ( 'NONE', *, *, #36728, .T. ) ;
#7658 = DIRECTION ( 'NONE',  ( -1.000000000000000000, 0.000000000000000000, 0.000000000000000000 ) ) ;
#7659 = CARTESIAN_POINT ( 'NONE',  ( -5.440836655099179353, 34.39106106163288246, 6.000000000000000000 ) ) ;
#7660 = ADVANCED_FACE ( 'NONE', ( #3518 ), #36852, .T. ) ;
#7661 = ADVANCED_FACE ( 'NONE', ( #6358 ), #6555, .F. ) ;
#7662 = DIRECTION ( 'NONE',  ( -1.000000000000000000, -1.224646799147353947E-16, 0.000000000000000000 ) ) ;
#7663 = VERTEX_POINT ( 'NONE', #9024 ) ;
#7664 = CARTESIAN_POINT ( 'NONE',  ( -0.6617914413177042876, 33.48614826591853699, -12.88875466627582611 ) ) ;
#7665 = DIRECTION ( 'NONE',  ( -0.000000000000000000, -0.000000000000000000, -1.000000000000000000 ) ) ;
#7666 = CARTESIAN_POINT ( 'NONE',  ( 14.11133924723984379, 27.61078317377175750, 10.49999999999999822 ) ) ;
#7667 = DIRECTION ( 'NONE',  ( 0.000000000000000000, 0.000000000000000000, 1.000000000000000000 ) ) ;
#7668 = DIRECTION ( 'NONE',  ( 0.000000000000000000, 0.000000000000000000, 1.000000000000000000 ) ) ;
#7669 = DIRECTION ( 'NONE',  ( 1.000000000000000000, 0.000000000000000000, 0.000000000000000000 ) ) ;
#7670 = VECTOR ( 'NONE', #14151, 1000.000000000000114 ) ;
#7671 = CARTESIAN_POINT ( 'NONE',  ( 12.77361610477846021, 26.39586754454798623, -13.30043833072773118 ) ) ;
#7672 = DIRECTION ( 'NONE',  ( -0.000000000000000000, -0.000000000000000000, -1.000000000000000000 ) ) ;
#7673 = AXIS2_PLACEMENT_3D ( 'NONE', #7794, #3738, #31974 ) ;
#7674 = ORIENTED_EDGE ( 'NONE', *, *, #28279, .F. ) ;
#7676 = CARTESIAN_POINT ( 'NONE',  ( 7.577540944421576441, 33.15743037285414374, 12.00000000000000000 ) ) ;
#7675 = CARTESIAN_POINT ( 'NONE',  ( -17.80721512534418594, 11.54891248224037703, -23.32888160359681606 ) ) ;
#7677 = FACE_OUTER_BOUND ( 'NONE', #14358, .T. ) ;
#7678 = CARTESIAN_POINT ( 'NONE',  ( 14.78531380799004857, -25.66241841546151647, -10.17861963493258592 ) ) ;
#7679 = FACE_OUTER_BOUND ( 'NONE', #22830, .T. ) ;
#7680 = CARTESIAN_POINT ( 'NONE',  ( 14.27327873935064240, 24.51847890865961332, -12.54657257531869163 ) ) ;
#7681 = VECTOR ( 'NONE', #5858, 1000.000000000000000 ) ;
#7682 = CARTESIAN_POINT ( 'NONE',  ( -15.29245034862078256, 32.56469986091995850, -13.99876745781543441 ) ) ;
#7683 = CARTESIAN_POINT ( 'NONE',  ( -10.77091082532341204, 29.60251629318183575, 6.000000000000000000 ) ) ;
#7684 = EDGE_CURVE ( 'NONE', #36577, #34387, #77, .T. ) ;
#7685 = CONICAL_SURFACE ( 'NONE', #20011, 1.000000000000000444, 0.7853981633974482790 ) ;
#7686 = CARTESIAN_POINT ( 'NONE',  ( -15.00563708114499839, -14.08213718363703038, -28.49568921477004579 ) ) ;
#7687 = CARTESIAN_POINT ( 'NONE',  ( 7.295766330847792247, -19.78656087607541281, -25.27750885764057287 ) ) ;
#7688 = CARTESIAN_POINT ( 'NONE',  ( 13.07663108452908673, 21.41433421891530742, -17.46206790837113232 ) ) ;
#7689 = EDGE_CURVE ( 'NONE', #39696, #20607, #21589, .T. ) ;
#7690 = CARTESIAN_POINT ( 'NONE',  ( 21.09554553119179587, 13.00325820389446640, -5.483046721296032544 ) ) ;
#7691 = LINE ( 'NONE', #29226, #18615 ) ;
#7692 = EDGE_LOOP ( 'NONE', ( #7946, #983, #9218, #6840 ) ) ;
#7693 = CARTESIAN_POINT ( 'NONE',  ( -6.113050074066779693, 35.28635442325187199, -9.759865422729246731 ) ) ;
#7694 = ORIENTED_EDGE ( 'NONE', *, *, #38411, .T. ) ;
#7695 = CARTESIAN_POINT ( 'NONE',  ( 2.525645716490518833, 8.212903943950921715, 7.000000000000000000 ) ) ;
#7696 = ORIENTED_EDGE ( 'NONE', *, *, #35695, .F. ) ;
#7697 = CARTESIAN_POINT ( 'NONE',  ( -2.835137251120299684, 29.44922644035488446, 6.000000000000000000 ) ) ;
#7698 = CARTESIAN_POINT ( 'NONE',  ( -8.195318570657255108, 10.36946087849385378, 11.00000000000000000 ) ) ;
#7699 = ORIENTED_EDGE ( 'NONE', *, *, #33414, .T. ) ;
#7700 = CARTESIAN_POINT ( 'NONE',  ( -28.80451674142937435, 0.2040911148255387941, -11.60275554337247250 ) ) ;
#7701 = VERTEX_POINT ( 'NONE', #9625 ) ;
#7702 = CARTESIAN_POINT ( 'NONE',  ( 30.88881066025174249, -7.339856315056953129, -13.03470611699965254 ) ) ;
#7703 = AXIS2_PLACEMENT_3D ( 'NONE', #13373, #17040, #1596 ) ;
#7704 = AXIS2_PLACEMENT_3D ( 'NONE', #11733, #18035, #23520 ) ;
#7705 = VERTEX_POINT ( 'NONE', #24854 ) ;
#7706 = DIRECTION ( 'NONE',  ( -0.5000000000000041078, 0.8660254037844364872, 0.000000000000000000 ) ) ;
#7707 = CARTESIAN_POINT ( 'NONE',  ( -3.900486991066871578, 40.17991855517983879, 11.00000000000019007 ) ) ;
#7708 = AXIS2_PLACEMENT_3D ( 'NONE', #21598, #16106, #28490 ) ;
#7709 = CARTESIAN_POINT ( 'NONE',  ( -5.034171952701850472, 35.03623199971307400, 9.500000000000000000 ) ) ;
#7710 = DIRECTION ( 'NONE',  ( -0.9510565162951503115, 0.3090169943749573878, -0.000000000000000000 ) ) ;
#7711 = CARTESIAN_POINT ( 'NONE',  ( 10.52848948537593721, 31.43736604633500065, 18.42518152272110044 ) ) ;
#7712 = CARTESIAN_POINT ( 'NONE',  ( -11.61633080063096379, 31.93537370176186840, 10.49999999999999467 ) ) ;
#7713 = VERTEX_POINT ( 'NONE', #18766 ) ;
#7714 = CARTESIAN_POINT ( 'NONE',  ( -11.48173768534023154, 32.16538668264431777, 11.00000000000000000 ) ) ;
#7715 = DIRECTION ( 'NONE',  ( 0.000000000000000000, 0.000000000000000000, 1.000000000000000000 ) ) ;
#7716 = EDGE_CURVE ( 'NONE', #4829, #12491, #37250, .T. ) ;
#7717 = DIRECTION ( 'NONE',  ( -0.000000000000000000, -0.000000000000000000, -1.000000000000000000 ) ) ;
#7718 = CARTESIAN_POINT ( 'NONE',  ( 18.46013033000776105, 17.79035490549923892, -7.894551517905889604 ) ) ;
#7719 = CARTESIAN_POINT ( 'NONE',  ( 11.71220820147315500, 33.45731985618542836, -4.999999999999999112 ) ) ;
#7720 = VERTEX_POINT ( 'NONE', #31349 ) ;
#7721 = DIRECTION ( 'NONE',  ( 1.000000000000000000, 0.000000000000000000, 0.000000000000000000 ) ) ;
#7722 = DIRECTION ( 'NONE',  ( 0.000000000000000000, 0.000000000000000000, 1.000000000000000000 ) ) ;
#7723 = CARTESIAN_POINT ( 'NONE',  ( 14.59862030170441294, -25.11507782388870069, -11.58181169016334700 ) ) ;
#7724 = FACE_OUTER_BOUND ( 'NONE', #6567, .T. ) ;
#7725 = DIRECTION ( 'NONE',  ( -0.000000000000000000, -0.000000000000000000, -1.000000000000000000 ) ) ;
#7726 = VECTOR ( 'NONE', #6807, 1000.000000000000000 ) ;
#7727 = ORIENTED_EDGE ( 'NONE', *, *, #9833, .T. ) ;
#7728 = CARTESIAN_POINT ( 'NONE',  ( -14.83546796608161067, 25.62370260551899648, -10.17934226487036398 ) ) ;
#7729 = CARTESIAN_POINT ( 'NONE',  ( -15.37000524125038048, -27.20210912714571805, 15.72805884748939498 ) ) ;
#7730 = CARTESIAN_POINT ( 'NONE',  ( 14.65009913602293246, -26.04841806957208306, -8.771861423863645868 ) ) ;
#7731 = CARTESIAN_POINT ( 'NONE',  ( -7.530592408761010326, 11.28437794979203268, 9.500000000000000000 ) ) ;
#7732 = ORIENTED_EDGE ( 'NONE', *, *, #20844, .T. ) ;
#7733 = ORIENTED_EDGE ( 'NONE', *, *, #33684, .F. ) ;
#7734 = AXIS2_PLACEMENT_3D ( 'NONE', #22948, #22540, #3862 ) ;
#7735 = CARTESIAN_POINT ( 'NONE',  ( -13.23903555654749020, 31.23875059796648301, -6.800458226667165818 ) ) ;
#7736 = FACE_OUTER_BOUND ( 'NONE', #32776, .T. ) ;
#7737 = FACE_BOUND ( 'NONE', #6607, .T. ) ;
#7738 = CARTESIAN_POINT ( 'NONE',  ( -33.89543892622803156, -8.375972393599855792, -9.375676559666750620 ) ) ;
#7739 = DIRECTION ( 'NONE',  ( 0.000000000000000000, 0.000000000000000000, 1.000000000000000000 ) ) ;
#7740 = ORIENTED_EDGE ( 'NONE', *, *, #21958, .T. ) ;
#7741 = CARTESIAN_POINT ( 'NONE',  ( 20.68287806670252849, 0.9940655047353081919, -27.45775483230204728 ) ) ;
#7742 = CARTESIAN_POINT ( 'NONE',  ( -10.61811999842798038, 32.73341455422775681, 10.94387467463492847 ) ) ;
#7743 = CARTESIAN_POINT ( 'NONE',  ( -14.63635198741550347, 25.78286467897752487, 7.000000000000000000 ) ) ;
#7744 = DIRECTION ( 'NONE',  ( -0.000000000000000000, -0.000000000000000000, -1.000000000000000000 ) ) ;
#7745 = ORIENTED_EDGE ( 'NONE', *, *, #39800, .T. ) ;
#7746 = CARTESIAN_POINT ( 'NONE',  ( -30.90411674721317326, -0.04211297212934855816, -5.474206011825583751 ) ) ;
#7747 = DIRECTION ( 'NONE',  ( -0.4999999999999920064, 0.8660254037844432595, 0.000000000000000000 ) ) ;
#7748 = VERTEX_POINT ( 'NONE', #38202 ) ;
#7749 = CARTESIAN_POINT ( 'NONE',  ( 31.26306821908464428, -2.125275754412755624, -10.04085527566182634 ) ) ;
#7750 = CARTESIAN_POINT ( 'NONE',  ( 18.28409177823415277, 9.297167255826021659, -29.99999999999998934 ) ) ;
#7751 = CARTESIAN_POINT ( 'NONE',  ( 20.72701401736302529, -28.35932241216985972, 14.53008259254010959 ) ) ;
#7752 = ORIENTED_EDGE ( 'NONE', *, *, #2916, .F. ) ;
#7753 = CARTESIAN_POINT ( 'NONE',  ( 15.75274587708552154, 28.77197995862663760, 15.13084544680308063 ) ) ;
#7754 = CARTESIAN_POINT ( 'NONE',  ( -16.23042486172771248, -23.86708630543029130, 18.87996532025784902 ) ) ;
#7755 = DIRECTION ( 'NONE',  ( -1.000000000000000000, 0.000000000000000000, 0.000000000000000000 ) ) ;
#7756 = CARTESIAN_POINT ( 'NONE',  ( 0.8051564177163211822, 29.93655406406124797, 20.82122704794079837 ) ) ;
#7757 = VECTOR ( 'NONE', #5175, 1000.000000000000000 ) ;
#7758 = DIRECTION ( 'NONE',  ( -0.000000000000000000, -0.000000000000000000, -1.000000000000000000 ) ) ;
#7759 = VERTEX_POINT ( 'NONE', #2726 ) ;
#7760 = EDGE_CURVE ( 'NONE', #28177, #35442, #7306, .T. ) ;
#7761 = CARTESIAN_POINT ( 'NONE',  ( 14.47283171447379146, 21.48159823030311344, 11.00000000000000000 ) ) ;
#7762 = AXIS2_PLACEMENT_3D ( 'NONE', #32043, #13753, #22692 ) ;
#7763 = CARTESIAN_POINT ( 'NONE',  ( 5.000626697282971378, 37.74343557191168941, -4.999999999999998224 ) ) ;
#7764 = DIRECTION ( 'NONE',  ( -1.000000000000000000, 0.000000000000000000, 0.000000000000000000 ) ) ;
#7765 = ADVANCED_FACE ( 'NONE', ( #26609 ), #38467, .T. ) ;
#7766 = CARTESIAN_POINT ( 'NONE',  ( 31.72789954390927392, 0.7664678198816438082, 14.53008259254011136 ) ) ;
#7767 = ADVANCED_FACE ( 'NONE', ( #38399 ), #17725, .T. ) ;
#7768 = CARTESIAN_POINT ( 'NONE',  ( 17.86928906486870616, -20.91001877870844439, -16.92124633107672338 ) ) ;
#7769 = CARTESIAN_POINT ( 'NONE',  ( -75.15099915297791711, 43.38844959084113384, 0.000000000000000000 ) ) ;
#7770 = CARTESIAN_POINT ( 'NONE',  ( -35.48538791413474769, -11.24999995268676933, -5.000000000000001776 ) ) ;
#7771 = DIRECTION ( 'NONE',  ( 1.000000000000000000, 0.000000000000000000, 0.000000000000000000 ) ) ;
#7772 = EDGE_LOOP ( 'NONE', ( #30220, #7431, #10147, #1607 ) ) ;
#7773 = CARTESIAN_POINT ( 'NONE',  ( 12.58653840504220156, 21.15301265646719742, -18.43749620103639586 ) ) ;
#7774 = ORIENTED_EDGE ( 'NONE', *, *, #35230, .F. ) ;
#7775 = CARTESIAN_POINT ( 'NONE',  ( -11.60488116879842835, 17.80579030430908816, -25.05364671859870640 ) ) ;
#7776 = CARTESIAN_POINT ( 'NONE',  ( -29.36302367423271065, -15.61102309902027585, 19.99202127657132877 ) ) ;
#7777 = CARTESIAN_POINT ( 'NONE',  ( -14.42035624161472640, 26.65972665747679216, 10.49999999999999822 ) ) ;
#7778 = CARTESIAN_POINT ( 'NONE',  ( 15.45734228612143646, 26.63525802094401840, -5.000000000000000000 ) ) ;
#7779 = EDGE_LOOP ( 'NONE', ( #38746, #29521, #5886, #8980 ) ) ;
#7780 = CARTESIAN_POINT ( 'NONE',  ( 21.14049327140447687, -10.84634200327551312, -21.84289514537541166 ) ) ;
#7781 = ORIENTED_EDGE ( 'NONE', *, *, #683, .F. ) ;
#7783 = CARTESIAN_POINT ( 'NONE',  ( 13.63581098909226519, 27.45627467658428600, 11.00000000000000000 ) ) ;
#7782 = CARTESIAN_POINT ( 'NONE',  ( -15.18956287470529709, 27.28009750321776039, -6.407581706259474430 ) ) ;
#7784 = CARTESIAN_POINT ( 'NONE',  ( -13.64508740925339758, -22.56256837047442687, -16.33802543730708123 ) ) ;
#7785 = FACE_OUTER_BOUND ( 'NONE', #19336, .T. ) ;
#7786 = VECTOR ( 'NONE', #35156, 1000.000000000000000 ) ;
#7787 = VERTEX_POINT ( 'NONE', #4270 ) ;
#7788 = CARTESIAN_POINT ( 'NONE',  ( -35.01063367814790439, -14.47062566131834416, -6.283729949479822885 ) ) ;
#7789 = CARTESIAN_POINT ( 'NONE',  ( -12.26719960628313899, -22.55384718030699176, -16.47309707856247485 ) ) ;
#7790 = CARTESIAN_POINT ( 'NONE',  ( 35.72300736400854504, -23.12593624637943179, 22.99999999999999289 ) ) ;
#7791 = CARTESIAN_POINT ( 'NONE',  ( 17.28126569830730475, 21.10767333569910065, -5.476227410499634018 ) ) ;
#7792 = VERTEX_POINT ( 'NONE', #26208 ) ;
#7793 = CARTESIAN_POINT ( 'NONE',  ( 27.14291608416113988, 3.777963889476882109, -7.862006169886337048 ) ) ;
#7794 = CARTESIAN_POINT ( 'NONE',  ( 19.48557158514988075, -11.24999999999998224, 0.000000000000000000 ) ) ;
#7795 = EDGE_CURVE ( 'NONE', #8150, #26803, #22883, .T. ) ;
#7796 = CARTESIAN_POINT ( 'NONE',  ( -11.87435565298220830, 15.06698729810789139, 9.500000000000000000 ) ) ;
#7797 = ADVANCED_FACE ( 'NONE', ( #10574 ), #10774, .T. ) ;
#7798 = AXIS2_PLACEMENT_3D ( 'NONE', #22841, #3754, #31791 ) ;
#7799 = VERTEX_POINT ( 'NONE', #23161 ) ;
#7800 = CARTESIAN_POINT ( 'NONE',  ( -25.96849961500957349, 0.1468702090680218675, -16.42151745127020135 ) ) ;
#7801 = CARTESIAN_POINT ( 'NONE',  ( 20.49250884496040115, 0.5553618484168653113, -30.00000000000000355 ) ) ;
#7802 = CARTESIAN_POINT ( 'NONE',  ( 17.59613548593226540, -24.21943298483269302, 18.87996532025752217 ) ) ;
#7803 = VERTEX_POINT ( 'NONE', #39003 ) ;
#7804 = CARTESIAN_POINT ( 'NONE',  ( -20.63698148512490604, 1.517229800946207297, -27.48967112051710160 ) ) ;
#7805 = CARTESIAN_POINT ( 'NONE',  ( 3.091399026088761826, 22.35909668862748489, -30.00000000000000711 ) ) ;
#7806 = DIRECTION ( 'NONE',  ( 1.000000000000000000, 0.000000000000000000, 0.000000000000000000 ) ) ;
#7807 = AXIS2_PLACEMENT_3D ( 'NONE', #35347, #37989, #16867 ) ;
#7808 = DIRECTION ( 'NONE',  ( -1.000000000000000000, 0.000000000000000000, 0.000000000000000000 ) ) ;
#7809 = EDGE_CURVE ( 'NONE', #12521, #17600, #5080, .T. ) ;
#7810 = CYLINDRICAL_SURFACE ( 'NONE', #15599, 1.000000000000000000 ) ;
#7811 = DIRECTION ( 'NONE',  ( -0.1045284632676437842, 0.9945218953682744001, 0.000000000000000000 ) ) ;
#7812 = CARTESIAN_POINT ( 'NONE',  ( 1.100969307443724343, 12.51061230184417816, 10.49999999999999467 ) ) ;
#7813 = ORIENTED_EDGE ( 'NONE', *, *, #8412, .T. ) ;
#7814 = CARTESIAN_POINT ( 'NONE',  ( -23.14161831312300066, 5.133065578429416576, -16.80419845731963946 ) ) ;
#7815 = CARTESIAN_POINT ( 'NONE',  ( -8.541476348891238857, 27.59512447410525127, 13.00000000000000178 ) ) ;
#7816 = DIRECTION ( 'NONE',  ( 0.000000000000000000, 0.000000000000000000, 1.000000000000000000 ) ) ;
#7817 = CARTESIAN_POINT ( 'NONE',  ( 18.61921750058829517, -17.17969631063009928, -19.77528146303147949 ) ) ;
#7818 = CARTESIAN_POINT ( 'NONE',  ( 1.485571585149812135, -11.25000000000009415, 3.000000000000000000 ) ) ;
#7819 = CARTESIAN_POINT ( 'NONE',  ( -14.60528968261104055, 20.46216805729389066, 10.94387467463490360 ) ) ;
#7820 = CARTESIAN_POINT ( 'NONE',  ( 14.68255685887305795, 26.08100846820239838, -10.15216213446657356 ) ) ;
#7821 = ORIENTED_EDGE ( 'NONE', *, *, #35727, .F. ) ;
#7822 = CARTESIAN_POINT ( 'NONE',  ( -17.16552075097585117, 20.40790064679622873, -8.835065107039243415 ) ) ;
#7823 = DIRECTION ( 'NONE',  ( -0.9510565162951544194, -0.3090169943749450643, 0.000000000000000000 ) ) ;
#7824 = CARTESIAN_POINT ( 'NONE',  ( 11.11074582133875843, -20.48182189777266160, -20.55012700056129660 ) ) ;
#7825 = CARTESIAN_POINT ( 'NONE',  ( 4.706335727061685681, 24.35410196624994583, 6.000000000000000000 ) ) ;
#7826 = CARTESIAN_POINT ( 'NONE',  ( 14.54328903961689790, 24.94079327997583917, -11.59986628730510105 ) ) ;
#7827 = ORIENTED_EDGE ( 'NONE', *, *, #11316, .T. ) ;
#7828 = CARTESIAN_POINT ( 'NONE',  ( 11.47176157324268786, 18.44815111932139118, -23.85198228110581908 ) ) ;
#7829 = ORIENTED_EDGE ( 'NONE', *, *, #20021, .F. ) ;
#7831 = DIRECTION ( 'NONE',  ( 1.000000000000000000, 0.000000000000000000, 0.000000000000000000 ) ) ;
#7830 = CARTESIAN_POINT ( 'NONE',  ( -15.25818811814006715, 26.64143884112164073, -7.354687272877148629 ) ) ;
#7832 = CARTESIAN_POINT ( 'NONE',  ( -14.74254311150509622, -25.65307385468569734, -10.18114048116609460 ) ) ;
#7833 = CARTESIAN_POINT ( 'NONE',  ( -32.33143948541798096, 1.358872982501892590, 11.00000000000000000 ) ) ;
#7834 = CARTESIAN_POINT ( 'NONE',  ( -31.94951466207645296, -20.64243727267584561, -7.119159330032495347 ) ) ;
#7835 = CARTESIAN_POINT ( 'NONE',  ( -9.079790354755763460, -25.03302911735815073, -8.836781494452289110 ) ) ;
#7836 = CARTESIAN_POINT ( 'NONE',  ( 15.81916445039664687, 24.79389647095221250, -7.365108267298476008 ) ) ;
#7837 = ORIENTED_EDGE ( 'NONE', *, *, #37876, .F. ) ;
#7838 = CARTESIAN_POINT ( 'NONE',  ( 20.75988934644436767, 7.624137786315204224, -20.05700069588757728 ) ) ;
#7839 = VECTOR ( 'NONE', #13705, 1000.000000000000000 ) ;
#7840 = DIRECTION ( 'NONE',  ( 0.000000000000000000, 0.000000000000000000, 1.000000000000000000 ) ) ;
#7841 = DIRECTION ( 'NONE',  ( 1.000000000000000000, 0.000000000000000000, 0.000000000000000000 ) ) ;
#7842 = EDGE_CURVE ( 'NONE', #33096, #33201, #15789, .T. ) ;
#7843 = DIRECTION ( 'NONE',  ( 0.000000000000000000, 0.000000000000000000, 1.000000000000000000 ) ) ;
#7844 = ORIENTED_EDGE ( 'NONE', *, *, #19715, .T. ) ;
#7845 = CARTESIAN_POINT ( 'NONE',  ( -31.44789842147330106, -2.359368921698832722, -10.02552052183717635 ) ) ;
#7846 = CARTESIAN_POINT ( 'NONE',  ( -15.48226359616454495, 8.938689054909644938, 20.50957957746029336 ) ) ;
#7847 = CARTESIAN_POINT ( 'NONE',  ( 25.43307211745627328, -8.368469763667489403, 20.94377226548379411 ) ) ;
#7848 = DIRECTION ( 'NONE',  ( 0.9876883405951395467, 0.1564344650402197390, 0.000000000000000000 ) ) ;
#7849 = AXIS2_PLACEMENT_3D ( 'NONE', #36156, #39793, #17880 ) ;
#7850 = CARTESIAN_POINT ( 'NONE',  ( -3.485571585149855434, -11.25000000000002132, 6.000000000000000000 ) ) ;
#7851 = CARTESIAN_POINT ( 'NONE',  ( 24.20165044650383734, -11.49403616741239809, -18.62786580867516051 ) ) ;
#7852 = CARTESIAN_POINT ( 'NONE',  ( 22.73075399258386398, -29.06185307675093199, 10.99999999999955769 ) ) ;
#7853 = EDGE_LOOP ( 'NONE', ( #885, #1750, #30592, #3439 ) ) ;
#7854 = CYLINDRICAL_SURFACE ( 'NONE', #35316, 1.000000000000000000 ) ;
#7855 = DIRECTION ( 'NONE',  ( 1.000000000000000000, 0.000000000000000000, 0.000000000000000000 ) ) ;
#7856 = EDGE_CURVE ( 'NONE', #17014, #18163, #15579, .T. ) ;
#7857 = CIRCLE ( 'NONE', #7189, 1.000000000000000888 ) ;
#7858 = CARTESIAN_POINT ( 'NONE',  ( 6.451376067921989588, 35.76073122305122354, 10.94387467463335639 ) ) ;
#7859 = ORIENTED_EDGE ( 'NONE', *, *, #25017, .T. ) ;
#7860 = ADVANCED_FACE ( 'NONE', ( #19919 ), #17486, .F. ) ;
#7861 = CARTESIAN_POINT ( 'NONE',  ( 0.2867187372796554667, 26.83502801510120506, -18.61248171148112363 ) ) ;
#7862 = DIRECTION ( 'NONE',  ( 1.000000000000000000, 0.000000000000000000, 0.000000000000000000 ) ) ;
#7863 = CARTESIAN_POINT ( 'NONE',  ( 14.06009009443824986, 27.59413131461127833, 10.76099332938163577 ) ) ;
#7864 = FACE_OUTER_BOUND ( 'NONE', #9694, .T. ) ;
#7865 = DIRECTION ( 'NONE',  ( 1.000000000000000000, 0.000000000000000000, 0.000000000000000000 ) ) ;
#7866 = LINE ( 'NONE', #22901, #8008 ) ;
#7867 = CARTESIAN_POINT ( 'NONE',  ( 9.427076569009681606, 18.67421965452293620, -26.67537954699011848 ) ) ;
#7868 = DIRECTION ( 'NONE',  ( 0.6691306063588569053, -0.7431448254773954654, 0.000000000000000000 ) ) ;
#7869 = EDGE_LOOP ( 'NONE', ( #27521, #19781, #7308, #24719 ) ) ;
#7870 = EDGE_CURVE ( 'NONE', #2515, #7748, #33323, .T. ) ;
#7872 = DIRECTION ( 'NONE',  ( -0.9781476007338042455, 0.2079116908177663370, 0.000000000000000000 ) ) ;
#7871 = CARTESIAN_POINT ( 'NONE',  ( -17.71759125216689412, 12.53367430966638985, -21.16048139840979658 ) ) ;
#7873 = CARTESIAN_POINT ( 'NONE',  ( -11.41268156625113406, 18.79179606750104981, 13.00000000000000178 ) ) ;
#7874 = CARTESIAN_POINT ( 'NONE',  ( 9.640484335838371166, -18.33127209161421334, -27.44640424101937626 ) ) ;
#7875 = DIRECTION ( 'NONE',  ( 0.9135454576426059736, 0.4067366430757889395, -0.000000000000000000 ) ) ;
#7876 = CARTESIAN_POINT ( 'NONE',  ( 15.40208502184672135, 26.83309954512951023, -4.999999999999998224 ) ) ;
#7877 = CARTESIAN_POINT ( 'NONE',  ( -22.40982762235195835, 2.618079236897030704, -21.24786896499725231 ) ) ;
#7878 = PLANE ( 'NONE',  #25877 ) ;
#7879 = CARTESIAN_POINT ( 'NONE',  ( -15.82313792508790584, -13.97225745301835964, -26.33890869513203370 ) ) ;
#7880 = CARTESIAN_POINT ( 'NONE',  ( 5.143376291546045032, -22.33000100694908241, -17.91295319193513791 ) ) ;
#7881 = CARTESIAN_POINT ( 'NONE',  ( 15.44311626412968508, 26.25345304022521375, -6.888681639014727409 ) ) ;
#7882 = CARTESIAN_POINT ( 'NONE',  ( 19.51749221952617930, 13.16658399996466322, -13.89803554530751128 ) ) ;
#7883 = CARTESIAN_POINT ( 'NONE',  ( -3.713592597587352717, 7.966960743906856379, 7.499999999999997335 ) ) ;
#7885 = VERTEX_POINT ( 'NONE', #8119 ) ;
#7884 = EDGE_CURVE ( 'NONE', #11472, #12432, #2041, .T. ) ;
#7886 = CARTESIAN_POINT ( 'NONE',  ( -7.127291779580057884, 34.85034489748454689, -9.772412510442009648 ) ) ;
#7887 = EDGE_CURVE ( 'NONE', #19767, #36141, #31353, .T. ) ;
#7888 = EDGE_LOOP ( 'NONE', ( #17702, #12787, #29692 ) ) ;
#7889 = EDGE_CURVE ( 'NONE', #6833, #25338, #17081, .T. ) ;
#7890 = AXIS2_PLACEMENT_3D ( 'NONE', #15013, #8923, #2824 ) ;
#7891 = CARTESIAN_POINT ( 'NONE',  ( 12.41267482483262796, 26.20820393249957192, 12.00000000000000000 ) ) ;
#7892 = EDGE_LOOP ( 'NONE', ( #10844, #5182, #6489, #16210 ) ) ;
#7893 = VECTOR ( 'NONE', #29846, 1000.000000000000000 ) ;
#7894 = FACE_OUTER_BOUND ( 'NONE', #15800, .T. ) ;
#7895 = DIRECTION ( 'NONE',  ( -1.000000000000000000, 0.000000000000000000, 0.000000000000000000 ) ) ;
#7896 = EDGE_LOOP ( 'NONE', ( #17922, #37279, #31913, #19416 ) ) ;
#7897 = CARTESIAN_POINT ( 'NONE',  ( -23.25167227063256803, 0.7341704794712563542, -20.56396823476833902 ) ) ;
#7898 = VERTEX_POINT ( 'NONE', #1635 ) ;
#7899 = CARTESIAN_POINT ( 'NONE',  ( 34.05899686684449534, -10.24931931024947929, -9.342407649574157702 ) ) ;
#7900 = EDGE_LOOP ( 'NONE', ( #17195, #29897, #25908, #22234 ) ) ;
#7901 = APPLICATION_PROTOCOL_DEFINITION ( 'draft international standard', 'automotive_design', 1998, #21521 ) ;
#7902 = AXIS2_PLACEMENT_3D ( 'NONE', #3842, #9747, #38171 ) ;
#7903 = CARTESIAN_POINT ( 'NONE',  ( 13.48130249190479191, 27.93180293473185927, 10.50000000000000533 ) ) ;
#7904 = ORIENTED_EDGE ( 'NONE', *, *, #24739, .F. ) ;
#7905 = DIRECTION ( 'NONE',  ( 0.000000000000000000, 0.000000000000000000, -1.000000000000000000 ) ) ;
#7906 = CYLINDRICAL_SURFACE ( 'NONE', #26043, 1.000000000000000000 ) ;
#7907 = EDGE_CURVE ( 'NONE', #32385, #1779, #11245, .T. ) ;
#7908 = CARTESIAN_POINT ( 'NONE',  ( -12.17657648715623608, 27.34841683166460058, 18.87996532025750085 ) ) ;
#7909 = DIRECTION ( 'NONE',  ( 0.7431448254773953543, 0.6691306063588570163, 0.000000000000000000 ) ) ;
#7910 = VERTEX_POINT ( 'NONE', #38805 ) ;
#7911 = EDGE_CURVE ( 'NONE', #31854, #16687, #4744, .T. ) ;
#7912 =( LENGTH_UNIT ( ) NAMED_UNIT ( * ) SI_UNIT ( .MILLI., .METRE. ) );
#7913 = CARTESIAN_POINT ( 'NONE',  ( -16.72879317732252247, -11.86740072773090127, -30.00000000000002132 ) ) ;
#7914 = DIRECTION ( 'NONE',  ( 1.000000000000000000, 0.000000000000000000, 0.000000000000000000 ) ) ;
#7915 = DIRECTION ( 'NONE',  ( 0.000000000000000000, 0.000000000000000000, 1.000000000000000000 ) ) ;
#7916 = CARTESIAN_POINT ( 'NONE',  ( 18.05890274853723199, 15.78661794053360801, -13.85158280915597473 ) ) ;
#7917 = CARTESIAN_POINT ( 'NONE',  ( 10.15314824002201810, 31.60015277329938144, -11.20656053573065236 ) ) ;
#7918 = ORIENTED_EDGE ( 'NONE', *, *, #13621, .F. ) ;
#7919 = DIRECTION ( 'NONE',  ( 0.3090169943749450643, -0.9510565162951544194, 0.000000000000000000 ) ) ;
#7920 = CARTESIAN_POINT ( 'NONE',  ( -2.363107919609845009, 7.722275577009013681, 10.49999999999999467 ) ) ;
#7921 = CARTESIAN_POINT ( 'NONE',  ( 15.68476252645482205, -26.40036019609846107, -8.278550333207020273 ) ) ;
#7922 = CARTESIAN_POINT ( 'NONE',  ( 31.47283671532267846, -25.12609584734865464, -5.000000000000008882 ) ) ;
#7923 = LINE ( 'NONE', #39007, #24383 ) ;
#7924 = ORIENTED_EDGE ( 'NONE', *, *, #21335, .T. ) ;
#7925 = CARTESIAN_POINT ( 'NONE',  ( -12.65206519043741551, 21.05528877957942768, -18.45198030644581877 ) ) ;
#7926 = CARTESIAN_POINT ( 'NONE',  ( -33.86051255203334875, -2.258496953481841096, 15.13084544680166665 ) ) ;
#7927 = CARTESIAN_POINT ( 'NONE',  ( 12.73482621124554726, -24.80592790563511585, -11.64540342703255682 ) ) ;
#7928 = CARTESIAN_POINT ( 'NONE',  ( 1.000000000000000222, 36.00000000000000711, 9.500000000000000000 ) ) ;
#7929 = ORIENTED_EDGE ( 'NONE', *, *, #264, .T. ) ;
#7930 = VERTEX_POINT ( 'NONE', #26002 ) ;
#7931 = CARTESIAN_POINT ( 'NONE',  ( -12.58732244184787774, 32.13884721240458475, -6.785466956703739783 ) ) ;
#7932 = LINE ( 'NONE', #1650, #2945 ) ;
#7933 = FACE_BOUND ( 'NONE', #30692, .T. ) ;
#7934 = VECTOR ( 'NONE', #22321, 1000.000000000000000 ) ;
#7935 = CARTESIAN_POINT ( 'NONE',  ( -20.17828169183510667, -3.673208557823401943, -29.26865376204499114 ) ) ;
#7936 = LINE ( 'NONE', #23180, #23487 ) ;
#7937 = ORIENTED_EDGE ( 'NONE', *, *, #14773, .F. ) ;
#7938 = CARTESIAN_POINT ( 'NONE',  ( 20.47879743316550005, 0.9320964914785052624, -30.00000000000000000 ) ) ;
#7939 = DIRECTION ( 'NONE',  ( 1.000000000000000000, 0.000000000000000000, 0.000000000000000000 ) ) ;
#7940 = DIRECTION ( 'NONE',  ( -0.6691306063588560171, 0.7431448254773962425, 0.000000000000000000 ) ) ;
#7941 = CARTESIAN_POINT ( 'NONE',  ( -32.57473823703268323, -23.68076927422058731, 10.99999999999993960 ) ) ;
#7942 = UNCERTAINTY_MEASURE_WITH_UNIT (LENGTH_MEASURE( 1.000000000000000082E-05 ), #36754, 'distance_accuracy_value', 'NONE');
#7943 = ORIENTED_EDGE ( 'NONE', *, *, #17665, .F. ) ;
#7944 = CARTESIAN_POINT ( 'NONE',  ( -30.86643083211014016, -0.03928469928488562135, -5.946079256554607007 ) ) ;
#7945 = DIRECTION ( 'NONE',  ( 1.000000000000000000, 0.000000000000000000, 0.000000000000000000 ) ) ;
#7946 = ORIENTED_EDGE ( 'NONE', *, *, #24930, .T. ) ;
#7947 = CARTESIAN_POINT ( 'NONE',  ( 31.76370184099492633, -4.744110583585224639, -11.28924081358098341 ) ) ;
#7948 = AXIS2_PLACEMENT_3D ( 'NONE', #37253, #21413, #2536 ) ;
#7949 = CARTESIAN_POINT ( 'NONE',  ( 34.31157940325252298, -4.066883398345114919, 15.72805884748939853 ) ) ;
#7950 = ORIENTED_EDGE ( 'NONE', *, *, #29798, .T. ) ;
#7951 = CARTESIAN_POINT ( 'NONE',  ( 14.19638663437042503, 32.12978188971815285, 14.53008259254012025 ) ) ;
#7952 = CARTESIAN_POINT ( 'NONE',  ( 10.43399472913278103, -25.44514827092724829, 16.30093088679983637 ) ) ;
#7953 = DIRECTION ( 'NONE',  ( 1.000000000000000000, 0.000000000000000000, 0.000000000000000000 ) ) ;
#7954 = CARTESIAN_POINT ( 'NONE',  ( 8.084325832714235105, 26.79336336920809813, 20.50957957746030047 ) ) ;
#7955 = CARTESIAN_POINT ( 'NONE',  ( -12.39464589777671044, 26.66807349098043289, 6.000000000000000000 ) ) ;
#7956 = EDGE_LOOP ( 'NONE', ( #19320, #23627, #10427, #10080 ) ) ;
#7957 = VECTOR ( 'NONE', #30892, 1000.000000000000000 ) ;
#7958 = LINE ( 'NONE', #29702, #35092 ) ;
#7959 = CARTESIAN_POINT ( 'NONE',  ( 6.075063716662223001, 37.19263437435982667, -6.287285438531430515 ) ) ;
#7960 = VECTOR ( 'NONE', #1912, 1000.000000000000000 ) ;
#7961 = DIRECTION ( 'NONE',  ( 0.000000000000000000, 0.000000000000000000, -1.000000000000000000 ) ) ;
#7962 = CARTESIAN_POINT ( 'NONE',  ( 14.04126239388501496, 8.106726622871901711, 20.82122704794079837 ) ) ;
#7963 = CARTESIAN_POINT ( 'NONE',  ( 14.22296627154594084, -18.85705313786432313, -21.18946184155140244 ) ) ;
#7964 = CARTESIAN_POINT ( 'NONE',  ( 5.440908595777814050, 35.94977745735560859, 7.000000000000000000 ) ) ;
#7965 = CARTESIAN_POINT ( 'NONE',  ( -13.24038105676664401, 15.43301270189234309, 10.50000000000000355 ) ) ;
#7966 = DIRECTION ( 'NONE',  ( 0.000000000000000000, 0.000000000000000000, 1.000000000000000000 ) ) ;
#7967 = VERTEX_POINT ( 'NONE', #23369 ) ;
#7968 = CIRCLE ( 'NONE', #30052, 6.000000000000003553 ) ;
#7969 = CARTESIAN_POINT ( 'NONE',  ( 11.60819584869819288, 18.98628572600766518, -22.72157423742040905 ) ) ;
#7970 = ORIENTED_EDGE ( 'NONE', *, *, #7045, .F. ) ;
#7971 = CARTESIAN_POINT ( 'NONE',  ( -15.43622781282135215, 26.27460386919110746, -6.888601964265022026 ) ) ;
#7972 = CARTESIAN_POINT ( 'NONE',  ( -26.17288861939861988, -20.72787579792414903, 19.66345542862528362 ) ) ;
#7973 = CARTESIAN_POINT ( 'NONE',  ( 13.63581098909227052, 27.45627467658428600, 9.500000000000000000 ) ) ;
#7974 = CARTESIAN_POINT ( 'NONE',  ( 14.76676254508215713, 25.31098156848036851, -10.65510591171607579 ) ) ;
#7975 = VERTEX_POINT ( 'NONE', #1842 ) ;
#7976 = CARTESIAN_POINT ( 'NONE',  ( 31.77261430474117532, -21.49768664888851788, -4.999999999999999112 ) ) ;
#7977 = ORIENTED_EDGE ( 'NONE', *, *, #26033, .T. ) ;
#7979 = LINE ( 'NONE', #1906, #2409 ) ;
#7978 = CARTESIAN_POINT ( 'NONE',  ( -14.67061210956474326, 28.11310680807456208, -7.773254751785441563 ) ) ;
#7980 = CARTESIAN_POINT ( 'NONE',  ( -16.71012240396724025, -26.29450614545289611, -9.160826647832207570 ) ) ;
#7981 = CARTESIAN_POINT ( 'NONE',  ( 0.000000000000000000, 22.50000000000000355, 7.000000000000000000 ) ) ;
#7982 = PRESENTATION_LAYER_ASSIGNMENT (  '', '', ( #222 ) ) ;
#7983 = ORIENTED_EDGE ( 'NONE', *, *, #13870, .T. ) ;
#7984 = CARTESIAN_POINT ( 'NONE',  ( -28.69690197025867562, -11.83258904652041643, -14.76511728228867604 ) ) ;
#7985 = CARTESIAN_POINT ( 'NONE',  ( -14.45483107746191465, -26.00542429865824090, -8.773822038624603081 ) ) ;
#7986 = LINE ( 'NONE', #14490, #28060 ) ;
#7987 = CARTESIAN_POINT ( 'NONE',  ( 16.77170801253743448, 22.01473390083994275, -7.380717902106597172 ) ) ;
#7988 = ORIENTED_EDGE ( 'NONE', *, *, #6094, .F. ) ;
#7989 = CARTESIAN_POINT ( 'NONE',  ( 20.54205287650563250, 2.405902401984270522, -27.54068107859523096 ) ) ;
#7990 = EDGE_CURVE ( 'NONE', #11320, #9704, #31622, .T. ) ;
#7991 = LINE ( 'NONE', #17559, #39457 ) ;
#7992 = CIRCLE ( 'NONE', #35225, 1.000000000000000000 ) ;
#7993 = CARTESIAN_POINT ( 'NONE',  ( -29.22254794994760729, -28.85350742528338586, 22.99999999999905853 ) ) ;
#7994 = ORIENTED_EDGE ( 'NONE', *, *, #16600, .F. ) ;
#7995 = CARTESIAN_POINT ( 'NONE',  ( -30.57520037393770451, -0.1065157518614621435, -7.823604440374101188 ) ) ;
#7996 = CARTESIAN_POINT ( 'NONE',  ( 27.50873112917703978, -0.2858532659916371843, -14.41729497493959045 ) ) ;
#7997 = AXIS2_PLACEMENT_3D ( 'NONE', #15656, #6693, #22337 ) ;
#7998 = EDGE_CURVE ( 'NONE', #30397, #6485, #1519, .T. ) ;
#7999 = CARTESIAN_POINT ( 'NONE',  ( 23.01245512501257551, -23.08877437847652558, 19.27171037444193757 ) ) ;
#8000 = EDGE_LOOP ( 'NONE', ( #22407, #31886, #21543, #39311 ) ) ;
#8001 = CARTESIAN_POINT ( 'NONE',  ( -21.17204097405855023, 1.464915700757598360, -25.08531244034496055 ) ) ;
#8002 = EDGE_CURVE ( 'NONE', #11250, #31137, #8526, .T. ) ;
#8003 = CARTESIAN_POINT ( 'NONE',  ( -16.84920187454419960, 29.09530251867925443, -13.79123840944734170 ) ) ;
#8004 = CIRCLE ( 'NONE', #39147, 0.5000000000000004441 ) ;
#8005 = DIRECTION ( 'NONE',  ( -0.4999999999999921729, 0.8660254037844432595, 0.000000000000000000 ) ) ;
#8006 = CIRCLE ( 'NONE', #35916, 1.000000000000000888 ) ;
#8007 = DIRECTION ( 'NONE',  ( 0.000000000000000000, 0.000000000000000000, 1.000000000000000000 ) ) ;
#8008 = VECTOR ( 'NONE', #35302, 1000.000000000000114 ) ;
#8009 = DIRECTION ( 'NONE',  ( -0.4067366430757888285, 0.9135454576426059736, -0.000000000000000000 ) ) ;
#8010 = CARTESIAN_POINT ( 'NONE',  ( 0.000000000000000000, 22.50000000000000355, 0.000000000000000000 ) ) ;
#8011 = CARTESIAN_POINT ( 'NONE',  ( -6.312041872459064784, 25.58773265502866678, 12.00000000000000000 ) ) ;
#8012 = ORIENTED_EDGE ( 'NONE', *, *, #26918, .T. ) ;
#8013 = CARTESIAN_POINT ( 'NONE',  ( -21.59735981781079417, 5.059875484007670288, -20.98042407182869340 ) ) ;
#8014 = CARTESIAN_POINT ( 'NONE',  ( -1.229437847141422901, 24.50739181907689712, 6.000000000000000000 ) ) ;
#8015 = ADVANCED_FACE ( 'NONE', ( #39603 ), #30270, .T. ) ;
#8016 = FACE_OUTER_BOUND ( 'NONE', #39782, .T. ) ;
#8017 = CARTESIAN_POINT ( 'NONE',  ( 26.32663925810967953, -25.71384748841218837, -4.999999999999998224 ) ) ;
#8018 = LINE ( 'NONE', #17789, #26820 ) ;
#8019 = CARTESIAN_POINT ( 'NONE',  ( -14.98890121934610242, -28.67928442654176635, 0.000000000000000000 ) ) ;
#8020 = CARTESIAN_POINT ( 'NONE',  ( 15.30309001416959802, 27.17055420720160441, -4.999999999999999112 ) ) ;
#8021 = CARTESIAN_POINT ( 'NONE',  ( -0.2655091840902661926, 8.754836972118123839, 12.00000000000000000 ) ) ;
#8022 = VERTEX_POINT ( 'NONE', #15021 ) ;
#8023 = AXIS2_PLACEMENT_3D ( 'NONE', #7709, #35345, #16660 ) ;
#8024 = CARTESIAN_POINT ( 'NONE',  ( -16.25978453391780221, 22.36894860302335886, -9.288381802591871406 ) ) ;
#8025 = CARTESIAN_POINT ( 'NONE',  ( -21.91981567634955397, -15.65087685632102499, 20.99999999999999645 ) ) ;
#8026 = CARTESIAN_POINT ( 'NONE',  ( 15.21665703708782935, -26.47879611614396111, -7.358218835048320194 ) ) ;
#8027 = DIRECTION ( 'NONE',  ( -0.000000000000000000, -0.000000000000000000, 1.000000000000000000 ) ) ;
#8028 = CARTESIAN_POINT ( 'NONE',  ( 12.40183761314701449, 20.47613423964896029, -19.49836111761218405 ) ) ;
#8029 = EDGE_LOOP ( 'NONE', ( #38816, #17314, #3759, #12872 ) ) ;
#8030 = CARTESIAN_POINT ( 'NONE',  ( -14.52509594610762278, 21.97885917798745226, 10.49999999999999822 ) ) ;
#8031 = ORIENTED_EDGE ( 'NONE', *, *, #11316, .F. ) ;
#8033 = DIRECTION ( 'NONE',  ( -0.000000000000000000, -0.000000000000000000, 1.000000000000000000 ) ) ;
#8032 = CARTESIAN_POINT ( 'NONE',  ( -13.41058178396609080, 22.98005122180817139, -15.43185508673824735 ) ) ;
#8034 = CARTESIAN_POINT ( 'NONE',  ( -15.44635164275937811, -26.65726164833965228, -6.416678024205798359 ) ) ;
#8035 = CARTESIAN_POINT ( 'NONE',  ( -34.10020663062397972, -21.93670956716203690, 11.00000000000017231 ) ) ;
#8036 = CARTESIAN_POINT ( 'NONE',  ( -17.29914876638407861, -11.16020024788362974, -28.44682971825362827 ) ) ;
#8037 = CARTESIAN_POINT ( 'NONE',  ( -6.226074173696266811, -19.80104272504923557, -27.05930787988562258 ) ) ;
#8038 = CARTESIAN_POINT ( 'NONE',  ( 15.49015922161475167, 24.15577049684528887, -9.735419282224947679 ) ) ;
#8039 = ORIENTED_EDGE ( 'NONE', *, *, #15345, .F. ) ;
#8040 = CARTESIAN_POINT ( 'NONE',  ( 23.97835192852010167, 8.298819924180955709, -6.446434780486328009 ) ) ;
#8041 = LINE ( 'NONE', #36088, #30996 ) ;
#8042 = CARTESIAN_POINT ( 'NONE',  ( -6.688306800005769048, 28.52217545723006609, 6.000000000000000000 ) ) ;
#8043 = DIRECTION ( 'NONE',  ( 1.000000000000000000, 0.000000000000000000, 0.000000000000000000 ) ) ;
#8044 = EDGE_LOOP ( 'NONE', ( #23833, #10354 ) ) ;
#8045 = CARTESIAN_POINT ( 'NONE',  ( -32.30815150485408793, -1.680769291408187316, -5.000000000000000000 ) ) ;
#8046 = EDGE_CURVE ( 'NONE', #10907, #38994, #31990, .T. ) ;
#8047 = STYLED_ITEM ( 'NONE', ( #31 ), #9362 ) ;
#8048 = LINE ( 'NONE', #32853, #11820 ) ;
#8049 = CARTESIAN_POINT ( 'NONE',  ( 22.70288158165702086, -17.06695585772177992, 20.94377226548368043 ) ) ;
#8050 = CARTESIAN_POINT ( 'NONE',  ( -11.01950087092618524, 17.43848460801469002, -28.07618716959215277 ) ) ;
#8051 = DIRECTION ( 'NONE',  ( -0.9945218953682744001, -0.1045284632676437564, 0.000000000000000000 ) ) ;
#8052 = ADVANCED_FACE ( 'NONE', ( #11777 ), #2438, .F. ) ;
#8053 = LINE ( 'NONE', #26744, #29421 ) ;
#8054 = CARTESIAN_POINT ( 'NONE',  ( 19.35680011505175457, -9.211710752562881410, -25.58994971620333558 ) ) ;
#8055 = CYLINDRICAL_SURFACE ( 'NONE', #2443, 1.000000000000000000 ) ;
#8056 = CONICAL_SURFACE ( 'NONE', #30770, 0.5000000000000046629, 0.7853981633974503884 ) ;
#8057 = VERTEX_POINT ( 'NONE', #21121 ) ;
#8058 = LINE ( 'NONE', #4615, #7400 ) ;
#8059 = PLANE ( 'NONE',  #37001 ) ;
#8060 = DIRECTION ( 'NONE',  ( 0.000000000000000000, 0.000000000000000000, 1.000000000000000000 ) ) ;
#8061 = CONICAL_SURFACE ( 'NONE', #38542, 0.5000000000000108802, 0.7853981633974482790 ) ;
#8062 = CARTESIAN_POINT ( 'NONE',  ( 0.4110586764534028270, 38.44431916748334288, -5.855741157794193796 ) ) ;
#8063 = CARTESIAN_POINT ( 'NONE',  ( -11.14717575287011542, 32.53695909538323860, 6.000000000000000000 ) ) ;
#8064 = EDGE_CURVE ( 'NONE', #25619, #20347, #23566, .T. ) ;
#8065 = CARTESIAN_POINT ( 'NONE',  ( -13.94482798346716201, 26.50521816028930644, 7.000000000000000000 ) ) ;
#8066 = ADVANCED_FACE ( 'NONE', ( #2633 ), #17689, .T. ) ;
#8067 = LINE ( 'NONE', #33475, #12156 ) ;
#8068 = DIRECTION ( 'NONE',  ( 0.5877852522924796874, 0.8090169943749426773, 0.000000000000000000 ) ) ;
#8069 = DIRECTION ( 'NONE',  ( 0.000000000000000000, 0.000000000000000000, 1.000000000000000000 ) ) ;
#8070 = AXIS2_PLACEMENT_3D ( 'NONE', #14221, #17694, #17491 ) ;
#8071 = CARTESIAN_POINT ( 'NONE',  ( 9.903829054754655914, 18.12412366152800658, -28.01031554129876966 ) ) ;
#8072 = CARTESIAN_POINT ( 'NONE',  ( 14.52509594610761923, 21.97885917798724975, 7.000000000000000000 ) ) ;
#8073 = EDGE_LOOP ( 'NONE', ( #3596, #35127 ) ) ;
#8075 = CARTESIAN_POINT ( 'NONE',  ( 14.26584774442731884, 27.13525491562417713, 7.000000000000000000 ) ) ;
#8074 = CARTESIAN_POINT ( 'NONE',  ( -16.91598364292035939, 12.90154645153827140, -23.29995136833793268 ) ) ;
#8076 = CARTESIAN_POINT ( 'NONE',  ( -0.4999999999999998890, 37.00000000000000711, 10.99999999999999645 ) ) ;
#8077 = CARTESIAN_POINT ( 'NONE',  ( 14.88972759991149530, -25.83697725034997461, -9.708168427115946741 ) ) ;
#8078 = DIRECTION ( 'NONE',  ( -0.000000000000000000, -0.000000000000000000, -1.000000000000000000 ) ) ;
#8079 = CARTESIAN_POINT ( 'NONE',  ( 15.38794517075334056, 26.79091751018437861, -5.945654618937589397 ) ) ;
#8080 = DIRECTION ( 'NONE',  ( -1.000000000000000000, 0.000000000000000000, 0.000000000000000000 ) ) ;
#8081 = FACE_OUTER_BOUND ( 'NONE', #22730, .T. ) ;
#8082 = AXIS2_PLACEMENT_3D ( 'NONE', #19806, #13293, #35042 ) ;
#8083 = CARTESIAN_POINT ( 'NONE',  ( -17.65121957807252784, -15.59521983380484222, -21.96053948915082188 ) ) ;
#8084 = CARTESIAN_POINT ( 'NONE',  ( 4.234769651857060779, -20.16607359150837553, -27.68998930902958122 ) ) ;
#8085 = CARTESIAN_POINT ( 'NONE',  ( 14.85392080762270339, 25.05954230463082766, -10.66070852731747998 ) ) ;
#8086 = CARTESIAN_POINT ( 'NONE',  ( 17.99011237037677802, 13.10895772829668182, -19.04357418431120763 ) ) ;
#8087 = CARTESIAN_POINT ( 'NONE',  ( 9.541469607472739867, 17.40487552589537401, 6.000000000000000000 ) ) ;
#8088 = EDGE_LOOP ( 'NONE', ( #26285, #32721, #26591, #27744 ) ) ;
#8089 = CARTESIAN_POINT ( 'NONE',  ( -6.361647429086256800, 31.06932854847694969, -13.87644038312246764 ) ) ;
#8090 = VERTEX_POINT ( 'NONE', #27214 ) ;
#8091 = EDGE_CURVE ( 'NONE', #28113, #12049, #25482, .T. ) ;
#8092 = CARTESIAN_POINT ( 'NONE',  ( -0.4999999999999998890, 37.50000000000000711, 11.00000000000000000 ) ) ;
#8093 = VERTEX_POINT ( 'NONE', #1362 ) ;
#8094 = DIRECTION ( 'NONE',  ( -0.9135454576426059736, -0.4067366430757889395, 0.000000000000000000 ) ) ;
#8095 = DIRECTION ( 'NONE',  ( 0.6724985119639536046, -0.2185080122244175416, -0.7071067811865489050 ) ) ;
#8096 = ORIENTED_EDGE ( 'NONE', *, *, #24041, .F. ) ;
#8097 = CARTESIAN_POINT ( 'NONE',  ( -29.61458559055934714, 0.2518799484168193770, -9.713275453577335128 ) ) ;
#8098 = VERTEX_POINT ( 'NONE', #39337 ) ;
#8099 = CARTESIAN_POINT ( 'NONE',  ( 28.16713897950105405, -8.472997818002736992, -15.79648965232683544 ) ) ;
#8100 = VECTOR ( 'NONE', #17847, 1000.000000000000000 ) ;
#8101 = VERTEX_POINT ( 'NONE', #5008 ) ;
#8102 = DIRECTION ( 'NONE',  ( 0.000000000000000000, 0.000000000000000000, 1.000000000000000000 ) ) ;
#8103 = ORIENTED_EDGE ( 'NONE', *, *, #35561, .T. ) ;
#8104 = DIRECTION ( 'NONE',  ( -1.000000000000000000, 0.000000000000000000, 0.000000000000000000 ) ) ;
#8105 = CIRCLE ( 'NONE', #34073, 0.5000000000000002220 ) ;
#8106 = CARTESIAN_POINT ( 'NONE',  ( -7.096882951594430722, 29.56287847632736288, 10.49999999999999822 ) ) ;
#8107 = CARTESIAN_POINT ( 'NONE',  ( -4.383143208095260590, 35.51174355874280053, 18.42518152272109333 ) ) ;
#8108 = VECTOR ( 'NONE', #20872, 1000.000000000000000 ) ;
#8109 = CARTESIAN_POINT ( 'NONE',  ( -3.963760424820539363, 8.194319839800240146, 10.49999999999999467 ) ) ;
#8110 = ORIENTED_EDGE ( 'NONE', *, *, #30287, .F. ) ;
#8111 =( LENGTH_UNIT ( ) NAMED_UNIT ( * ) SI_UNIT ( .MILLI., .METRE. ) );
#8112 = CARTESIAN_POINT ( 'NONE',  ( -13.39464589777671044, 26.66807349098043289, 6.000000000000000000 ) ) ;
#8113 = DIRECTION ( 'NONE',  ( 0.000000000000000000, 0.000000000000000000, 1.000000000000000000 ) ) ;
#8114 = DIRECTION ( 'NONE',  ( 0.1045284632676569680, 0.9945218953682729568, -0.000000000000000000 ) ) ;
#8115 = EDGE_CURVE ( 'NONE', #38307, #3978, #23700, .T. ) ;
#8116 = CARTESIAN_POINT ( 'NONE',  ( 14.85614242573017840, 14.30966537380568759, -27.67306061729238209 ) ) ;
#8117 = CARTESIAN_POINT ( 'NONE',  ( 8.359857552323353147, 21.45424803955862458, -22.25965238277191460 ) ) ;
#8118 = VERTEX_POINT ( 'NONE', #33063 ) ;
#8119 = CARTESIAN_POINT ( 'NONE',  ( -9.831584923911583118, 26.22020669908462764, 10.00000000000000000 ) ) ;
#8120 = CARTESIAN_POINT ( 'NONE',  ( -2.629601561899595374, 7.723830143584053509, 10.49999999999999822 ) ) ;
#8121 = CARTESIAN_POINT ( 'NONE',  ( 13.23316282574661251, -23.10607048933782082, -15.42806814948440497 ) ) ;
#8122 = PLANE ( 'NONE',  #35982 ) ;
#8123 = B_SPLINE_CURVE_WITH_KNOTS ( 'NONE', 3,
 ( #902, #38275, #34824, #16341 ),
 .UNSPECIFIED., .F., .F.,
 ( 4, 4 ),
 ( 0.6666666663583977748, 1.000000000000000000 ),
 .UNSPECIFIED. ) ;
#8124 = DIRECTION ( 'NONE',  ( 0.5000000000000043299, 0.8660254037844361541, 0.000000000000000000 ) ) ;
#8125 = VECTOR ( 'NONE', #20543, 999.9999999999998863 ) ;
#8126 = CARTESIAN_POINT ( 'NONE',  ( -11.47830338918615745, 18.44249444189321707, -23.85302490474181880 ) ) ;
#8127 = CARTESIAN_POINT ( 'NONE',  ( -26.23899120466318280, -27.34191102820705055, 13.92931973827808534 ) ) ;
#8128 = CARTESIAN_POINT ( 'NONE',  ( 11.58858825903818257, -23.03010094018678089, -15.54224781274825595 ) ) ;
#8129 = DIRECTION ( 'NONE',  ( -0.000000000000000000, -0.000000000000000000, -1.000000000000000000 ) ) ;
#8130 = VERTEX_POINT ( 'NONE', #32242 ) ;
#8131 = VERTEX_POINT ( 'NONE', #32450 ) ;
#8132 = CARTESIAN_POINT ( 'NONE',  ( -11.75129741676435380, 32.67431248936103572, -7.653645928010829103 ) ) ;
#8133 = VECTOR ( 'NONE', #38506, 1000.000000000000000 ) ;
#8134 = DIRECTION ( 'NONE',  ( -0.9945218953682745111, -0.1045284632676436454, 0.000000000000000000 ) ) ;
#8135 = ADVANCED_FACE ( 'NONE', ( #4611 ), #14557, .F. ) ;
#8136 = DIRECTION ( 'NONE',  ( 0.000000000000000000, 0.000000000000000000, 1.000000000000000000 ) ) ;
#8137 = AXIS2_PLACEMENT_3D ( 'NONE', #30809, #9862, #19006 ) ;
#8139 = AXIS2_PLACEMENT_3D ( 'NONE', #12588, #31081, #31279 ) ;
#8138 = CARTESIAN_POINT ( 'NONE',  ( -33.33009440080085284, -5.279162264021511675, -9.006299637744488606 ) ) ;
#8140 = CARTESIAN_POINT ( 'NONE',  ( -8.559512017365658920, 19.71884705062586107, 12.00000000000000000 ) ) ;
#8141 = ORIENTED_EDGE ( 'NONE', *, *, #39373, .F. ) ;
#8142 = CARTESIAN_POINT ( 'NONE',  ( 28.81778564524760000, 0.1882255715981525357, -11.60218017744097807 ) ) ;
#8143 = EDGE_CURVE ( 'NONE', #1258, #25235, #6696, .T. ) ;
#8144 = CARTESIAN_POINT ( 'NONE',  ( 8.927394655428276593, 11.06314620770945290, 7.500000000000000888 ) ) ;
#8145 = CARTESIAN_POINT ( 'NONE',  ( -8.593266739736661108, 16.38397459621564067, 10.50000000000000000 ) ) ;
#8146 = CARTESIAN_POINT ( 'NONE',  ( -5.362728154696096539, 13.41753630677062148, 10.50000000000000711 ) ) ;
#8147 = ORIENTED_EDGE ( 'NONE', *, *, #36682, .T. ) ;
#8148 = CARTESIAN_POINT ( 'NONE',  ( -23.31383330372760909, 0.5610641285874745643, -20.54315880825037510 ) ) ;
#8149 = CARTESIAN_POINT ( 'NONE',  ( -13.60579549876895911, 27.97225316470548862, 10.49999999999999822 ) ) ;
#8150 = VERTEX_POINT ( 'NONE', #7653 ) ;
#8151 = CARTESIAN_POINT ( 'NONE',  ( 20.68113486913782850, -2.268168025704259794, -27.24842174564768982 ) ) ;
#8152 = EDGE_CURVE ( 'NONE', #13390, #4137, #1769, .T. ) ;
#8153 = CARTESIAN_POINT ( 'NONE',  ( 18.87563634320844130, -28.49365729390225965, 14.53008259254033163 ) ) ;
#8154 = ORIENTED_EDGE ( 'NONE', *, *, #1889, .F. ) ;
#8155 = MANIFOLD_SOLID_BREP ( 'Boss-Extrude2', #19662 ) ;
#8156 = CARTESIAN_POINT ( 'NONE',  ( -10.19952947928024933, 35.92118758406519419, 15.13084544680213384 ) ) ;
#8157 = CARTESIAN_POINT ( 'NONE',  ( 5.178899460637698127, -25.25135431486990711, 15.72805884748939853 ) ) ;
#8158 = CARTESIAN_POINT ( 'NONE',  ( -10.36702044712414938, 31.16169077310601665, 10.50000000000000000 ) ) ;
#8159 = CARTESIAN_POINT ( 'NONE',  ( 1.610977985362757936, 29.80447555512223445, 20.82122704794079482 ) ) ;
#8160 = CARTESIAN_POINT ( 'NONE',  ( 8.718890067807359756, 5.003589289612210500, 10.00000000000000000 ) ) ;
#8161 = ORIENTED_EDGE ( 'NONE', *, *, #2172, .F. ) ;
#8162 = DIRECTION ( 'NONE',  ( 0.5877852522924691403, -0.8090169943749503378, -6.938893903907234689E-15 ) ) ;
#8163 = CIRCLE ( 'NONE', #20505, 15.00000000000000000 ) ;
#8164 = EDGE_CURVE ( 'NONE', #38004, #29091, #38531, .T. ) ;
#8165 = EDGE_CURVE ( 'NONE', #33425, #3338, #17113, .T. ) ;
#8166 = AXIS2_PLACEMENT_3D ( 'NONE', #11333, #20479, #20273 ) ;
#8167 = CARTESIAN_POINT ( 'NONE',  ( 4.527020475796621923, 33.83005428846027485, -11.99704615662030527 ) ) ;
#8168 = VECTOR ( 'NONE', #31025, 1000.000000000000000 ) ;
#8169 = DIRECTION ( 'NONE',  ( -0.6691306063588569053, 0.7431448254773954654, 0.000000000000000000 ) ) ;
#8170 = CARTESIAN_POINT ( 'NONE',  ( 7.164929079092710928, 24.49151390637290149, 20.82122704794079837 ) ) ;
#8171 = AXIS2_PLACEMENT_3D ( 'NONE', #18871, #10324, #31262 ) ;
#8172 = CARTESIAN_POINT ( 'NONE',  ( 17.86692456966301989, -23.49199618837229764, -14.12595633806949103 ) ) ;
#8173 = DIRECTION ( 'NONE',  ( -0.000000000000000000, -0.000000000000000000, -1.000000000000000000 ) ) ;
#8174 = CARTESIAN_POINT ( 'NONE',  ( -13.21633681164003171, 15.44689465328864486, 10.68306113187833084 ) ) ;
#8175 = CARTESIAN_POINT ( 'NONE',  ( 1.623731701744046241, 25.43444280220171194, 13.00000000000000178 ) ) ;
#8176 = EDGE_LOOP ( 'NONE', ( #17345, #7124 ) ) ;
#8177 = CARTESIAN_POINT ( 'NONE',  ( 11.83320386989883488, 19.44516747061696904, -21.60573074431047402 ) ) ;
#8178 = ORIENTED_EDGE ( 'NONE', *, *, #25883, .F. ) ;
#8179 = CARTESIAN_POINT ( 'NONE',  ( -12.78688490849339487, 19.97022096780329292, -19.56400173231042317 ) ) ;
#8180 = CARTESIAN_POINT ( 'NONE',  ( -21.83517059620288236, -24.14399886393494299, 18.87996532025750795 ) ) ;
#8181 = CARTESIAN_POINT ( 'NONE',  ( -3.458872323573595864, 26.51478363815348160, 6.000000000000000000 ) ) ;
#8182 = CARTESIAN_POINT ( 'NONE',  ( 14.99150837520656410, 25.62483198016352759, -9.711665107101897121 ) ) ;
#8183 = EDGE_LOOP ( 'NONE', ( #26587, #4815, #12559, #31094 ) ) ;
#8184 = CARTESIAN_POINT ( 'NONE',  ( 32.47636040670842306, -20.57534817285772277, -5.855945076690642459 ) ) ;
#8185 = ORIENTED_EDGE ( 'NONE', *, *, #485, .T. ) ;
#8187 = DIRECTION ( 'NONE',  ( -0.9510565162951497564, 0.3090169943749591086, -3.469446951953608667E-15 ) ) ;
#8186 = CARTESIAN_POINT ( 'NONE',  ( -14.50613712064790306, 26.05512619081983772, -10.61110433390421015 ) ) ;
#8188 = CARTESIAN_POINT ( 'NONE',  ( -18.34279529041538126, -27.21360250413895443, -5.919932557224159453 ) ) ;
#8189 = ADVANCED_FACE ( 'NONE', ( #23301 ), #26551, .T. ) ;
#8190 = DIRECTION ( 'NONE',  ( 0.000000000000000000, 0.000000000000000000, 1.000000000000000000 ) ) ;
#8191 = EDGE_LOOP ( 'NONE', ( #4468, #34993, #2724, #28577 ) ) ;
#8192 = CARTESIAN_POINT ( 'NONE',  ( -35.12294622822932411, -10.95518361376287508, -7.153933696636912032 ) ) ;
#8193 = CARTESIAN_POINT ( 'NONE',  ( -14.01793117240702458, -25.34536848690236255, -10.66627488844276073 ) ) ;
#8194 = CARTESIAN_POINT ( 'NONE',  ( 20.38753357181587234, -16.19769905861744519, 23.00000000000000000 ) ) ;
#8195 = ORIENTED_EDGE ( 'NONE', *, *, #6787, .T. ) ;
#8196 = CARTESIAN_POINT ( 'NONE',  ( 27.89362309832364417, 2.032256754323124248, -10.22863755220655513 ) ) ;
#8197 = EDGE_CURVE ( 'NONE', #15130, #16687, #35696, .T. ) ;
#8198 = DIRECTION ( 'NONE',  ( -0.000000000000000000, -0.000000000000000000, -1.000000000000000000 ) ) ;
#8199 = CARTESIAN_POINT ( 'NONE',  ( -34.33271597228865346, -24.82403720151219417, 23.00000000000000000 ) ) ;
#8200 = AXIS2_PLACEMENT_3D ( 'NONE', #37412, #37618, #12823 ) ;
#8201 = ORIENTED_EDGE ( 'NONE', *, *, #12790, .F. ) ;
#8202 = CARTESIAN_POINT ( 'NONE',  ( -20.61417483570997433, 0.7840236751464569886, -28.07419235526585055 ) ) ;
#8203 = B_SPLINE_CURVE_WITH_KNOTS ( 'NONE', 3,
 ( #27273, #31120, #21177, #18730, #33781, #36814 ),
 .UNSPECIFIED., .F., .F.,
 ( 4, 2, 4 ),
 ( 0.1333333595060078314, 0.5666666797530039990, 1.000000000000000000 ),
 .UNSPECIFIED. ) ;
#8204 = CARTESIAN_POINT ( 'NONE',  ( 28.39197557152373363, -0.7107394051037417837, -13.42105332491729541 ) ) ;
#8205 = TOROIDAL_SURFACE ( 'NONE', #28315, 1.000000000000000000, 0.5000000000000000000 ) ;
#8206 = CARTESIAN_POINT ( 'NONE',  ( 30.59706755222660135, -4.299425952516082283, 18.87996532025822916 ) ) ;
#8207 = AXIS2_PLACEMENT_3D ( 'NONE', #26275, #13886, #32175 ) ;
#8208 = EDGE_LOOP ( 'NONE', ( #39982, #740, #203 ) ) ;
#8209 = CARTESIAN_POINT ( 'NONE',  ( -29.17914473192155711, 1.735411910516140299, -5.947304834939044049 ) ) ;
#8210 = CARTESIAN_POINT ( 'NONE',  ( -22.45323650136969462, -2.382502413133420038, -20.55760979252980647 ) ) ;
#8211 = CARTESIAN_POINT ( 'NONE',  ( 14.81901435602781802, 20.17583222033112733, 7.455539900862803826 ) ) ;
#8212 = FACE_OUTER_BOUND ( 'NONE', #3229, .T. ) ;
#8213 = DIRECTION ( 'NONE',  ( 0.4067366430757888840, -0.9135454576426058626, -0.000000000000000000 ) ) ;
#8214 = DIRECTION ( 'NONE',  ( 1.000000000000000000, 0.000000000000000000, 0.000000000000000000 ) ) ;
#8215 = CARTESIAN_POINT ( 'NONE',  ( 12.63581098909226341, 27.45627467658428955, 7.000000000000000000 ) ) ;
#8216 = EDGE_LOOP ( 'NONE', ( #33894, #16935, #17059, #27761 ) ) ;
#8217 = CARTESIAN_POINT ( 'NONE',  ( -25.87260067993565116, 5.291969182969162411, -8.360226650860235864 ) ) ;
#8218 = DIRECTION ( 'NONE',  ( 1.000000000000000000, 0.000000000000000000, 0.000000000000000000 ) ) ;
#8219 = CARTESIAN_POINT ( 'NONE',  ( -12.80736835487442349, 15.68301270189233954, 7.000000000000000000 ) ) ;
#8220 = CARTESIAN_POINT ( 'NONE',  ( 25.59259726831772497, -25.05938252355970519, -8.471152770727268688 ) ) ;
#8221 = EDGE_CURVE ( 'NONE', #11661, #32239, #20056, .T. ) ;
#8222 = LINE ( 'NONE', #39098, #5393 ) ;
#8223 = PLANE ( 'NONE',  #11264 ) ;
#8224 = CARTESIAN_POINT ( 'NONE',  ( 13.58448792996048304, 23.80199789373500963, -14.43409159148844090 ) ) ;
#8225 = CIRCLE ( 'NONE', #3035, 0.5000000000000015543 ) ;
#8226 = CARTESIAN_POINT ( 'NONE',  ( -5.067385705950865571, -26.57793081542402547, 12.73282698324853257 ) ) ;
#8227 = EDGE_LOOP ( 'NONE', ( #22984, #24437, #12555 ) ) ;
#8229 = AXIS2_PLACEMENT_3D ( 'NONE', #28619, #3836, #16237 ) ;
#8228 = CARTESIAN_POINT ( 'NONE',  ( -14.12254998924808191, 16.91766681099430869, -21.95434448082308521 ) ) ;
#8230 = CARTESIAN_POINT ( 'NONE',  ( -24.51396478725073536, -11.15767879383071737, 20.99999999999999645 ) ) ;
#8231 = DIRECTION ( 'NONE',  ( -0.000000000000000000, -0.000000000000000000, -1.000000000000000000 ) ) ;
#8232 = CARTESIAN_POINT ( 'NONE',  ( 11.31505853063862688, 18.03411298331075940, -25.01525395742355329 ) ) ;
#8233 = EDGE_LOOP ( 'NONE', ( #37688, #35872, #22461, #22940, #21321, #26863, #13635 ) ) ;
#8234 = CARTESIAN_POINT ( 'NONE',  ( 13.20924685295718248, 22.23599012058754099, -16.44404666642639867 ) ) ;
#8235 = EDGE_LOOP ( 'NONE', ( #12441, #18947 ) ) ;
#8237 = FACE_OUTER_BOUND ( 'NONE', #18181, .T. ) ;
#8236 = CARTESIAN_POINT ( 'NONE',  ( -10.92267213224567968, 17.34778819946280493, -29.99999999999998934 ) ) ;
#8238 = CARTESIAN_POINT ( 'NONE',  ( -15.55120232977052552, -26.73296669180702878, -5.945196455431404736 ) ) ;
#8239 = CARTESIAN_POINT ( 'NONE',  ( -31.34430980808800626, -24.70897660846286570, 12.14047268033097282 ) ) ;
#8240 = CARTESIAN_POINT ( 'NONE',  ( -23.40264495275803469, -13.17898732060409372, -18.60987684574479673 ) ) ;
#8241 = CARTESIAN_POINT ( 'NONE',  ( -9.241023740148470722, -25.33547218322737038, -6.910767586270462282 ) ) ;
#8242 = DIRECTION ( 'NONE',  ( 0.6691306063588671194, 0.7431448254773863615, -0.000000000000000000 ) ) ;
#8243 = CARTESIAN_POINT ( 'NONE',  ( 13.92769306801763207, 21.97374865699145019, -15.51183746870685809 ) ) ;
#8244 = ORIENTED_EDGE ( 'NONE', *, *, #24642, .F. ) ;
#8245 = CARTESIAN_POINT ( 'NONE',  ( 24.57025407321291510, 7.375674204439781612, -6.926099335226528098 ) ) ;
#8246 = CARTESIAN_POINT ( 'NONE',  ( 15.48853125999101898, -26.74269726803731828, -5.000000000000000000 ) ) ;
#8247 = CARTESIAN_POINT ( 'NONE',  ( 6.151085731882511176, 35.08626808545850650, 7.500000000000000000 ) ) ;
#8248 = CARTESIAN_POINT ( 'NONE',  ( -9.356056665764020508, 26.06569820189716324, 10.50000000000000533 ) ) ;
#8249 = ORIENTED_EDGE ( 'NONE', *, *, #20447, .F. ) ;
#8250 = CARTESIAN_POINT ( 'NONE',  ( -31.84661580973198625, -1.628238131297263358, -7.766091669641889794 ) ) ;
#8251 = CARTESIAN_POINT ( 'NONE',  ( 29.73426277082694114, -0.1029795250634506915, -10.16860317180123374 ) ) ;
#8252 = DIRECTION ( 'NONE',  ( 1.000000000000000000, 0.000000000000000000, 0.000000000000000000 ) ) ;
#8253 = CARTESIAN_POINT ( 'NONE',  ( 21.72603204741341898, -16.58852365944996166, 20.99999999999999645 ) ) ;
#8254 = DIRECTION ( 'NONE',  ( -0.000000000000000000, -0.000000000000000000, 1.000000000000000000 ) ) ;
#8255 = ADVANCED_FACE ( 'NONE', ( #17216 ), #29590, .T. ) ;
#8256 = FILL_AREA_STYLE ('',( #23496 ) ) ;
#8257 = PLANE ( 'NONE',  #6940 ) ;
#8258 = AXIS2_PLACEMENT_3D ( 'NONE', #21779, #256, #25032 ) ;
#8259 = CIRCLE ( 'NONE', #12149, 17.99999999999993250 ) ;
#8260 = ORIENTED_EDGE ( 'NONE', *, *, #10994, .T. ) ;
#8261 = CARTESIAN_POINT ( 'NONE',  ( 14.99496371230769931, 22.09054546458561674, 7.203056206335837430 ) ) ;
#8262 = AXIS2_PLACEMENT_3D ( 'NONE', #24137, #8905, #15997 ) ;
#8263 = VECTOR ( 'NONE', #32000, 1000.000000000000000 ) ;
#8264 = CARTESIAN_POINT ( 'NONE',  ( 6.807850151676529293, 35.76876263333484474, 10.49999999999999822 ) ) ;
#8265 = LINE ( 'NONE', #29803, #24851 ) ;
#8266 = CARTESIAN_POINT ( 'NONE',  ( 0.4001783121710071889, 37.17016172131723550, -8.843365538038478135 ) ) ;
#8267 = DIRECTION ( 'NONE',  ( -0.2876062384759483503, -0.6459741880212440668, 0.7071067811865547892 ) ) ;
#8268 = EDGE_CURVE ( 'NONE', #29799, #16943, #8053, .T. ) ;
#8269 = DIRECTION ( 'NONE',  ( 1.000000000000000000, 0.000000000000000000, 0.000000000000000000 ) ) ;
#8270 = DIRECTION ( 'NONE',  ( 0.5720614028176917998, 0.4156269377774556295, 0.7071067811865402453 ) ) ;
#8271 = DIRECTION ( 'NONE',  ( 0.000000000000000000, 0.000000000000000000, 1.000000000000000000 ) ) ;
#8273 = EDGE_CURVE ( 'NONE', #9944, #4851, #28203, .T. ) ;
#8272 = CARTESIAN_POINT ( 'NONE',  ( 12.30736835487432757, 14.81698729810772441, 7.499999999999997335 ) ) ;
#8274 = CARTESIAN_POINT ( 'NONE',  ( 3.118671991557230516, 37.17221401100731981, 13.00000000000000178 ) ) ;
#8275 = CARTESIAN_POINT ( 'NONE',  ( 13.79182622341905962, 26.77182061978390237, -11.47104827624631262 ) ) ;
#8276 = FACE_OUTER_BOUND ( 'NONE', #20752, .T. ) ;
#8277 = ORIENTED_EDGE ( 'NONE', *, *, #2242, .T. ) ;
#8279 = DIRECTION ( 'NONE',  ( 1.000000000000000000, 0.000000000000000000, 0.000000000000000000 ) ) ;
#8278 = CARTESIAN_POINT ( 'NONE',  ( -16.38814671032943693, 12.36958133795433135, -28.85484690269119668 ) ) ;
#8280 = EDGE_CURVE ( 'NONE', #24136, #11401, #3464, .T. ) ;
#8281 = CARTESIAN_POINT ( 'NONE',  ( -14.11133924723977628, 27.61078317377193159, 10.49999999999999822 ) ) ;
#8282 = CARTESIAN_POINT ( 'NONE',  ( 14.37655681973246402, -25.07404765674405667, -11.59782526845664918 ) ) ;
#8283 = EDGE_CURVE ( 'NONE', #21540, #23024, #34584, .T. ) ;
#8284 = CARTESIAN_POINT ( 'NONE',  ( -14.11133924723978517, 27.61078317377194580, 10.63089969389956835 ) ) ;
#8285 = CARTESIAN_POINT ( 'NONE',  ( 14.01431933016365150, 23.97271075189374656, -13.50973434947982099 ) ) ;
#8286 = LINE ( 'NONE', #5240, #2357 ) ;
#8287 = CARTESIAN_POINT ( 'NONE',  ( 25.22779561345564758, -30.53001674459726189, 11.00000000000000178 ) ) ;
#8288 = AXIS2_PLACEMENT_3D ( 'NONE', #22980, #25622, #38021 ) ;
#8289 = CIRCLE ( 'NONE', #26465, 0.5000000000000004441 ) ;
#8290 = CARTESIAN_POINT ( 'NONE',  ( -21.37336528869494146, -18.93283188275981743, -16.72296912899527399 ) ) ;
#8291 = CARTESIAN_POINT ( 'NONE',  ( 3.641758806176171870, -23.49846102025998817, -13.88050724111706913 ) ) ;
#8292 = CARTESIAN_POINT ( 'NONE',  ( 11.35670081024726663, 17.63068499975756964, -26.24312638122347607 ) ) ;
#8293 = CARTESIAN_POINT ( 'NONE',  ( 19.13565567046500959, 11.72986290071136217, -18.01978235670257789 ) ) ;
#8294 = CARTESIAN_POINT ( 'NONE',  ( 6.330070799514983193, 27.28854476845134513, 6.000000000000000000 ) ) ;
#8295 = B_SPLINE_CURVE_WITH_KNOTS ( 'NONE', 3,
 ( #22171, #21771, #45, #16283, #448, #9985 ),
 .UNSPECIFIED., .F., .F.,
 ( 4, 2, 4 ),
 ( 0.000000000000000000, 0.5000000000000000000, 1.000000000000000000 ),
 .UNSPECIFIED. ) ;
#8296 = VERTEX_POINT ( 'NONE', #19063 ) ;
#8297 = CARTESIAN_POINT ( 'NONE',  ( -4.675295383163502017, 19.96902330696676131, -29.99999999999998579 ) ) ;
#8298 = CIRCLE ( 'NONE', #10878, 1.000000000000004441 ) ;
#8299 = ORIENTED_EDGE ( 'NONE', *, *, #16305, .F. ) ;
#8300 = B_SPLINE_CURVE_WITH_KNOTS ( 'NONE', 3,
 ( #26737, #24484, #5801, #29985, #36292, #33253 ),
 .UNSPECIFIED., .F., .F.,
 ( 4, 2, 4 ),
 ( 0.000000000000000000, 0.5000000000000000000, 1.000000000000000000 ),
 .UNSPECIFIED. ) ;
#8301 = CIRCLE ( 'NONE', #31002, 0.5000000000000004441 ) ;
#8302 = APPLICATION_CONTEXT ( 'automotive_design' ) ;
#8303 = CARTESIAN_POINT ( 'NONE',  ( -11.14717575287011542, 32.53695909538323860, 12.00000000000000000 ) ) ;
#8304 = ORIENTED_EDGE ( 'NONE', *, *, #1407, .T. ) ;
#8305 = EDGE_CURVE ( 'NONE', #13116, #34935, #14486, .T. ) ;
#8306 = FACE_OUTER_BOUND ( 'NONE', #3245, .T. ) ;
#8307 = ADVANCED_FACE ( 'NONE', ( #979 ), #25749, .T. ) ;
#8308 = CARTESIAN_POINT ( 'NONE',  ( 9.426561227484755889, 11.13126706419770073, 10.49999999999999822 ) ) ;
#8309 = EDGE_CURVE ( 'NONE', #37532, #39789, #2173, .T. ) ;
#8310 = ORIENTED_EDGE ( 'NONE', *, *, #2798, .T. ) ;
#8311 = CARTESIAN_POINT ( 'NONE',  ( -22.67633955519294631, 0.7916079257996353480, -21.63973890270278844 ) ) ;
#8312 = ORIENTED_EDGE ( 'NONE', *, *, #13832, .F. ) ;
#8313 = CARTESIAN_POINT ( 'NONE',  ( 19.63120307387857011, -5.935663759831211195, -29.23833046634263511 ) ) ;
#8314 = VERTEX_POINT ( 'NONE', #37948 ) ;
#8315 = DIRECTION ( 'NONE',  ( 0.000000000000000000, 0.000000000000000000, 1.000000000000000000 ) ) ;
#8316 = ORIENTED_EDGE ( 'NONE', *, *, #22087, .T. ) ;
#8317 = DIRECTION ( 'NONE',  ( 0.000000000000000000, 0.000000000000000000, 1.000000000000000000 ) ) ;
#8318 = CARTESIAN_POINT ( 'NONE',  ( 17.34253826607184479, 27.32041144404033162, 11.00000000000000000 ) ) ;
#8319 = VECTOR ( 'NONE', #33506, 1000.000000000000000 ) ;
#8320 = AXIS2_PLACEMENT_3D ( 'NONE', #20197, #4752, #27880 ) ;
#8321 = DIRECTION ( 'NONE',  ( 0.000000000000000000, 0.000000000000000000, 1.000000000000000000 ) ) ;
#8322 = ORIENTED_EDGE ( 'NONE', *, *, #12343, .T. ) ;
#8323 = DIRECTION ( 'NONE',  ( 0.000000000000000000, 0.000000000000000000, 1.000000000000000000 ) ) ;
#8324 = LINE ( 'NONE', #39989, #16303 ) ;
#8325 = AXIS2_PLACEMENT_3D ( 'NONE', #10864, #35650, #7806 ) ;
#8326 = CARTESIAN_POINT ( 'NONE',  ( -2.421689871081829537, 8.701977744317861863, 7.499999999999997335 ) ) ;
#8327 = ADVANCED_FACE ( 'NONE', ( #12763 ), #24958, .F. ) ;
#8328 = CARTESIAN_POINT ( 'NONE',  ( 18.09980013376456398, 17.32878008101015155, -10.83467271882861560 ) ) ;
#8329 = VECTOR ( 'NONE', #23591, 1000.000000000000000 ) ;
#8330 = CARTESIAN_POINT ( 'NONE',  ( 8.579543980086729249, 24.19985443805853720, -18.94540614325930150 ) ) ;
#8331 = EDGE_LOOP ( 'NONE', ( #38796, #35257, #3165, #2657 ) ) ;
#8332 = CARTESIAN_POINT ( 'NONE',  ( -18.81000520956799704, 8.529488778487996470, -27.16704582425938597 ) ) ;
#8333 = CARTESIAN_POINT ( 'NONE',  ( 10.53831209642084943, 32.66155519649334593, 11.00000000000000178 ) ) ;
#8334 = DIRECTION ( 'NONE',  ( 0.000000000000000000, 0.000000000000000000, 1.000000000000000000 ) ) ;
#8335 = CARTESIAN_POINT ( 'NONE',  ( 11.36210984317571615, -20.43702075986949040, -20.51812109925986150 ) ) ;
#8336 = FACE_OUTER_BOUND ( 'NONE', #3458, .T. ) ;
#8337 = LINE ( 'NONE', #11584, #17268 ) ;
#8338 = CARTESIAN_POINT ( 'NONE',  ( -11.03706680401473506, 17.42694036731077745, -28.07723557321667585 ) ) ;
#8339 = CARTESIAN_POINT ( 'NONE',  ( -36.37100582830133533, -12.78888441968056000, 15.13084544680203258 ) ) ;
#8340 = CARTESIAN_POINT ( 'NONE',  ( 12.47139895626693828, -24.39478734073985677, -12.60803247688938988 ) ) ;
#8341 = CARTESIAN_POINT ( 'NONE',  ( -9.303655249773276736, 10.73386218874833631, 7.500000000000000888 ) ) ;
#8342 = ORIENTED_EDGE ( 'NONE', *, *, #24492, .F. ) ;
#8343 = ORIENTED_EDGE ( 'NONE', *, *, #20256, .F. ) ;
#8344 = CARTESIAN_POINT ( 'NONE',  ( -9.986907921862322013, 27.50688179610501294, -14.99363465816162666 ) ) ;
#8345 = PLANE ( 'NONE',  #9442 ) ;
#8346 = CARTESIAN_POINT ( 'NONE',  ( -12.23768179954928392, 14.31935546172410412, 10.49999999999999822 ) ) ;
#8347 = CIRCLE ( 'NONE', #25212, 15.00000000000000000 ) ;
#8348 = VECTOR ( 'NONE', #32056, 1000.000000000000000 ) ;
#8349 = CARTESIAN_POINT ( 'NONE',  ( -15.02235689379176087, 21.92659494635362449, 10.49999999999999822 ) ) ;
#8350 = ORIENTED_EDGE ( 'NONE', *, *, #30112, .F. ) ;
#8351 = CARTESIAN_POINT ( 'NONE',  ( 20.52348880615194915, 0.9275646289840523417, -28.70940543212687501 ) ) ;
#8352 = DIRECTION ( 'NONE',  ( 0.000000000000000000, 0.000000000000000000, 1.000000000000000000 ) ) ;
#8353 = CYLINDRICAL_SURFACE ( 'NONE', #31711, 0.5000000000000001110 ) ;
#8354 = CARTESIAN_POINT ( 'NONE',  ( -35.04557732017523364, -20.40215588137732894, 10.99999999999994138 ) ) ;
#8355 = EDGE_CURVE ( 'NONE', #2590, #29319, #26168, .T. ) ;
#8356 = AXIS2_PLACEMENT_3D ( 'NONE', #36842, #30153, #5764 ) ;
#8357 = ORIENTED_EDGE ( 'NONE', *, *, #19332, .T. ) ;
#8358 = CARTESIAN_POINT ( 'NONE',  ( -25.20077581846105375, 0.3984468658264971319, -17.44060062697873192 ) ) ;
#8359 = DIRECTION ( 'NONE',  ( 0.000000000000000000, 0.000000000000000000, 1.000000000000000000 ) ) ;
#8360 = EDGE_LOOP ( 'NONE', ( #15103, #27841, #22949 ) ) ;
#8361 = CARTESIAN_POINT ( 'NONE',  ( 33.54902081565550276, -4.132526625222229910, -7.247087903461005176 ) ) ;
#8362 = CARTESIAN_POINT ( 'NONE',  ( 29.43343111547206448, -25.34807889869614073, 14.53008259253982892 ) ) ;
#8363 = ORIENTED_EDGE ( 'NONE', *, *, #17331, .T. ) ;
#8364 = CARTESIAN_POINT ( 'NONE',  ( -3.717128218779113702, 39.34929362537324948, 14.53008259254020551 ) ) ;
#8365 = CARTESIAN_POINT ( 'NONE',  ( 4.276224980513730623E-14, -25.25135431486990711, 15.72805884748939853 ) ) ;
#8366 = DIRECTION ( 'NONE',  ( 0.000000000000000000, 0.000000000000000000, 1.000000000000000000 ) ) ;
#8367 = CARTESIAN_POINT ( 'NONE',  ( 2.905187527479470067, 31.12430299512154264, 20.50957957746028626 ) ) ;
#8368 = DIRECTION ( 'NONE',  ( 0.000000000000000000, 0.000000000000000000, 1.000000000000000000 ) ) ;
#8369 = ORIENTED_EDGE ( 'NONE', *, *, #28043, .F. ) ;
#8370 = CARTESIAN_POINT ( 'NONE',  ( -3.476907992048017260, 18.63850621467409496, 6.000000000000000000 ) ) ;
#8371 = DIRECTION ( 'NONE',  ( 0.1470157664651937091, -0.6916548014802239575, -0.7071067811865501263 ) ) ;
#8372 = EDGE_CURVE ( 'NONE', #37754, #17829, #6352, .T. ) ;
#8373 = VECTOR ( 'NONE', #30438, 1000.000000000000000 ) ;
#8375 = AXIS2_PLACEMENT_3D ( 'NONE', #5233, #14782, #23324 ) ;
#8374 = CARTESIAN_POINT ( 'NONE',  ( 3.888268390277564546, 20.12764833916413210, -30.00000000000000000 ) ) ;
#8376 = CARTESIAN_POINT ( 'NONE',  ( 12.05736835487432579, 14.38397459621550567, 11.00000000000000000 ) ) ;
#8377 = EDGE_CURVE ( 'NONE', #17859, #11555, #21903, .T. ) ;
#8378 = CARTESIAN_POINT ( 'NONE',  ( 11.08993573033173696, 19.63476728479018973, 20.25080042701548777 ) ) ;
#8379 = CARTESIAN_POINT ( 'NONE',  ( 19.58288088771594815, -26.98521917108113399, -7.262093437065574975 ) ) ;
#8380 = DIRECTION ( 'NONE',  ( 1.000000000000000000, 0.000000000000000000, 0.000000000000000000 ) ) ;
#8381 = CIRCLE ( 'NONE', #7055, 1.000000000000000000 ) ;
#8382 = FACE_OUTER_BOUND ( 'NONE', #9118, .T. ) ;
#8383 = CARTESIAN_POINT ( 'NONE',  ( 2.575189371470594235, 7.979819372998081306, 10.94387467463492492 ) ) ;
#8384 = ORIENTED_EDGE ( 'NONE', *, *, #16329, .F. ) ;
#8385 = CARTESIAN_POINT ( 'NONE',  ( 15.12690670045320651, 26.44130067926909788, -8.291666083221429062 ) ) ;
#8386 = ORIENTED_EDGE ( 'NONE', *, *, #8309, .F. ) ;
#8387 = CARTESIAN_POINT ( 'NONE',  ( -15.59869368156687486, 26.13660472685725722, -5.000000000000000000 ) ) ;
#8388 = EDGE_CURVE ( 'NONE', #17187, #37715, #25350, .T. ) ;
#8389 = CARTESIAN_POINT ( 'NONE',  ( -32.48980236688448997, -6.600743665353513201, 18.42518152272148413 ) ) ;
#8390 = CARTESIAN_POINT ( 'NONE',  ( 3.994223993665185546, 8.041403552485290263, 7.382773698552457020 ) ) ;
#8391 = CARTESIAN_POINT ( 'NONE',  ( 11.97503790938721657, 19.29424847012439059, -21.63139525819087439 ) ) ;
#8392 = ORIENTED_EDGE ( 'NONE', *, *, #32277, .T. ) ;
#8393 = CARTESIAN_POINT ( 'NONE',  ( 19.66064036848656826, -11.63052904784041353, -22.98217444469445425 ) ) ;
#8394 = ORIENTED_EDGE ( 'NONE', *, *, #22580, .T. ) ;
#8396 = FACE_OUTER_BOUND ( 'NONE', #33033, .T. ) ;
#8395 = CARTESIAN_POINT ( 'NONE',  ( -10.86333472933958433, 17.98415157847645318, -26.19019042869090086 ) ) ;
#8397 = CARTESIAN_POINT ( 'NONE',  ( -17.29263770120802945, -27.09866115540251030, -4.999999999999999112 ) ) ;
#8398 = CARTESIAN_POINT ( 'NONE',  ( 8.577540944421576441, 33.15743037285414374, 12.00000000000000000 ) ) ;
#8399 = VERTEX_POINT ( 'NONE', #10120 ) ;
#8400 = CARTESIAN_POINT ( 'NONE',  ( -19.17275462598830060, -7.282501898908932958, -30.00000000000000711 ) ) ;
#8401 = CARTESIAN_POINT ( 'NONE',  ( -14.98552525403816027, -26.61491965241963342, -5.474092641348948796 ) ) ;
#8402 = CARTESIAN_POINT ( 'NONE',  ( 0.000000000000000000, 22.50000000000000355, 7.000000000000000000 ) ) ;
#8403 = ORIENTED_EDGE ( 'NONE', *, *, #9769, .F. ) ;
#8404 = CARTESIAN_POINT ( 'NONE',  ( 28.07054727141038697, 2.026488101130145658, -9.749946147146546949 ) ) ;
#8405 = DIRECTION ( 'NONE',  ( -0.000000000000000000, -0.000000000000000000, -1.000000000000000000 ) ) ;
#8406 = CARTESIAN_POINT ( 'NONE',  ( -6.330077540933487512, 17.71145523154927659, 6.000000000000000000 ) ) ;
#8407 = EDGE_CURVE ( 'NONE', #31812, #4123, #11190, .T. ) ;
#8408 = VERTEX_POINT ( 'NONE', #34309 ) ;
#8409 = EDGE_CURVE ( 'NONE', #747, #24654, #28802, .T. ) ;
#8410 = CARTESIAN_POINT ( 'NONE',  ( -20.69840430391611008, 0.7747587285446246863, -27.44368215450492698 ) ) ;
#8412 = EDGE_CURVE ( 'NONE', #13055, #5349, #3621, .T. ) ;
#8411 = ORIENTED_EDGE ( 'NONE', *, *, #36100, .T. ) ;
#8413 = CARTESIAN_POINT ( 'NONE',  ( 20.54837291512225406, 0.2170867354722968989, -28.68434330076379979 ) ) ;
#8414 = CARTESIAN_POINT ( 'NONE',  ( 16.05557028316289347, -24.54483004364954368, 18.42518152272108622 ) ) ;
#8415 = ORIENTED_EDGE ( 'NONE', *, *, #1529, .T. ) ;
#8416 = CARTESIAN_POINT ( 'NONE',  ( -27.64268375266474109, 3.518380400506786909, -5.950924345792210524 ) ) ;
#8417 = DIRECTION ( 'NONE',  ( 0.7431448254773953543, 0.6691306063588570163, 0.000000000000000000 ) ) ;
#8418 = CARTESIAN_POINT ( 'NONE',  ( 14.83020139230451662, 20.24804233373097873, 7.485699520496988946 ) ) ;
#8419 = CARTESIAN_POINT ( 'NONE',  ( -0.2655091840902661926, 8.754836972118123839, 6.000000000000000000 ) ) ;
#8420 = EDGE_CURVE ( 'NONE', #17593, #27237, #33357, .T. ) ;
#8421 = LINE ( 'NONE', #14511, #33130 ) ;
#8422 = CARTESIAN_POINT ( 'NONE',  ( 6.557822374958316658, 35.99981354310111215, 10.49999999999999822 ) ) ;
#8423 = EDGE_CURVE ( 'NONE', #19485, #10298, #9921, .T. ) ;
#8424 = PLANE ( 'NONE',  #12026 ) ;
#8425 = ORIENTED_EDGE ( 'NONE', *, *, #38771, .F. ) ;
#8426 = CARTESIAN_POINT ( 'NONE',  ( -24.98617032440317942, 5.239009436875295300, -11.77689850835809793 ) ) ;
#8427 = FACE_OUTER_BOUND ( 'NONE', #23439, .T. ) ;
#8428 = CARTESIAN_POINT ( 'NONE',  ( -1.838889047819898037, 31.15129278236396360, 7.000000000000000000 ) ) ;
#8429 = CARTESIAN_POINT ( 'NONE',  ( 20.86948450591783555, -20.46856481552917373, -15.82250207514942986 ) ) ;
#8430 = DIRECTION ( 'NONE',  ( 0.000000000000000000, 0.000000000000000000, 1.000000000000000000 ) ) ;
#8431 = CARTESIAN_POINT ( 'NONE',  ( -14.31603901957233660, 19.98981538725089635, 10.49999999999999822 ) ) ;
#8432 = CARTESIAN_POINT ( 'NONE',  ( 15.13840818345982520, 27.03333146816605748, -7.344069862628868073 ) ) ;
#8433 = CARTESIAN_POINT ( 'NONE',  ( -5.050662510305666153, -26.77689918168226058, 11.00000000000000000 ) ) ;
#8434 = AXIS2_PLACEMENT_3D ( 'NONE', #15711, #27903, #18767 ) ;
#8435 = ORIENTED_EDGE ( 'NONE', *, *, #32229, .T. ) ;
#8436 = CARTESIAN_POINT ( 'NONE',  ( -16.52923656195466151, 22.85177225473215756, -6.899933075074482502 ) ) ;
#8437 = CARTESIAN_POINT ( 'NONE',  ( -24.20198940123846398, -6.620595927252818313, 20.94377226548378701 ) ) ;
#8438 = CARTESIAN_POINT ( 'NONE',  ( -0.6108529249776363246, 37.48755679569042343, 7.000000000000000000 ) ) ;
#8439 = CARTESIAN_POINT ( 'NONE',  ( 11.00415319253780488, 17.29620292487934563, -30.00000000000001421 ) ) ;
#8440 = ORIENTED_EDGE ( 'NONE', *, *, #25743, .F. ) ;
#8441 = CARTESIAN_POINT ( 'NONE',  ( -14.97986028244562107, 21.52226669793691727, 10.49999999999999822 ) ) ;
#8442 = AXIS2_PLACEMENT_3D ( 'NONE', #2032, #1832, #27399 ) ;
#8443 = ORIENTED_EDGE ( 'NONE', *, *, #37334, .F. ) ;
#8445 = LINE ( 'NONE', #4790, #1719 ) ;
#8444 = CARTESIAN_POINT ( 'NONE',  ( -13.43406490775605278, 22.93255246805462733, -15.43730422837821159 ) ) ;
#8446 = CARTESIAN_POINT ( 'NONE',  ( -14.43849888084333877, -25.08593691932569314, -11.59330415005311643 ) ) ;
#8447 = DIRECTION ( 'NONE',  ( -0.000000000000000000, -0.000000000000000000, -1.000000000000000000 ) ) ;
#8448 = CARTESIAN_POINT ( 'NONE',  ( -31.87643534942240819, -17.94561782331171784, -9.724772667764392864 ) ) ;
#8449 = CARTESIAN_POINT ( 'NONE',  ( -6.368927712313042555, -20.05147684786715701, -25.34049200730608220 ) ) ;
#8450 = DIRECTION ( 'NONE',  ( 0.000000000000000000, -0.000000000000000000, 1.000000000000000000 ) ) ;
#8451 = CARTESIAN_POINT ( 'NONE',  ( 12.55804699249790168, 17.47949508554678388, -24.00749146857737770 ) ) ;
#8452 = EDGE_LOOP ( 'NONE', ( #24578, #37470 ) ) ;
#8453 = CARTESIAN_POINT ( 'NONE',  ( 19.58333117617996777, 6.632644045549831446, -27.12887243873458942 ) ) ;
#8454 = CARTESIAN_POINT ( 'NONE',  ( -3.724378136954612284, 12.76962061027129458, 12.00000000000000000 ) ) ;
#8455 = CYLINDRICAL_SURFACE ( 'NONE', #19915, 1.000000000000000888 ) ;
#8456 = FACE_OUTER_BOUND ( 'NONE', #27339, .T. ) ;
#8457 = EDGE_LOOP ( 'NONE', ( #8343, #33467, #35337, #17984 ) ) ;
#8458 = CARTESIAN_POINT ( 'NONE',  ( -31.33630356776520642, -0.7993948758031136359, -7.330644645363229017 ) ) ;
#8459 = CARTESIAN_POINT ( 'NONE',  ( 20.69783600767029696, 0.7831999650737890839, -27.44422954938529813 ) ) ;
#8460 = CARTESIAN_POINT ( 'NONE',  ( -14.36830325120615548, 20.48707633493503621, 7.500000000000004441 ) ) ;
#8461 = CARTESIAN_POINT ( 'NONE',  ( 22.36336935241927293, -18.10715803802170498, 20.82122704794078771 ) ) ;
#8462 = FACE_OUTER_BOUND ( 'NONE', #18004, .T. ) ;
#8463 = CARTESIAN_POINT ( 'NONE',  ( 22.52744239175980923, -0.1803094636422790109, -20.90349153981001606 ) ) ;
#8464 = DIRECTION ( 'NONE',  ( 1.000000000000000000, 0.000000000000000000, 0.000000000000000000 ) ) ;
#8465 = ORIENTED_EDGE ( 'NONE', *, *, #2639, .F. ) ;
#8466 = B_SPLINE_CURVE_WITH_KNOTS ( 'NONE', 3,
 ( #12712, #28753, #928, #6416, #12913, #3373 ),
 .UNSPECIFIED., .F., .F.,
 ( 4, 2, 4 ),
 ( 0.000000000000000000, 0.3333333331791988874, 0.6666666663583977748 ),
 .UNSPECIFIED. ) ;
#8467 = CONICAL_SURFACE ( 'NONE', #36367, 0.5000000000000069944, 0.7853981633974450594 ) ;
#8468 = CARTESIAN_POINT ( 'NONE',  ( 0.000000000000000000, 22.50000000000000355, 0.000000000000000000 ) ) ;
#8469 = CARTESIAN_POINT ( 'NONE',  ( 6.811226782241717181, 35.33967249274190436, 10.49999999999999822 ) ) ;
#8470 = EDGE_LOOP ( 'NONE', ( #35385, #21278, #37935, #8363 ) ) ;
#8471 = CARTESIAN_POINT ( 'NONE',  ( 0.3940515309154056234, 36.53847938540027229, -9.725803077370580141 ) ) ;
#8472 = DIRECTION ( 'NONE',  ( -0.4731467892558149924, 0.5254827454987555102, 0.7071067811865500152 ) ) ;
#8473 = DIRECTION ( 'NONE',  ( 1.000000000000000000, 0.000000000000000000, 0.000000000000000000 ) ) ;
#8474 = CARTESIAN_POINT ( 'NONE',  ( -19.48557158514988785, -11.24999999999987743, 10.00000000000000000 ) ) ;
#8475 = DIRECTION ( 'NONE',  ( 0.000000000000000000, 0.000000000000000000, 1.000000000000000000 ) ) ;
#8476 = DIRECTION ( 'NONE',  ( 0.5000000000000015543, 0.8660254037844377084, 0.000000000000000000 ) ) ;
#8477 = CARTESIAN_POINT ( 'NONE',  ( -6.811226782241547539, 35.33967249274200384, 10.49999999999999822 ) ) ;
#8478 = CARTESIAN_POINT ( 'NONE',  ( 14.41393829650433211, 27.23447492386241819, -9.633712356753633799 ) ) ;
#8479 = CARTESIAN_POINT ( 'NONE',  ( 12.80736835487433289, 15.68301270189216545, 7.499999999999997335 ) ) ;
#8480 = ORIENTED_EDGE ( 'NONE', *, *, #22198, .F. ) ;
#8481 = VECTOR ( 'NONE', #13146, 1000.000000000000000 ) ;
#8483 = DIRECTION ( 'NONE',  ( 0.000000000000000000, 0.000000000000000000, 1.000000000000000000 ) ) ;
#8482 = CARTESIAN_POINT ( 'NONE',  ( -16.60583435348276282, 13.74075903883709593, -22.18912786978531315 ) ) ;
#8484 = DIRECTION ( 'NONE',  ( 0.6691306063588570163, -0.7431448254773953543, 0.000000000000000000 ) ) ;
#8485 = VECTOR ( 'NONE', #37102, 1000.000000000000000 ) ;
#8486 = CARTESIAN_POINT ( 'NONE',  ( 10.25084136881418573, -19.15538197628319139, -23.85068623870123972 ) ) ;
#8487 = DIRECTION ( 'NONE',  ( 0.000000000000000000, 0.000000000000000000, 1.000000000000000000 ) ) ;
#8488 = CARTESIAN_POINT ( 'NONE',  ( 15.39020460041367855, 26.78288689686343105, -5.945739410967055605 ) ) ;
#8489 = FACE_OUTER_BOUND ( 'NONE', #30174, .T. ) ;
#8490 = CARTESIAN_POINT ( 'NONE',  ( 2.587660364795204782, 9.681887955242936883, 13.00000000000000178 ) ) ;
#8491 = CARTESIAN_POINT ( 'NONE',  ( -29.08184185256072141, -22.79149011935838587, -8.424513042702869825 ) ) ;
#8492 = CARTESIAN_POINT ( 'NONE',  ( 1.817969461173305712, -24.76413945269762351, -5.000000000000001776 ) ) ;
#8493 = CARTESIAN_POINT ( 'NONE',  ( 15.34008105399866828, 26.04368486401110871, -7.829779149383753634 ) ) ;
#8494 = CARTESIAN_POINT ( 'NONE',  ( 18.01512450864053250, 10.08994624255825912, -27.17860653033931939 ) ) ;
#8495 = DIRECTION ( 'NONE',  ( 0.000000000000000000, 0.000000000000000000, 1.000000000000000000 ) ) ;
#8496 = EDGE_LOOP ( 'NONE', ( #35047, #14933, #28934 ) ) ;
#8497 = CIRCLE ( 'NONE', #31194, 1.000000000000000000 ) ;
#8498 = CARTESIAN_POINT ( 'NONE',  ( -4.693749193973906664, 20.04595565361518084, -28.49495074315137799 ) ) ;
#8499 = ORIENTED_EDGE ( 'NONE', *, *, #12564, .F. ) ;
#8500 = CARTESIAN_POINT ( 'NONE',  ( -31.24272016124701068, 0.2902395683534709780, 15.72805884748939853 ) ) ;
#8501 = VERTEX_POINT ( 'NONE', #31851 ) ;
#8502 = CYLINDRICAL_SURFACE ( 'NONE', #1776, 1.000000000000000888 ) ;
#8503 = EDGE_CURVE ( 'NONE', #14734, #39078, #248, .T. ) ;
#8504 = CARTESIAN_POINT ( 'NONE',  ( 9.353067506536371312, 10.78869951827618046, 10.49999999999999822 ) ) ;
#8505 = CARTESIAN_POINT ( 'NONE',  ( -25.74458659788053083, 0.5194498575017915121, -16.46142640285149028 ) ) ;
#8506 = CARTESIAN_POINT ( 'NONE',  ( 25.05526511386589306, -8.388987150351875144, -18.72753401343204160 ) ) ;
#8507 = AXIS2_PLACEMENT_3D ( 'NONE', #7106, #25004, #15462 ) ;
#8508 = EDGE_CURVE ( 'NONE', #24105, #26292, #36588, .T. ) ;
#8509 = VECTOR ( 'NONE', #13244, 1000.000000000000000 ) ;
#8510 = VERTEX_POINT ( 'NONE', #23513 ) ;
#8511 = DIRECTION ( 'NONE',  ( -0.5000000000000038858, -0.8660254037844364872, 0.000000000000000000 ) ) ;
#8512 = ORIENTED_EDGE ( 'NONE', *, *, #35460, .T. ) ;
#8513 = EDGE_CURVE ( 'NONE', #16864, #20155, #13628, .T. ) ;
#8514 = DIRECTION ( 'NONE',  ( -1.000000000000000000, 0.000000000000000000, 0.000000000000000000 ) ) ;
#8515 = CARTESIAN_POINT ( 'NONE',  ( -9.427394655428429360, 11.06314620770957013, 11.00000000000000000 ) ) ;
#8516 = CARTESIAN_POINT ( 'NONE',  ( -11.94134295108998600, 16.18301270189233776, 9.500000000000000000 ) ) ;
#8517 = ORIENTED_EDGE ( 'NONE', *, *, #33999, .T. ) ;
#8518 = LINE ( 'NONE', #24358, #2292 ) ;
#8519 = DIRECTION ( 'NONE',  ( -0.7431448254773953543, -0.6691306063588570163, 0.000000000000000000 ) ) ;
#8520 = TOROIDAL_SURFACE ( 'NONE', #33187, 1.000000000000000000, 0.5000000000000000000 ) ;
#8521 = LINE ( 'NONE', #8326, #55 ) ;
#8522 = CARTESIAN_POINT ( 'NONE',  ( 18.90535999708258075, 15.28347868722541669, -11.85787095818008297 ) ) ;
#8523 = CARTESIAN_POINT ( 'NONE',  ( 11.20956939700582211, 31.79909661247546637, -9.876575786099936138 ) ) ;
#8524 = VERTEX_POINT ( 'NONE', #26565 ) ;
#8525 = CARTESIAN_POINT ( 'NONE',  ( -20.61860813537857240, 9.113149517100110231, -17.99812580813538432 ) ) ;
#8526 = LINE ( 'NONE', #20733, #19670 ) ;
#8527 = CARTESIAN_POINT ( 'NONE',  ( -7.659620408498105881, 26.92228390473685096, 7.000000000000000000 ) ) ;
#8528 = EDGE_CURVE ( 'NONE', #16847, #14003, #7361, .T. ) ;
#8529 = EDGE_CURVE ( 'NONE', #32217, #19954, #26359, .T. ) ;
#8530 = CARTESIAN_POINT ( 'NONE',  ( 9.922609748437189126, -18.19104734674453994, -27.42597713094579248 ) ) ;
#8531 = CARTESIAN_POINT ( 'NONE',  ( -13.14827996435949053, 25.72067290776677950, 10.50000000000000000 ) ) ;
#8532 = CARTESIAN_POINT ( 'NONE',  ( 21.88444403592372112, 6.126538576424477966, -21.50719306941230613 ) ) ;
#8533 = CARTESIAN_POINT ( 'NONE',  ( -13.76553621605945210, 23.40493025121552506, -14.47534936899553948 ) ) ;
#8534 = AXIS2_PLACEMENT_3D ( 'NONE', #32518, #22951, #13406 ) ;
#8535 = CARTESIAN_POINT ( 'NONE',  ( -13.33966701959958456, -16.00384814976887426, -27.17537271300066237 ) ) ;
#8536 = CARTESIAN_POINT ( 'NONE',  ( 13.73668809508641608, -25.59735168978018294, -9.726329721036846010 ) ) ;
#8537 = DIRECTION ( 'NONE',  ( -1.000000000000000000, 0.000000000000000000, 0.000000000000000000 ) ) ;
#8538 = ORIENTED_EDGE ( 'NONE', *, *, #19001, .T. ) ;
#8539 = ORIENTED_EDGE ( 'NONE', *, *, #28099, .T. ) ;
#8540 = B_SPLINE_CURVE_WITH_KNOTS ( 'NONE', 3,
 ( #13416, #435, #31508, #25810, #38205, #32109, #10377, #4274, #10779, #4876, #36366, #32926, #14020, #29860, #1638, #5280, #20328, #16884 ),
 .UNSPECIFIED., .F., .F.,
 ( 4, 2, 2, 2, 2, 2, 2, 2, 4 ),
 ( 0.000000000000000000, 0.1250000000000000000, 0.2500000000000000000, 0.3750000000000000000, 0.5000000000000000000, 0.6250000000000000000, 0.7500000000000000000, 0.8750000000000000000, 1.000000000000000000 ),
 .UNSPECIFIED. ) ;
#8541 = CARTESIAN_POINT ( 'NONE',  ( -11.89071426873642778, 33.14490429473632105, -5.891362697687537953 ) ) ;
#8542 = CARTESIAN_POINT ( 'NONE',  ( 12.39463915635820612, 18.33192650902018883, 6.000000000000000000 ) ) ;
#8543 = CARTESIAN_POINT ( 'NONE',  ( -12.05736835487443059, 14.38397459621567087, 10.49999999999999822 ) ) ;
#8544 = DIRECTION ( 'NONE',  ( 0.1045284632676559550, 0.9945218953682730678, 0.000000000000000000 ) ) ;
#8545 = EDGE_LOOP ( 'NONE', ( #15980, #6196, #4006, #35706 ) ) ;
#8546 = CARTESIAN_POINT ( 'NONE',  ( 29.28231774309053748, 0.1570984678961929726, -10.65577805818864121 ) ) ;
#8547 = CARTESIAN_POINT ( 'NONE',  ( 10.44103466624280685, 32.57396620494213124, 7.000000000000000000 ) ) ;
#8548 = CIRCLE ( 'NONE', #26049, 1.000000000000000888 ) ;
#8549 = DIRECTION ( 'NONE',  ( 1.000000000000000000, 0.000000000000000000, 0.000000000000000000 ) ) ;
#8550 = VERTEX_POINT ( 'NONE', #35508 ) ;
#8551 = CARTESIAN_POINT ( 'NONE',  ( -24.55370900864287975, 0.4434148628449753882, -18.45356317131482982 ) ) ;
#8552 = EDGE_CURVE ( 'NONE', #33546, #16724, #39148, .T. ) ;
#8553 = FACE_OUTER_BOUND ( 'NONE', #30194, .T. ) ;
#8554 = VERTEX_POINT ( 'NONE', #13561 ) ;
#8555 = CARTESIAN_POINT ( 'NONE',  ( 34.73099849614892065, -6.268898363069737911, -5.000000000000007994 ) ) ;
#8556 = CARTESIAN_POINT ( 'NONE',  ( 35.54328883424830110, -18.34041411986698478, 13.92931973827811909 ) ) ;
#8557 = ORIENTED_EDGE ( 'NONE', *, *, #29266, .T. ) ;
#8558 = CARTESIAN_POINT ( 'NONE',  ( -1.387327393066717074E-13, 39.65430245495500117, 14.53008259254011136 ) ) ;
#8559 = DIRECTION ( 'NONE',  ( 1.224646799147353207E-16, 1.000000000000000000, -0.000000000000000000 ) ) ;
#8560 = CARTESIAN_POINT ( 'NONE',  ( 12.30736835487432579, 14.81698729810772619, 9.000000000000001776 ) ) ;
#8561 = CARTESIAN_POINT ( 'NONE',  ( -1.971557875515829616, 31.43880600153361371, 20.50957957746028271 ) ) ;
#8562 = DIRECTION ( 'NONE',  ( 1.000000000000000000, 0.000000000000000000, 0.000000000000000000 ) ) ;
#8563 = VERTEX_POINT ( 'NONE', #11330 ) ;
#8564 = DIRECTION ( 'NONE',  ( -0.9781476007338067991, -0.2079116908177533474, 0.000000000000000000 ) ) ;
#8565 = LINE ( 'NONE', #36210, #9810 ) ;
#8566 = CARTESIAN_POINT ( 'NONE',  ( 6.086784706011969526, 31.15961814524406037, -13.87178128487113327 ) ) ;
#8567 = DIRECTION ( 'NONE',  ( 0.000000000000000000, 0.000000000000000000, 1.000000000000000000 ) ) ;
#8568 = CARTESIAN_POINT ( 'NONE',  ( 24.79273775960175996, -6.040746354374877392, 20.82122704794079837 ) ) ;
#8569 = CIRCLE ( 'NONE', #5990, 1.000000000000000000 ) ;
#8570 = ADVANCED_FACE ( 'NONE', ( #32672 ), #29810, .F. ) ;
#8571 = CARTESIAN_POINT ( 'NONE',  ( 11.74422086145278499, -16.80344316252863734, -29.30034920398468046 ) ) ;
#8572 = DIRECTION ( 'NONE',  ( -0.4067366430757889395, 0.9135454576426059736, 0.000000000000000000 ) ) ;
#8573 = DIRECTION ( 'NONE',  ( -0.8064441531181035794, 0.1277282058446102819, 0.5773502691896329475 ) ) ;
#8574 = FACE_OUTER_BOUND ( 'NONE', #9955, .T. ) ;
#8575 = VERTEX_POINT ( 'NONE', #16827 ) ;
#8576 = CARTESIAN_POINT ( 'NONE',  ( 14.69914344428350539, 25.51220288795486368, -10.64560462785820327 ) ) ;
#8577 = ORIENTED_EDGE ( 'NONE', *, *, #26018, .T. ) ;
#8578 = CARTESIAN_POINT ( 'NONE',  ( -15.27513262873028665, 25.94661827369742113, -8.300200833134605105 ) ) ;
#8579 = AXIS2_PLACEMENT_3D ( 'NONE', #9940, #6479, #37571 ) ;
#8580 = CARTESIAN_POINT ( 'NONE',  ( -29.77271197308770212, -3.128983846831010496, 18.87996532025785967 ) ) ;
#8581 = CIRCLE ( 'NONE', #808, 1.000000000000000000 ) ;
#8582 = CARTESIAN_POINT ( 'NONE',  ( -3.987511920225224937, 8.280017797930396384, 10.49999999999999822 ) ) ;
#8583 = CARTESIAN_POINT ( 'NONE',  ( 11.76965676669902727, 18.83126597396366009, -22.74873947259427709 ) ) ;
#8584 = ORIENTED_EDGE ( 'NONE', *, *, #11565, .F. ) ;
#8585 = CARTESIAN_POINT ( 'NONE',  ( 18.00492286382134566, -10.65055271466412812, -26.96479788887356221 ) ) ;
#8586 = EDGE_LOOP ( 'NONE', ( #11516, #18612, #24429 ) ) ;
#8588 = DIRECTION ( 'NONE',  ( -0.3090169943749573322, -0.9510565162951505336, 0.000000000000000000 ) ) ;
#8587 = CARTESIAN_POINT ( 'NONE',  ( -15.19527047305266443, 27.50996873332976378, -5.000000000000001776 ) ) ;
#8589 = CARTESIAN_POINT ( 'NONE',  ( -16.60262275586455161, -24.86345949671113331, -12.36567362711010354 ) ) ;
#8590 = CARTESIAN_POINT ( 'NONE',  ( 8.927394655428274817, 11.06314620770945290, 7.000000000000000000 ) ) ;
#8591 = ORIENTED_EDGE ( 'NONE', *, *, #38128, .F. ) ;
#8592 = CARTESIAN_POINT ( 'NONE',  ( -34.03066577109931501, -11.68171929586705815, -9.322546398942927581 ) ) ;
#8593 = UNCERTAINTY_MEASURE_WITH_UNIT (LENGTH_MEASURE( 1.000000000000000082E-05 ), #11767, 'distance_accuracy_value', 'NONE');
#8594 = CARTESIAN_POINT ( 'NONE',  ( -9.947661678533670226, -19.26027892739813652, -23.88733551178417613 ) ) ;
#8595 = CIRCLE ( 'NONE', #26747, 1.000000000000000888 ) ;
#8596 = CARTESIAN_POINT ( 'NONE',  ( 24.49409870379991716, -11.70597971641860191, 23.00000000000000000 ) ) ;
#8597 = ORIENTED_EDGE ( 'NONE', *, *, #9116, .T. ) ;
#8598 = CARTESIAN_POINT ( 'NONE',  ( 21.57580026240890447, 3.046887179118514588, -22.98849545702982766 ) ) ;
#8599 = B_SPLINE_CURVE_WITH_KNOTS ( 'NONE', 3,
 ( #37641, #6348, #3904, #15904, #7147 ),
 .UNSPECIFIED., .F., .F.,
 ( 4, 1, 4 ),
 ( 0.000000000000000000, 0.1250000000212990459, 0.1282122296533009798 ),
 .UNSPECIFIED. ) ;
#8600 = CARTESIAN_POINT ( 'NONE',  ( 8.118377661053324701, 10.47536095541698486, 7.000000000000000000 ) ) ;
#8601 = DIRECTION ( 'NONE',  ( 1.000000000000000000, 0.000000000000000000, 0.000000000000000000 ) ) ;
#8602 = ORIENTED_EDGE ( 'NONE', *, *, #8152, .F. ) ;
#8603 = CARTESIAN_POINT ( 'NONE',  ( -27.79845905001932849, 0.1112929649325302972, -13.50539263835538506 ) ) ;
#8604 = EDGE_CURVE ( 'NONE', #31324, #15244, #27475, .T. ) ;
#8605 = ORIENTED_EDGE ( 'NONE', *, *, #14748, .T. ) ;
#8606 = CARTESIAN_POINT ( 'NONE',  ( 20.64185622598208170, 0.04121980942568206213, -28.03684029888757578 ) ) ;
#8607 = CARTESIAN_POINT ( 'NONE',  ( 22.18734415243709179, -26.07761308992911964, 17.42190598798388379 ) ) ;
#8608 = ORIENTED_EDGE ( 'NONE', *, *, #32251, .T. ) ;
#8609 = AXIS2_PLACEMENT_3D ( 'NONE', #36469, #14934, #27322 ) ;
#8610 = EDGE_CURVE ( 'NONE', #22293, #19810, #22302, .T. ) ;
#8611 = CARTESIAN_POINT ( 'NONE',  ( -20.33969889556806265, 2.904538857774676686, -28.77042324836267895 ) ) ;
#8612 = CYLINDRICAL_SURFACE ( 'NONE', #5765, 17.00000000000000000 ) ;
#8613 = DIRECTION ( 'NONE',  ( -0.8660254037844431485, -0.4999999999999921729, 0.000000000000000000 ) ) ;
#8614 = ADVANCED_FACE ( 'NONE', ( #38752 ), #16624, .F. ) ;
#8615 = AXIS2_PLACEMENT_3D ( 'NONE', #18741, #18542, #39671 ) ;
#8616 = CARTESIAN_POINT ( 'NONE',  ( 3.835130509701798918, 15.55077355964573904, 12.00000000000000000 ) ) ;
#8617 = CARTESIAN_POINT ( 'NONE',  ( -14.97009266215794554, 21.42933399866948463, 10.50000000000000000 ) ) ;
#8618 = SHAPE_REPRESENTATION ( 'Detachable Washable Trimmer Head Cap', ( #24238 ), #9333 ) ;
#8619 = CARTESIAN_POINT ( 'NONE',  ( -11.61999097910615930, 31.98625350855128247, 7.479114585244767355 ) ) ;
#8620 = FACE_OUTER_BOUND ( 'NONE', #22417, .T. ) ;
#8621 = ORIENTED_EDGE ( 'NONE', *, *, #17470, .T. ) ;
#8622 = CARTESIAN_POINT ( 'NONE',  ( -20.18459099282218006, 5.011188685773205975, -26.50361906614367058 ) ) ;
#8623 = DIRECTION ( 'NONE',  ( -1.000000000000000000, 0.000000000000000000, 0.000000000000000000 ) ) ;
#8624 = DIRECTION ( 'NONE',  ( -0.000000000000000000, -0.000000000000000000, -1.000000000000000000 ) ) ;
#8625 = CARTESIAN_POINT ( 'NONE',  ( 24.39459500260992542, -25.35271717551619020, -8.931748512371612492 ) ) ;
#8626 = EDGE_CURVE ( 'NONE', #40197, #21179, #29208, .T. ) ;
#8627 = CARTESIAN_POINT ( 'NONE',  ( 18.23649648353767461, -16.09146789626181118, 23.00000000000000000 ) ) ;
#8628 = EDGE_CURVE ( 'NONE', #38824, #31959, #7866, .T. ) ;
#8629 = CARTESIAN_POINT ( 'NONE',  ( 15.30309001416959802, 27.17055420720160441, -5.472318710501133943 ) ) ;
#8630 = VECTOR ( 'NONE', #25807, 1000.000000000000000 ) ;
#8631 = CARTESIAN_POINT ( 'NONE',  ( -15.03860650580051761, -28.48662463501835163, 12.73282698324853257 ) ) ;
#8632 = ORIENTED_EDGE ( 'NONE', *, *, #17283, .T. ) ;
#8633 = CARTESIAN_POINT ( 'NONE',  ( -13.81191689907480047, 17.90740787171185389, -20.81067546043863103 ) ) ;
#8634 = CARTESIAN_POINT ( 'NONE',  ( -25.82310832280115775, -13.25591304976905427, 20.94377226548378346 ) ) ;
#8635 = DIRECTION ( 'NONE',  ( 1.000000000000000000, 0.000000000000000000, 0.000000000000000000 ) ) ;
#8636 = CARTESIAN_POINT ( 'NONE',  ( 15.41225152681027311, 26.70409590730232452, -5.946085469612699015 ) ) ;
#8637 = ORIENTED_EDGE ( 'NONE', *, *, #18062, .F. ) ;
#8638 = CYLINDRICAL_SURFACE ( 'NONE', #5359, 0.5000000000000004441 ) ;
#8639 = ORIENTED_EDGE ( 'NONE', *, *, #30031, .T. ) ;
#8641 = DIRECTION ( 'NONE',  ( 0.7032331762534055342, 0.07391278520357008608, -0.7071067811865457964 ) ) ;
#8640 = CARTESIAN_POINT ( 'NONE',  ( -15.29484476591128228, 26.76856196483461048, -6.884705497639315830 ) ) ;
#8642 = CARTESIAN_POINT ( 'NONE',  ( -10.02177213464359617, -18.79137684907821537, -25.00808960492178912 ) ) ;
#8643 = CARTESIAN_POINT ( 'NONE',  ( 9.221287281574507944, 10.65863771052197606, 10.63089969389957190 ) ) ;
#8644 = AXIS2_PLACEMENT_3D ( 'NONE', #25587, #31889, #12800 ) ;
#8645 = CARTESIAN_POINT ( 'NONE',  ( -18.68643025256734447, -10.52603743360108268, -25.57491845876295500 ) ) ;
#8646 = CARTESIAN_POINT ( 'NONE',  ( -11.46238439996275638, -22.55099105456122999, -16.53223957159231716 ) ) ;
#8647 = CARTESIAN_POINT ( 'NONE',  ( -18.76090689389219435, -16.22676322417297357, 21.00000000000000000 ) ) ;
#8648 = CARTESIAN_POINT ( 'NONE',  ( 15.75550723163302713, 23.75836650642312975, -9.268051056800263865 ) ) ;
#8649 = ORIENTED_EDGE ( 'NONE', *, *, #15507, .F. ) ;
#8650 = CARTESIAN_POINT ( 'NONE',  ( 21.17479613538668914, 6.043406367430672610, -21.04370527317109918 ) ) ;
#8651 = LINE ( 'NONE', #21045, #10911 ) ;
#8652 = FACE_OUTER_BOUND ( 'NONE', #308, .T. ) ;
#8653 = DIRECTION ( 'NONE',  ( 0.9781476007338042455, -0.2079116908177664758, 0.000000000000000000 ) ) ;
#8654 = ORIENTED_EDGE ( 'NONE', *, *, #7559, .F. ) ;
#8655 = CARTESIAN_POINT ( 'NONE',  ( -31.44678074335321938, -0.8094497182387121459, -6.866296305381922593 ) ) ;
#8656 = ADVANCED_FACE ( 'NONE', ( #7461 ), #1379, .T. ) ;
#8657 = AXIS2_PLACEMENT_3D ( 'NONE', #328, #37300, #33673 ) ;
#8658 = CARTESIAN_POINT ( 'NONE',  ( 29.02264181254402686, -0.05255188267202027391, -11.58473844147850684 ) ) ;
#8659 = DIRECTION ( 'NONE',  ( 0.000000000000000000, 0.000000000000000000, 1.000000000000000000 ) ) ;
#8660 = VECTOR ( 'NONE', #5817, 1000.000000000000114 ) ;
#8661 = EDGE_CURVE ( 'NONE', #12475, #9569, #3489, .T. ) ;
#8662 = CARTESIAN_POINT ( 'NONE',  ( 25.03753813966995168, -13.00734255224419655, 20.99999999999999645 ) ) ;
#8663 = CARTESIAN_POINT ( 'NONE',  ( 16.24796006241085422, 15.88921519459651144, -21.50719306941225639 ) ) ;
#8664 = CARTESIAN_POINT ( 'NONE',  ( 34.83525826321753271, -1.648928274806267025, 10.99999999999992006 ) ) ;
#8665 = EDGE_CURVE ( 'NONE', #5003, #4736, #23599, .T. ) ;
#8666 =( GEOMETRIC_REPRESENTATION_CONTEXT ( 3 ) GLOBAL_UNCERTAINTY_ASSIGNED_CONTEXT ( ( #26635 ) ) GLOBAL_UNIT_ASSIGNED_CONTEXT ( ( #35352, #16873, #10167 ) ) REPRESENTATION_CONTEXT ( 'NONE', 'WORKASPACE' ) );
#8667 = ORIENTED_EDGE ( 'NONE', *, *, #38159, .T. ) ;
#8668 = CARTESIAN_POINT ( 'NONE',  ( -15.00000000000000000, 22.50000000000000355, 7.000000000000000000 ) ) ;
#8669 = AXIS2_PLACEMENT_3D ( 'NONE', #6453, #19051, #7046 ) ;
#8670 = DIRECTION ( 'NONE',  ( 1.000000000000000000, 0.000000000000000000, 0.000000000000000000 ) ) ;
#8671 = VERTEX_POINT ( 'NONE', #20271 ) ;
#8672 = CARTESIAN_POINT ( 'NONE',  ( 1.558973647184125122, 37.87412607290816169, -7.545089284928025108 ) ) ;
#8673 = CARTESIAN_POINT ( 'NONE',  ( -4.984135866956331817, 36.15314577889358105, 10.50000000000000533 ) ) ;
#8674 = DIRECTION ( 'NONE',  ( 1.000000000000000000, 0.000000000000000000, 0.000000000000000000 ) ) ;
#8675 = CARTESIAN_POINT ( 'NONE',  ( -14.01838097023000707, 23.73363068877903359, 12.00000000000000000 ) ) ;
#8676 = EDGE_CURVE ( 'NONE', #4778, #30884, #19064, .T. ) ;
#8677 = DIRECTION ( 'NONE',  ( 1.000000000000000000, 0.000000000000000000, 0.000000000000000000 ) ) ;
#8678 = DIRECTION ( 'NONE',  ( 1.000000000000000000, 0.000000000000000000, 0.000000000000000000 ) ) ;
#8679 = DIRECTION ( 'NONE',  ( 0.000000000000000000, 0.000000000000000000, 1.000000000000000000 ) ) ;
#8680 = EDGE_CURVE ( 'NONE', #16522, #24243, #14510, .T. ) ;
#8681 = CARTESIAN_POINT ( 'NONE',  ( 14.31634612938960593, 27.02271693021451782, -10.09916008547401489 ) ) ;
#8682 = LINE ( 'NONE', #15171, #30155 ) ;
#8683 = ORIENTED_EDGE ( 'NONE', *, *, #115, .F. ) ;
#8685 = DIRECTION ( 'NONE',  ( 0.000000000000000000, 0.000000000000000000, 1.000000000000000000 ) ) ;
#8684 = CARTESIAN_POINT ( 'NONE',  ( -18.97573237204982277, 16.39359448400360009, -8.880896986686993344 ) ) ;
#8686 = VECTOR ( 'NONE', #5125, 1000.000000000000114 ) ;
#8687 = CARTESIAN_POINT ( 'NONE',  ( -9.183247089818959097, 16.78440424842446532, 12.00000000000000000 ) ) ;
#8688 = CARTESIAN_POINT ( 'NONE',  ( 11.19426416879276687, -20.46679275895131767, -20.54027932467983319 ) ) ;
#8689 = CARTESIAN_POINT ( 'NONE',  ( 14.02760127444122951, 23.93997290703920910, -13.51284491737118465 ) ) ;
#8690 = CARTESIAN_POINT ( 'NONE',  ( 12.37672620654822175, 20.50964447495777421, -19.49331178464071002 ) ) ;
#8691 = VERTEX_POINT ( 'NONE', #30618 ) ;
#8692 = CARTESIAN_POINT ( 'NONE',  ( 1.693998953219503667, 12.12549434688615513, 10.50000000000000000 ) ) ;
#8693 = CARTESIAN_POINT ( 'NONE',  ( 31.08218588373089020, -27.68808745788718895, 11.00000000000000178 ) ) ;
#8694 = AXIS2_PLACEMENT_3D ( 'NONE', #8477, #2777, #27758 ) ;
#8695 = CARTESIAN_POINT ( 'NONE',  ( -15.77773026942784185, -13.10308996503666101, -30.00000000000001066 ) ) ;
#8696 = CARTESIAN_POINT ( 'NONE',  ( 4.764572365127394349, -21.41444608039761022, -21.06969765009909423 ) ) ;
#8697 = CARTESIAN_POINT ( 'NONE',  ( 11.58080580526187298, 17.82453155642948772, -25.05040652983576166 ) ) ;
#8698 = CARTESIAN_POINT ( 'NONE',  ( 17.56107106814955898, 10.70378322536777205, -28.30016637139251756 ) ) ;
#8699 = CARTESIAN_POINT ( 'NONE',  ( 12.23327497914553597, 13.81973598992451713, 7.000000000000000000 ) ) ;
#8700 = CARTESIAN_POINT ( 'NONE',  ( -3.610436583610349359, 21.08180157035248214, -25.64550946592787284 ) ) ;
#8701 = EDGE_LOOP ( 'NONE', ( #22685, #14837, #26602, #25476 ) ) ;
#8702 = AXIS2_PLACEMENT_3D ( 'NONE', #35293, #966, #10711 ) ;
#8703 = DIRECTION ( 'NONE',  ( -0.9781476007338042455, 0.2079116908177663647, 0.000000000000000000 ) ) ;
#8704 = ORIENTED_EDGE ( 'NONE', *, *, #36880, .F. ) ;
#8705 = EDGE_CURVE ( 'NONE', #1690, #12341, #37222, .T. ) ;
#8706 = PLANE ( 'NONE',  #30969 ) ;
#8707 = CARTESIAN_POINT ( 'NONE',  ( -6.354454053420243831, 35.54304081427989814, 7.500000000000000888 ) ) ;
#8708 = CARTESIAN_POINT ( 'NONE',  ( -23.85997367143794889, 0.6784800307181348966, -19.51840897779039352 ) ) ;
#8709 = B_SPLINE_CURVE_WITH_KNOTS ( 'NONE', 3,
 ( #29317, #29917, #35817, #29719, #8390, #17747, #14683, #13878 ),
 .UNSPECIFIED., .F., .F.,
 ( 4, 2, 2, 4 ),
 ( 0.000000000000000000, 0.0004726692273637063640, 0.0007090038410455602779, 0.0009453384547274142459 ),
 .UNSPECIFIED. ) ;
#8710 = CARTESIAN_POINT ( 'NONE',  ( 35.29110269690040269, -10.66697437443527008, -6.728013520106306267 ) ) ;
#8711 = AXIS2_PLACEMENT_3D ( 'NONE', #18866, #33371, #30313 ) ;
#8712 = ORIENTED_EDGE ( 'NONE', *, *, #4405, .F. ) ;
#8713 = DIRECTION ( 'NONE',  ( 1.000000000000000000, 0.000000000000000000, 0.000000000000000000 ) ) ;
#8714 = ORIENTED_EDGE ( 'NONE', *, *, #21810, .T. ) ;
#8715 = DIRECTION ( 'NONE',  ( -0.000000000000000000, -0.000000000000000000, -1.000000000000000000 ) ) ;
#8716 = DIRECTION ( 'NONE',  ( 0.000000000000000000, 0.000000000000000000, -1.000000000000000000 ) ) ;
#8717 = AXIS2_PLACEMENT_3D ( 'NONE', #7964, #30316, #10826 ) ;
#8718 = CARTESIAN_POINT ( 'NONE',  ( 11.19134295108988830, 14.88397459621551100, 10.50000000000000000 ) ) ;
#8719 = VERTEX_POINT ( 'NONE', #33867 ) ;
#8720 =( NAMED_UNIT ( * ) SI_UNIT ( $, .STERADIAN. ) SOLID_ANGLE_UNIT ( ) );
#8721 = CARTESIAN_POINT ( 'NONE',  ( -3.992867117591420545, 8.524771480177605554, 10.50000000000000533 ) ) ;
#8722 = CARTESIAN_POINT ( 'NONE',  ( 19.48557158514982746, -11.25000000000009415, 23.00000000000000000 ) ) ;
#8723 = CARTESIAN_POINT ( 'NONE',  ( 0.000000000000000000, 22.50000000000000355, 7.000000000000000000 ) ) ;
#8724 = CARTESIAN_POINT ( 'NONE',  ( 28.33613644512890772, -21.83622121967587759, -10.19242865772655549 ) ) ;
#8725 = CARTESIAN_POINT ( 'NONE',  ( 19.98855543418123659, 14.89803298009520383, -6.936588910547434317 ) ) ;
#8726 = CARTESIAN_POINT ( 'NONE',  ( 12.06095707006059037, 31.48640300589477548, -9.007870101607295510 ) ) ;
#8727 = TOROIDAL_SURFACE ( 'NONE', #11345, 1.000000000000000000, 0.5000000000000000000 ) ;
#8728 = EDGE_LOOP ( 'NONE', ( #28105, #28795, #8999, #4578, #36428 ) ) ;
#8729 = CARTESIAN_POINT ( 'NONE',  ( -18.76069801487658850, 8.513798778646419763, -27.72809068051395442 ) ) ;
#8730 = DIRECTION ( 'NONE',  ( 0.9781476007338069101, 0.2079116908177532363, 0.000000000000000000 ) ) ;
#8731 = LINE ( 'NONE', #11976, #25049 ) ;
#8732 = EDGE_CURVE ( 'NONE', #31582, #32385, #26196, .T. ) ;
#8733 = CARTESIAN_POINT ( 'NONE',  ( 9.606819337878498288, -18.10969338424137831, -29.34610233316817585 ) ) ;
#8734 = DIRECTION ( 'NONE',  ( 0.000000000000000000, 0.000000000000000000, 1.000000000000000000 ) ) ;
#8735 = EDGE_CURVE ( 'NONE', #8719, #13029, #15367, .T. ) ;
#8736 = FACE_OUTER_BOUND ( 'NONE', #5315, .T. ) ;
#8737 = CARTESIAN_POINT ( 'NONE',  ( -14.92028588230428987, 25.84647088687363237, -9.706342443300702172 ) ) ;
#8738 = CARTESIAN_POINT ( 'NONE',  ( -13.91976629483763972, -16.67082186115019482, -24.55897349996614665 ) ) ;
#8739 = CARTESIAN_POINT ( 'NONE',  ( 8.893966021365395491, -18.47319264949478779, -30.00000000000000000 ) ) ;
#8740 = CARTESIAN_POINT ( 'NONE',  ( 11.58359689081945021, 32.01076807263225987, 10.49999999999999822 ) ) ;
#8741 = ADVANCED_FACE ( 'NONE', ( #17640 ), #32236, .T. ) ;
#8742 = ORIENTED_EDGE ( 'NONE', *, *, #22009, .T. ) ;
#8743 = EDGE_LOOP ( 'NONE', ( #32696, #15311 ) ) ;
#8744 = CARTESIAN_POINT ( 'NONE',  ( -6.444683815770512858, 21.56947076293902654, -23.23860985537865886 ) ) ;
#8745 = CYLINDRICAL_SURFACE ( 'NONE', #28336, 16.00000000000000711 ) ;
#8746 = FACE_OUTER_BOUND ( 'NONE', #37062, .T. ) ;
#8747 = VECTOR ( 'NONE', #20529, 1000.000000000000000 ) ;
#8748 = LINE ( 'NONE', #5891, #26701 ) ;
#8749 = VERTEX_POINT ( 'NONE', #33077 ) ;
#8750 = CARTESIAN_POINT ( 'NONE',  ( 21.26671072780636251, 0.8446411308849943733, -25.02192136719475712 ) ) ;
#8751 = CARTESIAN_POINT ( 'NONE',  ( 11.48173768534036121, 32.16538668264416145, 10.49999999999999822 ) ) ;
#8752 = DIRECTION ( 'NONE',  ( 0.000000000000000000, 0.000000000000000000, 1.000000000000000000 ) ) ;
#8753 = ORIENTED_EDGE ( 'NONE', *, *, #34014, .T. ) ;
#8754 = VECTOR ( 'NONE', #7618, 1000.000000000000000 ) ;
#8755 = CARTESIAN_POINT ( 'NONE',  ( -30.69713694106416568, -0.001249014335545420122, -6.887971490028672150 ) ) ;
#8756 = DIRECTION ( 'NONE',  ( -1.000000000000000000, 0.000000000000000000, 0.000000000000000000 ) ) ;
#8757 = ORIENTED_EDGE ( 'NONE', *, *, #16309, .T. ) ;
#8758 = CARTESIAN_POINT ( 'NONE',  ( 31.99794295650106690, -3.876779942215285324, -10.41291006183080725 ) ) ;
#8759 = CARTESIAN_POINT ( 'NONE',  ( 27.98024382195362136, -26.61114576561526590, 13.92931973827785086 ) ) ;
#8760 = ORIENTED_EDGE ( 'NONE', *, *, #4408, .F. ) ;
#8761 = CARTESIAN_POINT ( 'NONE',  ( 12.06278152636307865, 35.25200209733485934, 13.92931973827804626 ) ) ;
#8762 = EDGE_CURVE ( 'NONE', #10807, #32040, #9274, .T. ) ;
#8763 = CARTESIAN_POINT ( 'NONE',  ( -12.28720923544494248, -14.55658080566520418, 20.99999999999999645 ) ) ;
#8764 = FACE_OUTER_BOUND ( 'NONE', #2517, .T. ) ;
#8765 = CARTESIAN_POINT ( 'NONE',  ( -7.604803157139289560, 28.95581125563456126, 20.25080042701564764 ) ) ;
#8766 = DIRECTION ( 'NONE',  ( 0.000000000000000000, 0.000000000000000000, 1.000000000000000000 ) ) ;
#8767 = EDGE_LOOP ( 'NONE', ( #212, #35777 ) ) ;
#8768 = CARTESIAN_POINT ( 'NONE',  ( 1.828660225305865250, 9.087095699275852922, 10.00000000000000000 ) ) ;
#8769 = CARTESIAN_POINT ( 'NONE',  ( 6.312035131040564906, 19.41226734497195849, 12.00000000000000000 ) ) ;
#8770 = CARTESIAN_POINT ( 'NONE',  ( 5.459820500924835507, 28.05023579833048686, -16.71664541261905157 ) ) ;
#8771 = DIRECTION ( 'NONE',  ( 0.07391278520356048265, 0.7032331762534029806, 0.7071067811865493491 ) ) ;
#8772 = CARTESIAN_POINT ( 'NONE',  ( 16.18987435794473839, 9.347228318705804284, 20.25080042701566541 ) ) ;
#8773 = EDGE_CURVE ( 'NONE', #16261, #6733, #27360, .T. ) ;
#8774 = CARTESIAN_POINT ( 'NONE',  ( 19.79884881832018806, -27.24719281008185590, -5.457829539577221389 ) ) ;
#8775 = DIRECTION ( 'NONE',  ( 1.224646799147351235E-16, -1.000000000000000000, 0.000000000000000000 ) ) ;
#8776 = AXIS2_PLACEMENT_3D ( 'NONE', #28561, #19414, #32009 ) ;
#8777 = DIRECTION ( 'NONE',  ( 0.3090169943749573878, 0.9510565162951503115, 0.000000000000000000 ) ) ;
#8778 = CARTESIAN_POINT ( 'NONE',  ( 2.606860170653414244, 7.830819977571334078, 10.82238861112336714 ) ) ;
#8779 = PRODUCT_RELATED_PRODUCT_CATEGORY ( 'part', '', ( #13249 ) ) ;
#8780 = EDGE_LOOP ( 'NONE', ( #8683, #13125, #1023, #28790 ) ) ;
#8781 = CARTESIAN_POINT ( 'NONE',  ( 15.39300221565557436, 26.86528302342467001, -5.473805150799548436 ) ) ;
#8782 = ORIENTED_EDGE ( 'NONE', *, *, #14308, .F. ) ;
#8783 = VECTOR ( 'NONE', #32815, 1000.000000000000114 ) ;
#8784 = CARTESIAN_POINT ( 'NONE',  ( -15.38278943354864836, 26.63434012099637727, -6.417044010450005942 ) ) ;
#8785 = AXIS2_PLACEMENT_3D ( 'NONE', #36978, #6483, #6087 ) ;
#8786 = CARTESIAN_POINT ( 'NONE',  ( -29.45678984391951616, -18.54179626184216545, 19.27171037444122703 ) ) ;
#8787 = CARTESIAN_POINT ( 'NONE',  ( 9.930210031747556343, -18.82842284079468698, -25.01870781754495709 ) ) ;
#8788 = ADVANCED_FACE ( 'NONE', ( #24113 ), #39551, .T. ) ;
#8789 = DIRECTION ( 'NONE',  ( 0.000000000000000000, 0.000000000000000000, 1.000000000000000000 ) ) ;
#8790 = CARTESIAN_POINT ( 'NONE',  ( 11.14269862834027158, 17.45542210456148879, -27.45318300851278082 ) ) ;
#8791 = ADVANCED_FACE ( 'NONE', ( #36315 ), #20877, .T. ) ;
#8792 = ORIENTED_EDGE ( 'NONE', *, *, #3316, .F. ) ;
#8793 = CARTESIAN_POINT ( 'NONE',  ( 30.49893448008974417, -18.04955498499799305, -11.06631362726178835 ) ) ;
#8794 = ORIENTED_EDGE ( 'NONE', *, *, #13451, .F. ) ;
#8796 = CARTESIAN_POINT ( 'NONE',  ( -6.868154521567742421, 35.60001939699343865, 10.49999999999999822 ) ) ;
#8795 = CARTESIAN_POINT ( 'NONE',  ( -14.61184883681244884, 26.27612152894188213, -10.14089745567681078 ) ) ;
#8797 = CARTESIAN_POINT ( 'NONE',  ( -20.57926088536441966, -27.21289976561331514, -5.455544558262904076 ) ) ;
#8798 = CARTESIAN_POINT ( 'NONE',  ( -15.29245034909719081, 32.56469986039895304, -4.999999999999988454 ) ) ;
#8799 = EDGE_LOOP ( 'NONE', ( #3690, #16153, #13797, #17464 ) ) ;
#8800 = CARTESIAN_POINT ( 'NONE',  ( -19.38376532770186600, -6.700500133912340672, -29.23023060093576930 ) ) ;
#8801 = CARTESIAN_POINT ( 'NONE',  ( -14.97946999438102189, -26.42093270519550074, -7.359069949749521555 ) ) ;
#8802 = CARTESIAN_POINT ( 'NONE',  ( 39.59914439355202376, -10.88071517532279309, 11.00000000000000000 ) ) ;
#8803 = EDGE_LOOP ( 'NONE', ( #22277, #39704, #11451, #20806 ) ) ;
#8804 = CARTESIAN_POINT ( 'NONE',  ( 20.76747401923929104, 2.389443645289128337, -26.35181366210539977 ) ) ;
#8805 = DIRECTION ( 'NONE',  ( 0.000000000000000000, 0.000000000000000000, 1.000000000000000000 ) ) ;
#8806 = CARTESIAN_POINT ( 'NONE',  ( -16.58691282011820078, -31.15705289669412181, 11.00000000000000000 ) ) ;
#8807 = ORIENTED_EDGE ( 'NONE', *, *, #25637, .F. ) ;
#8808 = CARTESIAN_POINT ( 'NONE',  ( -30.77003892953206332, -0.07641085285610303701, -6.886502699455107290 ) ) ;
#8809 = EDGE_LOOP ( 'NONE', ( #4323, #22463, #6589, #9829 ) ) ;
#8810 = CARTESIAN_POINT ( 'NONE',  ( 30.69110547573335168, -1.275449444801196597, -10.08822704699340456 ) ) ;
#8811 = CARTESIAN_POINT ( 'NONE',  ( 31.72869323525675966, -3.591677789202227800, 17.92354375535289890 ) ) ;
#8812 = EDGE_CURVE ( 'NONE', #11532, #7488, #19182, .T. ) ;
#8813 = ORIENTED_EDGE ( 'NONE', *, *, #450, .F. ) ;
#8814 = CARTESIAN_POINT ( 'NONE',  ( -25.39309054194246329, 3.513990607092289054, -13.69008351871648443 ) ) ;
#8815 = EDGE_CURVE ( 'NONE', #11592, #36019, #35282, .T. ) ;
#8816 = VECTOR ( 'NONE', #37460, 1000.000000000000000 ) ;
#8817 = CARTESIAN_POINT ( 'NONE',  ( -10.62272290917004192, 33.09068932351447501, 7.455539900862802938 ) ) ;
#8818 = CARTESIAN_POINT ( 'NONE',  ( 5.139519228946050511, 36.36965741570532629, 10.49999999999999822 ) ) ;
#8819 = DIRECTION ( 'NONE',  ( -0.000000000000000000, -0.000000000000000000, -1.000000000000000000 ) ) ;
#8820 = CARTESIAN_POINT ( 'NONE',  ( 7.935100905948329064, 11.57827057593817344, 7.000000000000000000 ) ) ;
#8821 = FACE_BOUND ( 'NONE', #9879, .T. ) ;
#8822 = DIRECTION ( 'NONE',  ( 0.000000000000000000, 0.000000000000000000, 1.000000000000000000 ) ) ;
#8823 = ORIENTED_EDGE ( 'NONE', *, *, #19192, .T. ) ;
#8824 = CARTESIAN_POINT ( 'NONE',  ( -22.58227240774737510, 6.801869239798123523, -15.85529687906895369 ) ) ;
#8825 = CARTESIAN_POINT ( 'NONE',  ( -6.811226782241549316, 35.33967249274201095, 10.49999999999999822 ) ) ;
#8826 = MANIFOLD_SOLID_BREP ( 'Shell1', #26159 ) ;
#8827 = FACE_OUTER_BOUND ( 'NONE', #33325, .T. ) ;
#8828 = CARTESIAN_POINT ( 'NONE',  ( 24.88102591590622836, -25.82163281467740745, -7.612408864933811969 ) ) ;
#8829 = FACE_OUTER_BOUND ( 'NONE', #16928, .T. ) ;
#8830 = EDGE_CURVE ( 'NONE', #17580, #17841, #25106, .T. ) ;
#8831 = CARTESIAN_POINT ( 'NONE',  ( 11.13836630440169984, 18.17080407247200924, -24.99097017320102054 ) ) ;
#8832 = CARTESIAN_POINT ( 'NONE',  ( 5.050662510307052600, -26.77689918168226058, 11.55979286843934872 ) ) ;
#8833 = ORIENTED_EDGE ( 'NONE', *, *, #38942, .F. ) ;
#8834 = CARTESIAN_POINT ( 'NONE',  ( -16.59571780117528306, 22.97185772529794434, -5.474759697025393557 ) ) ;
#8835 = CARTESIAN_POINT ( 'NONE',  ( -22.36336935241945767, -18.10715803802132484, 20.82122704794079837 ) ) ;
#8836 = DIRECTION ( 'NONE',  ( 1.000000000000000000, 0.000000000000000000, 0.000000000000000000 ) ) ;
#8837 = CARTESIAN_POINT ( 'NONE',  ( 12.15468870735817752, 19.89582195369037620, -20.54525176704591516 ) ) ;
#8838 = ORIENTED_EDGE ( 'NONE', *, *, #5168, .F. ) ;
#8839 = CYLINDRICAL_SURFACE ( 'NONE', #36535, 1.000000000000000000 ) ;
#8840 = VERTEX_POINT ( 'NONE', #5227 ) ;
#8841 = AXIS2_PLACEMENT_3D ( 'NONE', #38010, #13020, #34970 ) ;
#8843 = LINE ( 'NONE', #25070, #38685 ) ;
#8842 = CARTESIAN_POINT ( 'NONE',  ( -11.00971296877878558, 17.54494704588714882, -27.44286833666322067 ) ) ;
#8844 = CARTESIAN_POINT ( 'NONE',  ( -15.47037888674134187, -26.61430711100896573, -6.886084615588098146 ) ) ;
#8845 = DIRECTION ( 'NONE',  ( -0.4067366430757919926, 0.9135454576426046414, 0.000000000000000000 ) ) ;
#8846 = VECTOR ( 'NONE', #942, 999.9999999999998863 ) ;
#8847 = CARTESIAN_POINT ( 'NONE',  ( -18.36169979798018304, -11.08193507441912296, -25.57557639782013936 ) ) ;
#8848 = CARTESIAN_POINT ( 'NONE',  ( -13.94379063328525703, -26.36485034788368864, -4.999999999999999112 ) ) ;
#8849 = CARTESIAN_POINT ( 'NONE',  ( 12.80736835487433289, 15.68301270189216545, 9.000000000000001776 ) ) ;
#8850 = CARTESIAN_POINT ( 'NONE',  ( 12.12823232338804402, 16.57707950519044005, -28.75067251775697486 ) ) ;
#8851 = ORIENTED_EDGE ( 'NONE', *, *, #13621, .T. ) ;
#8852 = CARTESIAN_POINT ( 'NONE',  ( 25.22318582504367868, 6.470064654807184290, -6.921000316633144855 ) ) ;
#8853 = VECTOR ( 'NONE', #36916, 1000.000000000000114 ) ;
#8854 = LINE ( 'NONE', #39723, #10219 ) ;
#8855 = DIRECTION ( 'NONE',  ( -0.6691306063588672304, -0.7431448254773862505, 0.000000000000000000 ) ) ;
#8856 = CARTESIAN_POINT ( 'NONE',  ( 4.678013043399745996, 44.50832101651059958, 7.000000000000000000 ) ) ;
#8857 = VERTEX_POINT ( 'NONE', #6801 ) ;
#8858 = CARTESIAN_POINT ( 'NONE',  ( -30.00628679341476968, -0.6868000848423935212, -10.59368060977712389 ) ) ;
#8859 = CARTESIAN_POINT ( 'NONE',  ( 24.62928168306611454, 0.2893784230877288199, -18.43276624462634317 ) ) ;
#8860 = DIRECTION ( 'NONE',  ( 0.9135454576426005335, -0.4067366430758009299, 0.000000000000000000 ) ) ;
#8861 = CARTESIAN_POINT ( 'NONE',  ( 26.86294352747594516, -10.31366695439891679, 20.82122704794079837 ) ) ;
#8862 = CARTESIAN_POINT ( 'NONE',  ( 35.84808252048253507, -3.038699442442335030, -4.999999999999996447 ) ) ;
#8863 = EDGE_CURVE ( 'NONE', #37261, #5543, #13196, .T. ) ;
#8864 = CARTESIAN_POINT ( 'NONE',  ( 12.03640989728592459, 29.14264673470096767, 13.00000000000000178 ) ) ;
#8865 = EDGE_LOOP ( 'NONE', ( #18999, #10452, #7093, #7037 ) ) ;
#8866 = DIRECTION ( 'NONE',  ( 0.000000000000000000, 0.000000000000000000, 1.000000000000000000 ) ) ;
#8867 = AXIS2_PLACEMENT_3D ( 'NONE', #38058, #37856, #13269 ) ;
#8868 = CARTESIAN_POINT ( 'NONE',  ( -10.77091082532341204, 29.60251629318183575, 12.00000000000000000 ) ) ;
#8869 = CARTESIAN_POINT ( 'NONE',  ( -6.082607396026893376, 23.58034083595207875, 13.00000000000000178 ) ) ;
#8870 = CARTESIAN_POINT ( 'NONE',  ( 1.992325487150441665, 27.82770543502457983, -17.60688455110214790 ) ) ;
#8871 = CARTESIAN_POINT ( 'NONE',  ( -5.644276917315534270, 36.40655018617698602, 10.49999999999999822 ) ) ;
#8872 = DIRECTION ( 'NONE',  ( 0.8660254037844432595, 0.4999999999999921729, 0.000000000000000000 ) ) ;
#8873 = DIRECTION ( 'NONE',  ( 0.9135454576426005335, -0.4067366430758008744, 0.000000000000000000 ) ) ;
#8874 = DIRECTION ( 'NONE',  ( -0.9945218953682742891, -0.1045284632676437425, 0.000000000000000000 ) ) ;
#8875 = CYLINDRICAL_SURFACE ( 'NONE', #28733, 0.5000000000000004441 ) ;
#8876 = ADVANCED_FACE ( 'NONE', ( #6412 ), #16926, .F. ) ;
#8877 = CARTESIAN_POINT ( 'NONE',  ( -14.48927117870118408, -30.61587158504671535, 22.99999999999999645 ) ) ;
#8878 = CARTESIAN_POINT ( 'NONE',  ( 13.73764686189923445, 25.77870856457095172, -12.44422647077569266 ) ) ;
#8879 = CARTESIAN_POINT ( 'NONE',  ( 9.821458659721804096, 11.16186433357816910, 7.102637441331451917 ) ) ;
#8880 = EDGE_LOOP ( 'NONE', ( #3182, #1833, #5250, #22618 ) ) ;
#8882 = CARTESIAN_POINT ( 'NONE',  ( 9.665073660139015033, 25.11464168560187460, 10.49999999999999822 ) ) ;
#8881 = CARTESIAN_POINT ( 'NONE',  ( -19.19919298765988813, 15.16185000874999211, -10.86730081220202671 ) ) ;
#8883 = DIRECTION ( 'NONE',  ( 0.4999999999999920064, -0.8660254037844432595, 0.000000000000000000 ) ) ;
#8884 = EDGE_CURVE ( 'NONE', #13564, #15556, #4117, .T. ) ;
#8885 = CARTESIAN_POINT ( 'NONE',  ( 15.40837845075638057, -26.64760342190364995, -6.417007949787735477 ) ) ;
#8886 = CARTESIAN_POINT ( 'NONE',  ( -21.22055300418212553, -26.61708612678433283, -8.117996566443485662 ) ) ;
#8887 = CARTESIAN_POINT ( 'NONE',  ( 31.94006737154955644, 0.9747213384812106751, 13.92931973827808712 ) ) ;
#8888 = CARTESIAN_POINT ( 'NONE',  ( 13.47312776821850200, 22.85298590836225330, -15.44645774616055967 ) ) ;
#8889 = ORIENTED_EDGE ( 'NONE', *, *, #7128, .T. ) ;
#8890 = CARTESIAN_POINT ( 'NONE',  ( -2.317734025672945286, 9.191051544684766483, 10.00000000000000000 ) ) ;
#8891 = CARTESIAN_POINT ( 'NONE',  ( 37.88915196488844117, -19.37406374111511198, 11.00000000000000000 ) ) ;
#8892 = EDGE_CURVE ( 'NONE', #25752, #10001, #31421, .T. ) ;
#8893 = CARTESIAN_POINT ( 'NONE',  ( -18.15993858576987563, -15.09575340168067470, -21.92571465217806193 ) ) ;
#8894 = CARTESIAN_POINT ( 'NONE',  ( 1.503347432918254123, -22.43982916438487152, -18.02207112121201504 ) ) ;
#8895 = CARTESIAN_POINT ( 'NONE',  ( 14.48665838210651025, 23.98092697758879410, -12.56944135157504228 ) ) ;
#8896 = CARTESIAN_POINT ( 'NONE',  ( 20.72086712622418148, 12.75943518406283594, -9.890071669578944125 ) ) ;
#8897 = FACE_OUTER_BOUND ( 'NONE', #35463, .T. ) ;
#8898 = CARTESIAN_POINT ( 'NONE',  ( -2.905413696073824603, 20.70236046713645095, -26.99976967470244560 ) ) ;
#8899 = ORIENTED_EDGE ( 'NONE', *, *, #23183, .T. ) ;
#8900 = CARTESIAN_POINT ( 'NONE',  ( -34.13545392654325639, -6.417351548865673827, -8.088078764923306352 ) ) ;
#8901 = CIRCLE ( 'NONE', #19266, 16.00000000000000000 ) ;
#8902 = CONICAL_SURFACE ( 'NONE', #28375, 0.4999999999999970024, 0.7853981633974447263 ) ;
#8903 = CARTESIAN_POINT ( 'NONE',  ( -32.33143948541790991, 1.358872982501832860, 11.00000000000000000 ) ) ;
#8904 = ORIENTED_EDGE ( 'NONE', *, *, #28856, .T. ) ;
#8905 = DIRECTION ( 'NONE',  ( -0.7431448254773863615, 0.6691306063588671194, 0.000000000000000000 ) ) ;
#8906 = DIRECTION ( 'NONE',  ( 0.6729908358753765585, 0.000000000000000000, 0.7396508195275403041 ) ) ;
#8907 = ADVANCED_FACE ( 'NONE', ( #3570 ), #10067, .F. ) ;
#8908 = VECTOR ( 'NONE', #3209, 999.9999999999998863 ) ;
#8909 = CARTESIAN_POINT ( 'NONE',  ( -30.15656701667666439, 0.6301168163923819288, -6.418133929584069364 ) ) ;
#8910 = EDGE_CURVE ( 'NONE', #5646, #19243, #726, .T. ) ;
#8911 = CARTESIAN_POINT ( 'NONE',  ( 34.05585594407177297, -13.68619932326567756, -8.863084868655485948 ) ) ;
#8912 = EDGE_CURVE ( 'NONE', #29040, #4287, #34855, .T. ) ;
#8913 = CIRCLE ( 'NONE', #36799, 1.000000000000000000 ) ;
#8914 = EDGE_LOOP ( 'NONE', ( #27107, #9370, #4644, #27794 ) ) ;
#8915 = PLANE ( 'NONE',  #25195 ) ;
#8916 = VERTEX_POINT ( 'NONE', #15966 ) ;
#8917 = CARTESIAN_POINT ( 'NONE',  ( -5.082607396026893376, 23.58034083595207875, 12.00000000000000000 ) ) ;
#8918 = DIRECTION ( 'NONE',  ( 1.000000000000000000, 0.000000000000000000, 0.000000000000000000 ) ) ;
#8919 = DIRECTION ( 'NONE',  ( 0.9135454576426059736, 0.4067366430757889395, -0.000000000000000000 ) ) ;
#8920 = ORIENTED_EDGE ( 'NONE', *, *, #6400, .F. ) ;
#8921 = CARTESIAN_POINT ( 'NONE',  ( -1.811830127027588722, 22.73191323099810290, -23.00449321371658939 ) ) ;
#8922 = CARTESIAN_POINT ( 'NONE',  ( -9.736411649803377699, 11.65093146000205770, 7.000000000000000000 ) ) ;
#8923 = DIRECTION ( 'NONE',  ( 0.000000000000000000, 0.000000000000000000, -1.000000000000000000 ) ) ;
#8924 = CYLINDRICAL_SURFACE ( 'NONE', #7849, 0.5000000000000005551 ) ;
#8925 = CARTESIAN_POINT ( 'NONE',  ( 18.78373925409778877, -14.41787429400073428, -21.88907065838856525 ) ) ;
#8926 = EDGE_CURVE ( 'NONE', #20981, #7910, #1481, .T. ) ;
#8927 = CARTESIAN_POINT ( 'NONE',  ( 16.30460026483097735, 12.60001878089315674, -27.71906073260982595 ) ) ;
#8928 = AXIS2_PLACEMENT_3D ( 'NONE', #2705, #39276, #36637 ) ;
#8929 = CARTESIAN_POINT ( 'NONE',  ( 13.05426751670861130, 31.50888625344096994, -6.795852486021440875 ) ) ;
#8930 = AXIS2_PLACEMENT_3D ( 'NONE', #2952, #34037, #6385 ) ;
#8931 = ORIENTED_EDGE ( 'NONE', *, *, #17882, .F. ) ;
#8932 = CARTESIAN_POINT ( 'NONE',  ( -18.69324927053147789, 8.492311550642993367, -28.85813498384544218 ) ) ;
#8933 = DIRECTION ( 'NONE',  ( 0.000000000000000000, 0.000000000000000000, -1.000000000000000000 ) ) ;
#8934 = EDGE_CURVE ( 'NONE', #23537, #35497, #11963, .T. ) ;
#8935 = CARTESIAN_POINT ( 'NONE',  ( 14.99763921991110571, -25.86109370504824412, -9.702356291737144645 ) ) ;
#8936 = DIRECTION ( 'NONE',  ( 1.000000000000000000, 0.000000000000000000, 0.000000000000000000 ) ) ;
#8937 = AXIS2_PLACEMENT_3D ( 'NONE', #2572, #20864, #24300 ) ;
#8938 = FACE_OUTER_BOUND ( 'NONE', #18407, .T. ) ;
#8939 = CARTESIAN_POINT ( 'NONE',  ( -15.00345964543641308, 26.01693641737093543, -9.235896020594065448 ) ) ;
#8940 = CARTESIAN_POINT ( 'NONE',  ( -17.77420980351482171, -19.95186716711776143, -17.87573902456129460 ) ) ;
#8941 = CARTESIAN_POINT ( 'NONE',  ( 12.51658123429344371, -25.23695220677343798, -10.22225441809272617 ) ) ;
#8942 = CARTESIAN_POINT ( 'NONE',  ( 11.50946345163907836, 31.52577281809587717, 10.49999999999999822 ) ) ;
#8943 = EDGE_LOOP ( 'NONE', ( #18200, #23996 ) ) ;
#8944 = ORIENTED_EDGE ( 'NONE', *, *, #24546, .F. ) ;
#8945 = CARTESIAN_POINT ( 'NONE',  ( -10.67202016487744309, 32.33296029975388564, -9.856390611844069838 ) ) ;
#8946 = FACE_OUTER_BOUND ( 'NONE', #10028, .T. ) ;
#8947 = CARTESIAN_POINT ( 'NONE',  ( -11.44134295108998245, 15.31698729810788251, 7.000000000000000000 ) ) ;
#8948 = LINE ( 'NONE', #33747, #13735 ) ;
#8949 = ORIENTED_EDGE ( 'NONE', *, *, #1205, .T. ) ;
#8950 = CARTESIAN_POINT ( 'NONE',  ( 30.44811295758598391, 0.02673777661638704339, -7.828045874607348686 ) ) ;
#8951 = CYLINDRICAL_SURFACE ( 'NONE', #10921, 1.000000000000000000 ) ;
#8952 = DIRECTION ( 'NONE',  ( -0.000000000000000000, -0.000000000000000000, 1.000000000000000000 ) ) ;
#8953 = CONICAL_SURFACE ( 'NONE', #3746, 1.000000000000002665, 0.7853981633974543852 ) ;
#8954 = ORIENTED_EDGE ( 'NONE', *, *, #33389, .T. ) ;
#8955 = CARTESIAN_POINT ( 'NONE',  ( -30.60578642345652156, -0.007519314768002983290, -7.357895972641363080 ) ) ;
#8956 = CARTESIAN_POINT ( 'NONE',  ( -6.330077540933487512, 17.71145523154927659, 6.000000000000000000 ) ) ;
#8957 = ORIENTED_EDGE ( 'NONE', *, *, #25566, .T. ) ;
#8958 = CARTESIAN_POINT ( 'NONE',  ( 20.84933153278981166, -4.276367845268469026, -25.81179670892463918 ) ) ;
#8959 = AXIS2_PLACEMENT_3D ( 'NONE', #27634, #18301, #18696 ) ;
#8960 = VECTOR ( 'NONE', #24090, 1000.000000000000000 ) ;
#8961 = ORIENTED_EDGE ( 'NONE', *, *, #5090, .F. ) ;
#8962 = CARTESIAN_POINT ( 'NONE',  ( 7.450289500751110516, 38.62958991718475943, 13.32518128616595199 ) ) ;
#8963 = EDGE_CURVE ( 'NONE', #26936, #35634, #38653, .T. ) ;
#8964 = TOROIDAL_SURFACE ( 'NONE', #20664, 1.000000000000000000, 0.5000000000000000000 ) ;
#8965 = CARTESIAN_POINT ( 'NONE',  ( 18.23649648353778474, -16.09146789626167262, 20.99999999999999645 ) ) ;
#8966 = B_SPLINE_CURVE_WITH_KNOTS ( 'NONE', 3,
 ( #3171, #21453, #37293, #2971 ),
 .UNSPECIFIED., .F., .F.,
 ( 4, 4 ),
 ( 0.000000000000000000, 1.000000000000000000 ),
 .UNSPECIFIED. ) ;
#8967 = LINE ( 'NONE', #30302, #34464 ) ;
#8968 = CARTESIAN_POINT ( 'NONE',  ( 8.231377095499450292, 29.48763288632292756, 19.99202127657103389 ) ) ;
#8969 = VECTOR ( 'NONE', #21534, 1000.000000000000000 ) ;
#8970 = CARTESIAN_POINT ( 'NONE',  ( -3.531008893910706714, 8.292776413244068223, 11.00000000000000355 ) ) ;
#8971 = ORIENTED_EDGE ( 'NONE', *, *, #21797, .F. ) ;
#8972 = CARTESIAN_POINT ( 'NONE',  ( -17.34253826607186966, 27.32041144404028188, 11.00000000000000000 ) ) ;
#8973 = DIRECTION ( 'NONE',  ( 1.000000000000000000, 0.000000000000000000, 0.000000000000000000 ) ) ;
#8974 = CARTESIAN_POINT ( 'NONE',  ( 6.877368450614945061, 35.27937098263085858, -9.323842147869731534 ) ) ;
#8975 = CARTESIAN_POINT ( 'NONE',  ( 0.7344908159097338629, 8.754836972118123839, 12.00000000000000000 ) ) ;
#8976 = CARTESIAN_POINT ( 'NONE',  ( 16.53758848021426076, -26.97586464850826005, -5.469368573213387208 ) ) ;
#8977 = CYLINDRICAL_SURFACE ( 'NONE', #30758, 0.5000000000000000000 ) ;
#8978 = DIRECTION ( 'NONE',  ( -1.000000000000000000, 0.000000000000000000, 0.000000000000000000 ) ) ;
#8979 = CARTESIAN_POINT ( 'NONE',  ( -12.03641663870442713, 15.85735326529964873, 6.000000000000000000 ) ) ;
#8980 = ORIENTED_EDGE ( 'NONE', *, *, #37188, .F. ) ;
#8981 = EDGE_LOOP ( 'NONE', ( #37968, #25711 ) ) ;
#8983 = CIRCLE ( 'NONE', #7673, 16.00000000000001066 ) ;
#8982 = CARTESIAN_POINT ( 'NONE',  ( -15.18305171862558645, 26.25295951765882307, -8.297948513766829848 ) ) ;
#8984 = CARTESIAN_POINT ( 'NONE',  ( -32.65234849725306532, -15.41672394535184054, 18.42518152272107557 ) ) ;
#8985 = CARTESIAN_POINT ( 'NONE',  ( 14.79500207508366216, -26.08087507433808483, -8.770434559489167725 ) ) ;
#8986 = DIRECTION ( 'NONE',  ( 0.000000000000000000, 0.000000000000000000, 1.000000000000000000 ) ) ;
#8987 = ORIENTED_EDGE ( 'NONE', *, *, #16350, .T. ) ;
#8988 = ORIENTED_EDGE ( 'NONE', *, *, #36476, .T. ) ;
#8989 = AXIS2_PLACEMENT_3D ( 'NONE', #13698, #1726, #7808 ) ;
#8991 = CYLINDRICAL_SURFACE ( 'NONE', #23802, 1.000000000000000000 ) ;
#8990 = CARTESIAN_POINT ( 'NONE',  ( -11.39786025644706768, 22.73419919495342256, -18.20970581293603985 ) ) ;
#8992 = CARTESIAN_POINT ( 'NONE',  ( -14.28885256234768164, -20.44271994159482020, -19.17122735343420459 ) ) ;
#8993 = DIRECTION ( 'NONE',  ( 0.000000000000000000, 0.000000000000000000, 1.000000000000000000 ) ) ;
#8994 = AXIS2_PLACEMENT_3D ( 'NONE', #5455, #17862, #21097 ) ;
#8995 = ORIENTED_EDGE ( 'NONE', *, *, #14619, .T. ) ;
#8996 = CARTESIAN_POINT ( 'NONE',  ( -23.11120214780726201, -7.974055487576295675, -20.80445922199539055 ) ) ;
#8997 = CARTESIAN_POINT ( 'NONE',  ( -14.29598325306471907, -25.39746503277514122, -10.66025640362116533 ) ) ;
#8998 = CARTESIAN_POINT ( 'NONE',  ( 0.5000000000000000000, 37.13089969389957901, 11.00000000000000355 ) ) ;
#8999 = ORIENTED_EDGE ( 'NONE', *, *, #39624, .T. ) ;
#9000 = CARTESIAN_POINT ( 'NONE',  ( 22.44741482142110911, 1.549842875461872937, -21.73216677922275863 ) ) ;
#9001 = CARTESIAN_POINT ( 'NONE',  ( -0.5000000000000004441, 37.00000000000000711, 7.500000000000000888 ) ) ;
#9002 = CARTESIAN_POINT ( 'NONE',  ( 8.411683849014126579, 19.76687823897103868, 9.000000000000001776 ) ) ;
#9003 = VERTEX_POINT ( 'NONE', #3178 ) ;
#9004 = CARTESIAN_POINT ( 'NONE',  ( -23.96634676013683318, 0.4262288974861807023, -19.48813325609940605 ) ) ;
#9005 = ORIENTED_EDGE ( 'NONE', *, *, #9813, .F. ) ;
#9006 = CARTESIAN_POINT ( 'NONE',  ( 31.77445454197319563, -1.004264897904582954, -5.468445260902000449 ) ) ;
#9007 = CARTESIAN_POINT ( 'NONE',  ( 30.82027224585396397, -2.301877357437541072, 17.92354375535443722 ) ) ;
#9008 = EDGE_CURVE ( 'NONE', #3338, #19810, #24908, .T. ) ;
#9009 = ORIENTED_EDGE ( 'NONE', *, *, #11946, .F. ) ;
#9010 = CARTESIAN_POINT ( 'NONE',  ( -24.98802169602269174, 2.696897768699792586, -15.63010232505275177 ) ) ;
#9011 = CARTESIAN_POINT ( 'NONE',  ( 14.86556419889027048, 20.43481210330100240, 11.00000000000000000 ) ) ;
#9012 = CARTESIAN_POINT ( 'NONE',  ( 14.47283171447379146, 21.48159823030311344, 7.000000000000000000 ) ) ;
#9013 = AXIS2_PLACEMENT_3D ( 'NONE', #23592, #23787, #14243 ) ;
#9014 = CARTESIAN_POINT ( 'NONE',  ( -15.12590024503300512, -28.14827041158709875, 13.92931973827808534 ) ) ;
#9015 = EDGE_CURVE ( 'NONE', #38676, #2411, #34261, .T. ) ;
#9016 = CARTESIAN_POINT ( 'NONE',  ( 10.77090408390491127, 15.39748370681878775, 6.000000000000000000 ) ) ;
#9017 = EDGE_CURVE ( 'NONE', #11250, #26597, #15763, .T. ) ;
#9018 = VECTOR ( 'NONE', #7557, 1000.000000000000000 ) ;
#9019 = B_SPLINE_SURFACE_WITH_KNOTS ( 'NONE', 3, 3, ( 
 ( #14322, #1533, #26715, #39703, #8433, #24069, #11680 ),
 ( #11481, #2731, #8832, #24267, #9029, #20632, #23868 ),
 ( #20830, #2341, #33032, #17983, #15122, #5180, #39896 ),
 ( #27511, #30373, #36064, #36462, #8226, #36662, #8631 ),
 ( #5573, #36270, #21218, #2538, #33231, #12072, #39504 ),
 ( #24462, #33433, #14522, #21023, #11876, #33629, #5778 ),
 ( #18179, #30573, #17592, #27117, #14926, #29960, #36860 ),
 ( #2140, #5378, #27314, #14727, #26915, #39303, #30168 ),
 ( #17793, #35797, #8157, #8365, #29094, #2075, #32556 ),
 ( #36201, #7952, #38438, #11213, #1267, #14254, #26646 ),
 ( #14450, #20365, #13853, #26847, #10610, #1878, #11018 ),
 ( #38841, #7553, #5114, #10813, #13651, #32959, #29495 ),
 ( #29297, #32352, #23402, #1467, #17521, #38638, #32757 ),
 ( #4913, #39034, #17320, #4513, #23200, #29695, #23798 ),
 ( #29893, #26243, #35599, #26038, #32144, #4715, #7754 ),
 ( #20159, #17119, #39236, #1670, #20562, #23603, #14050 ),
 ( #4308, #26443, #35395, #22991, #11416, #36001, #16710 ),
 ( #19957, #16915, #12206, #30505, #18309, #2666, #14659 ),
 ( #15052, #9162, #17918, #30700, #11809, #30301, #27845 ),
 ( #15255, #3060, #27245, #24794, #24195, #21354, #2474 ),
 ( #14860, #27442, #39830, #33559, #27643, #39634, #20765 ),
 ( #36592, #17722, #30898, #21151, #33161, #37191, #24397 ),
 ( #40025, #30097, #2865, #24600, #36992, #15454, #36789 ),
 ( #18, #27050, #21545, #12007, #33945, #33761, #39435 ),
 ( #8965, #5907, #33362, #6103, #18508, #8763, #12402 ) ),
 .UNSPECIFIED., .F., .F., .F.,
 ( 4, 3, 3, 3, 3, 3, 3, 3, 4 ),
 ( 4, 3, 4 ),
 ( 0.000000000000000000, 0.1250000000000000000, 0.2500000000000000000, 0.3750000000000000000, 0.5000000000000000000, 0.6250000000000000000, 0.7500000000000000000, 0.8750000000000000000, 1.000000000000000000 ),
 ( 1.318307113131750086, 1.570796326794896336, 1.823285540458042586 ),
 .UNSPECIFIED. ) ;
#9020 = FACE_BOUND ( 'NONE', #26337, .T. ) ;
#9021 = CARTESIAN_POINT ( 'NONE',  ( -5.396718838163291565, 36.49572678120085811, 7.455539900862802050 ) ) ;
#9022 = ORIENTED_EDGE ( 'NONE', *, *, #36962, .T. ) ;
#9023 = CARTESIAN_POINT ( 'NONE',  ( -24.75996061988843167, 7.109052737702043601, -6.924578970779640130 ) ) ;
#9024 = CARTESIAN_POINT ( 'NONE',  ( 8.744117900323280068, 12.16605582823063791, 10.50000000000000000 ) ) ;
#9025 = CARTESIAN_POINT ( 'NONE',  ( 14.42035624161478857, 26.65972665747660031, 7.000000000000000000 ) ) ;
#9026 = CARTESIAN_POINT ( 'NONE',  ( 14.20597032484196376, -14.79219592438034780, -29.99999999999998934 ) ) ;
#9027 = DIRECTION ( 'NONE',  ( 1.000000000000000000, 0.000000000000000000, 0.000000000000000000 ) ) ;
#9028 = CARTESIAN_POINT ( 'NONE',  ( 11.74151979421917957, 19.54197345652316287, -21.58831892365258653 ) ) ;
#9029 = CARTESIAN_POINT ( 'NONE',  ( -5.050662510306967334, -26.77689918168226058, 11.55979286843934872 ) ) ;
#9030 = EDGE_LOOP ( 'NONE', ( #20448, #36548, #25426, #34755 ) ) ;
#9031 = CARTESIAN_POINT ( 'NONE',  ( -15.62169025857701499, 22.97777262041562807, -10.70896060004613659 ) ) ;
#9032 = CARTESIAN_POINT ( 'NONE',  ( -19.25011873046071642, -17.89323911765397312, 20.94377226548387583 ) ) ;
#9033 = EDGE_CURVE ( 'NONE', #1139, #16240, #11422, .T. ) ;
#9034 = EDGE_CURVE ( 'NONE', #10554, #25424, #37878, .T. ) ;
#9035 = CARTESIAN_POINT ( 'NONE',  ( -2.835137251120299684, 29.44922644035488446, 12.00000000000000000 ) ) ;
#9036 = CARTESIAN_POINT ( 'NONE',  ( 15.42861054628522233, 26.73803055450190058, -4.999999999999998224 ) ) ;
#9037 = ORIENTED_EDGE ( 'NONE', *, *, #32237, .T. ) ;
#9038 = CARTESIAN_POINT ( 'NONE',  ( -1.605702774688126722, 27.44183462127829642, 6.000000000000000000 ) ) ;
#9039 = EDGE_LOOP ( 'NONE', ( #1634, #25978 ) ) ;
#9041 = FACE_OUTER_BOUND ( 'NONE', #5358, .T. ) ;
#9040 = CARTESIAN_POINT ( 'NONE',  ( -11.37233562734991743, 18.53355911076921458, -23.83618781163009714 ) ) ;
#9042 = CARTESIAN_POINT ( 'NONE',  ( -12.06406342568560852, -21.47399357335907411, -18.43280010396646773 ) ) ;
#9043 = CARTESIAN_POINT ( 'NONE',  ( -3.153820973115281312, 32.04219121950185212, 10.50000000000000533 ) ) ;
#9044 = CIRCLE ( 'NONE', #31743, 1.000000000000000000 ) ;
#9045 = AXIS2_PLACEMENT_3D ( 'NONE', #1999, #20484, #30430 ) ;
#9046 = CARTESIAN_POINT ( 'NONE',  ( -33.93084094755159441, -17.77584818155513702, -6.276893119624509687 ) ) ;
#9047 = CARTESIAN_POINT ( 'NONE',  ( -7.556576989782998410, -19.27055189435807137, -27.57996940079889825 ) ) ;
#9048 = DIRECTION ( 'NONE',  ( -1.000000000000000000, 0.000000000000000000, 0.000000000000000000 ) ) ;
#9049 = CARTESIAN_POINT ( 'NONE',  ( 14.65083719384613659, 22.52921530560692887, -13.58206962684690922 ) ) ;
#9050 = ORIENTED_EDGE ( 'NONE', *, *, #1461, .F. ) ;
#9051 = CARTESIAN_POINT ( 'NONE',  ( 19.17388597792686866, 7.309708964681583154, -28.84800037308729515 ) ) ;
#9052 = CARTESIAN_POINT ( 'NONE',  ( -75.15099915297791711, 43.38844959084113384, -5.000000000000000000 ) ) ;
#9053 = CARTESIAN_POINT ( 'NONE',  ( -5.082607396026893376, 23.58034083595207875, 13.00000000000000178 ) ) ;
#9054 = CARTESIAN_POINT ( 'NONE',  ( -20.57924982997939622, -27.21273881503329051, -4.999999999999998224 ) ) ;
#9055 = VECTOR ( 'NONE', #38592, 1000.000000000000000 ) ;
#9056 = ORIENTED_EDGE ( 'NONE', *, *, #28865, .T. ) ;
#9057 = CARTESIAN_POINT ( 'NONE',  ( -20.49507156785942641, -0.4678258087238867380, -30.00000000000000000 ) ) ;
#9058 = CARTESIAN_POINT ( 'NONE',  ( 30.67844260339930074, -0.08294063150054889477, -7.355559089466812139 ) ) ;
#9059 = CARTESIAN_POINT ( 'NONE',  ( -10.16521142134453548, 24.66068167190384841, 13.00000000000000178 ) ) ;
#9060 = CARTESIAN_POINT ( 'NONE',  ( 26.19533169775624160, -16.15700992729039598, 20.69868183039781329 ) ) ;
#9061 = ORIENTED_EDGE ( 'NONE', *, *, #19718, .F. ) ;
#9062 = EDGE_CURVE ( 'NONE', #25521, #11885, #4149, .T. ) ;
#9063 = CARTESIAN_POINT ( 'NONE',  ( 20.90924525106827758, -8.502318254486461058, -30.00000000000001421 ) ) ;
#9064 = CARTESIAN_POINT ( 'NONE',  ( 0.4999999999999995559, 37.00000000000000711, 11.00000000000000000 ) ) ;
#9065 = EDGE_LOOP ( 'NONE', ( #18325, #34333, #16018, #2256 ) ) ;
#9066 = DIRECTION ( 'NONE',  ( 0.000000000000000000, 0.000000000000000000, 1.000000000000000000 ) ) ;
#9067 = VECTOR ( 'NONE', #34057, 1000.000000000000000 ) ;
#9068 = CARTESIAN_POINT ( 'NONE',  ( -33.75875814100324135, 2.759858869446476959, 11.00000000000000000 ) ) ;
#9069 = DIRECTION ( 'NONE',  ( 1.000000000000000000, 0.000000000000000000, 0.000000000000000000 ) ) ;
#9070 = CARTESIAN_POINT ( 'NONE',  ( 2.547048354218667043, 35.22824564786088075, -11.07258388855395914 ) ) ;
#9071 = CARTESIAN_POINT ( 'NONE',  ( 4.980911888400610721, 31.22871793335020385, 10.49999999999999822 ) ) ;
#9072 = CARTESIAN_POINT ( 'NONE',  ( 14.83795255154715598, 20.43771420437945352, 10.68306085400105943 ) ) ;
#9073 = DIRECTION ( 'NONE',  ( 0.000000000000000000, 0.000000000000000000, -1.000000000000000000 ) ) ;
#9074 = AXIS2_PLACEMENT_3D ( 'NONE', #38540, #26144, #10714 ) ;
#9075 = CARTESIAN_POINT ( 'NONE',  ( 9.221287281574507944, 10.65863771052197784, 7.000000000000000000 ) ) ;
#9076 = CYLINDRICAL_SURFACE ( 'NONE', #30695, 1.000000000000000888 ) ;
#9077 = DIRECTION ( 'NONE',  ( -1.000000000000000000, 0.000000000000000000, 0.000000000000000000 ) ) ;
#9078 = CARTESIAN_POINT ( 'NONE',  ( 14.50911442997946388, 26.55381056816341712, -10.12498485435761886 ) ) ;
#9079 = DIRECTION ( 'NONE',  ( 1.000000000000000000, 0.000000000000000000, 0.000000000000000000 ) ) ;
#9080 = ORIENTED_EDGE ( 'NONE', *, *, #5484, .T. ) ;
#9082 = DIRECTION ( 'NONE',  ( 1.000000000000000000, 0.000000000000000000, 0.000000000000000000 ) ) ;
#9081 = CARTESIAN_POINT ( 'NONE',  ( -16.50249576148715036, 14.88229690510866199, -20.02363424797698954 ) ) ;
#9083 = LINE ( 'NONE', #21468, #26355 ) ;
#9084 = CARTESIAN_POINT ( 'NONE',  ( 14.87432661258679900, -25.83349755148350013, -9.709001257180572608 ) ) ;
#9085 = EDGE_CURVE ( 'NONE', #37515, #4328, #39849, .T. ) ;
#9086 = CARTESIAN_POINT ( 'NONE',  ( -21.53459943946054622, -26.97023605249422928, -6.785410596037112718 ) ) ;
#9087 = CARTESIAN_POINT ( 'NONE',  ( 31.51573171626900205, 0.5582143012820770522, 15.13084544680213561 ) ) ;
#9088 = CARTESIAN_POINT ( 'NONE',  ( 15.16643734843948721, 26.30888157207252931, -8.296799070927670883 ) ) ;
#9089 = VERTEX_POINT ( 'NONE', #4726 ) ;
#9090 = DIRECTION ( 'NONE',  ( 0.000000000000000000, 0.000000000000000000, 1.000000000000000000 ) ) ;
#9091 = CARTESIAN_POINT ( 'NONE',  ( -9.526537139939113885, -18.29543337056835028, -28.07984914598426229 ) ) ;
#9092 = CARTESIAN_POINT ( 'NONE',  ( -36.56052011373579802, -7.179325806537445231, 13.92931973827734993 ) ) ;
#9093 = CARTESIAN_POINT ( 'NONE',  ( -21.21462556743105310, -17.67001013903248108, -17.67149726547187072 ) ) ;
#9094 = CARTESIAN_POINT ( 'NONE',  ( 1.281579315327491253, -20.83699243184387129, -25.51341547554553202 ) ) ;
#9095 = CARTESIAN_POINT ( 'NONE',  ( 15.24262546998190437, 25.26847083144028971, -9.247276495989826373 ) ) ;
#9096 = CARTESIAN_POINT ( 'NONE',  ( 21.57989771907153198, 12.01233037074124788, -6.940427116014089570 ) ) ;
#9097 = DIRECTION ( 'NONE',  ( 0.4999999999999930056, -0.8660254037844428154, 0.000000000000000000 ) ) ;
#9098 = CARTESIAN_POINT ( 'NONE',  ( -3.498807313483044634, 20.43805243329230592, -27.74525970097024086 ) ) ;
#9099 = EDGE_LOOP ( 'NONE', ( #30483, #7131 ) ) ;
#9100 = CARTESIAN_POINT ( 'NONE',  ( -30.36244809506906606, -4.747588337124046376, -13.13675111056742217 ) ) ;
#9101 = CARTESIAN_POINT ( 'NONE',  ( -28.63966609530878671, 4.835996017633398480, 12.73282698325538398 ) ) ;
#9102 = ORIENTED_EDGE ( 'NONE', *, *, #21885, .F. ) ;
#9103 = DIRECTION ( 'NONE',  ( 1.000000000000000000, 0.000000000000000000, 0.000000000000000000 ) ) ;
#9104 = DIRECTION ( 'NONE',  ( 0.000000000000000000, 0.000000000000000000, -1.000000000000000000 ) ) ;
#9105 = AXIS2_PLACEMENT_3D ( 'NONE', #15958, #19003, #3955 ) ;
#9106 = CARTESIAN_POINT ( 'NONE',  ( -20.78574042926797460, 1.163748492297181025, -26.85583114029146401 ) ) ;
#9107 = ADVANCED_FACE ( 'NONE', ( #32770 ), #17133, .T. ) ;
#9108 = CARTESIAN_POINT ( 'NONE',  ( 33.14339359398684337, -13.30814253901729316, -10.19541812155104488 ) ) ;
#9109 = EDGE_CURVE ( 'NONE', #38623, #10038, #2486, .T. ) ;
#9110 = ORIENTED_EDGE ( 'NONE', *, *, #6439, .F. ) ;
#9111 = CARTESIAN_POINT ( 'NONE',  ( 7.353987181296509412, 35.57359447655183970, 7.000000000000000000 ) ) ;
#9112 = ORIENTED_EDGE ( 'NONE', *, *, #30569, .T. ) ;
#9113 = FACE_OUTER_BOUND ( 'NONE', #35329, .T. ) ;
#9114 = CARTESIAN_POINT ( 'NONE',  ( 19.26948696230200397, 27.85601271560037162, 11.00000000000000000 ) ) ;
#9115 = AXIS2_PLACEMENT_3D ( 'NONE', #8820, #21206, #33613 ) ;
#9116 = EDGE_CURVE ( 'NONE', #10226, #31380, #23214, .T. ) ;
#9117 = LINE ( 'NONE', #18662, #632 ) ;
#9118 = EDGE_LOOP ( 'NONE', ( #5289, #31981, #22, #34575 ) ) ;
#9119 = CARTESIAN_POINT ( 'NONE',  ( -3.045440459837997604, 37.80942315677882704, -7.122015871823959898 ) ) ;
#9120 = CARTESIAN_POINT ( 'NONE',  ( -4.503793317224517700, 8.420815634768723967, 7.000000000000000000 ) ) ;
#9121 = DIRECTION ( 'NONE',  ( 1.000000000000000000, 0.000000000000000000, 0.000000000000000000 ) ) ;
#9122 = CARTESIAN_POINT ( 'NONE',  ( 19.48557158514997667, 33.74999999999982236, 11.00000000000000000 ) ) ;
#9123 = CARTESIAN_POINT ( 'NONE',  ( 16.27615822911637622, -12.47890632334475924, -30.00000000000001421 ) ) ;
#9124 = CARTESIAN_POINT ( 'NONE',  ( 19.48931724336470594, 15.88182490461431406, -6.933233223513477483 ) ) ;
#9125 = CARTESIAN_POINT ( 'NONE',  ( 8.160668170145010336, 19.01481104899739094, -27.91480984821776801 ) ) ;
#9126 = EDGE_LOOP ( 'NONE', ( #24357, #19443, #37182, #30732, #15343, #23399 ) ) ;
#9127 = CARTESIAN_POINT ( 'NONE',  ( -19.83482056652078640, 8.857944167693910131, -21.15899509700257042 ) ) ;
#9128 = CARTESIAN_POINT ( 'NONE',  ( 3.833852081710629189, 25.75497152300991033, 23.00000000000000355 ) ) ;
#9129 = CARTESIAN_POINT ( 'NONE',  ( 10.65945867603157815, -19.54002146369526827, -22.71882543429452284 ) ) ;
#9130 = DIRECTION ( 'NONE',  ( 0.000000000000000000, 0.000000000000000000, 1.000000000000000000 ) ) ;
#9131 = EDGE_CURVE ( 'NONE', #17337, #31250, #22974, .T. ) ;
#9132 = EDGE_CURVE ( 'NONE', #36141, #19767, #34669, .T. ) ;
#9133 = CARTESIAN_POINT ( 'NONE',  ( 16.77267017469755217, -29.13948811618736912, -5.000000000000000888 ) ) ;
#9134 = B_SPLINE_CURVE_WITH_KNOTS ( 'NONE', 3,
 ( #24479, #101, #12090, #24678, #36875, #37072 ),
 .UNSPECIFIED., .F., .F.,
 ( 4, 2, 4 ),
 ( 0.06666641432897602026, 0.5333332071644880656, 1.000000000000000000 ),
 .UNSPECIFIED. ) ;
#9135 = ADVANCED_FACE ( 'NONE', ( #39249 ), #33382, .T. ) ;
#9136 = CARTESIAN_POINT ( 'NONE',  ( -12.11893889750869135, 19.93834885319187578, -20.53850700616269265 ) ) ;
#9137 = CARTESIAN_POINT ( 'NONE',  ( -24.97569650337160496, -26.32149808972361527, -5.000000000000002665 ) ) ;
#9138 = CARTESIAN_POINT ( 'NONE',  ( 8.369344652847257038, -18.90615068489544370, -27.52829367847808939 ) ) ;
#9139 = CARTESIAN_POINT ( 'NONE',  ( 11.25022250131758383, 31.95692947463369649, 10.96580508970282608 ) ) ;
#9140 = VERTEX_POINT ( 'NONE', #4929 ) ;
#9141 = CARTESIAN_POINT ( 'NONE',  ( -9.109889474751160066, 30.44524786122741489, -13.03254955294998751 ) ) ;
#9142 = CARTESIAN_POINT ( 'NONE',  ( 1.000000000000000444, 37.00000000000000711, 10.49999999999999822 ) ) ;
#9143 = CARTESIAN_POINT ( 'NONE',  ( -7.713869163866016621, 10.18146832927085121, 10.50000000000000711 ) ) ;
#9144 = CIRCLE ( 'NONE', #28592, 15.00000000000000000 ) ;
#9145 = CARTESIAN_POINT ( 'NONE',  ( 0.6056960332696259552, 17.55816537872232530, 6.000000000000000000 ) ) ;
#9146 = ORIENTED_EDGE ( 'NONE', *, *, #3441, .F. ) ;
#9147 = CARTESIAN_POINT ( 'NONE',  ( 27.12540744812873683, 0.2567673158908028719, -14.47800510790882633 ) ) ;
#9148 = VECTOR ( 'NONE', #6797, 1000.000000000000114 ) ;
#9149 = CARTESIAN_POINT ( 'NONE',  ( 14.21391437420825099, 30.04769070240185869, -5.000000000000000000 ) ) ;
#9150 = PLANE ( 'NONE',  #40058 ) ;
#9151 = ORIENTED_EDGE ( 'NONE', *, *, #39624, .F. ) ;
#9152 = CARTESIAN_POINT ( 'NONE',  ( -27.70776136782869514, 0.2300040921888646395, -13.51576448074164993 ) ) ;
#9153 = CARTESIAN_POINT ( 'NONE',  ( 13.94482798346721175, 26.50521816028912525, 7.000000000000000000 ) ) ;
#9154 = EDGE_CURVE ( 'NONE', #36335, #7574, #912, .T. ) ;
#9155 = ORIENTED_EDGE ( 'NONE', *, *, #17474, .T. ) ;
#9156 = CARTESIAN_POINT ( 'NONE',  ( 26.10825148640684645, -4.601592950812219307, -17.92875175135799282 ) ) ;
#9157 = ADVANCED_FACE ( 'NONE', ( #23617 ), #9986, .T. ) ;
#9158 = EDGE_CURVE ( 'NONE', #33341, #22260, #20577, .T. ) ;
#9159 = ORIENTED_EDGE ( 'NONE', *, *, #35436, .T. ) ;
#9160 = CARTESIAN_POINT ( 'NONE',  ( 3.857345576530424758, 39.98449713665801397, 12.73282698324868711 ) ) ;
#9161 = AXIS2_PLACEMENT_3D ( 'NONE', #36957, #381, #9526 ) ;
#9162 = CARTESIAN_POINT ( 'NONE',  ( 11.45923940083702597, -19.42154971127180474, 20.25080042701502947 ) ) ;
#9163 = CYLINDRICAL_SURFACE ( 'NONE', #31243, 1.000000000000000888 ) ;
#9164 = CARTESIAN_POINT ( 'NONE',  ( 2.148627388802076599, 32.24135036777348517, 20.25080042701565475 ) ) ;
#9165 = CARTESIAN_POINT ( 'NONE',  ( -14.26585111513660031, 17.86474508437623143, 13.00000000000000178 ) ) ;
#9166 = VERTEX_POINT ( 'NONE', #5128 ) ;
#9167 = CARTESIAN_POINT ( 'NONE',  ( 9.356056665764066693, 26.06569820189703179, 10.50000000000000000 ) ) ;
#9168 = CARTESIAN_POINT ( 'NONE',  ( 32.33143948541791701, 1.358872982501826865, 0.000000000000000000 ) ) ;
#9169 = DIRECTION ( 'NONE',  ( 0.000000000000000000, -0.6445931928399465383, 0.7645257456386955752 ) ) ;
#9170 = DIRECTION ( 'NONE',  ( 0.000000000000000000, 0.000000000000000000, -1.000000000000000000 ) ) ;
#9171 = CARTESIAN_POINT ( 'NONE',  ( 5.041034891940512352, 25.97319188981542837, -18.71755947577446832 ) ) ;
#9172 = CIRCLE ( 'NONE', #21494, 17.00000000000000355 ) ;
#9173 = FACE_OUTER_BOUND ( 'NONE', #5151, .T. ) ;
#9174 = AXIS2_PLACEMENT_3D ( 'NONE', #7345, #13447, #19751 ) ;
#9175 = CARTESIAN_POINT ( 'NONE',  ( 16.28251897248971503, -25.35181217798053765, -11.46904951680661000 ) ) ;
#9176 = CARTESIAN_POINT ( 'NONE',  ( 14.97009266215792778, 21.42933399866928568, 10.49999999999999822 ) ) ;
#9177 = LINE ( 'NONE', #21563, #9926 ) ;
#9178 = FACE_BOUND ( 'NONE', #3838, .T. ) ;
#9179 = ADVANCED_FACE ( 'NONE', ( #17535 ), #29909, .T. ) ;
#9180 = ORIENTED_EDGE ( 'NONE', *, *, #34335, .F. ) ;
#9181 = CARTESIAN_POINT ( 'NONE',  ( -14.40426848691212847, 24.18477772179416974, -12.56146234885731872 ) ) ;
#9182 = CARTESIAN_POINT ( 'NONE',  ( -33.78274305024888946, -17.56282548559296330, 16.87380292611478438 ) ) ;
#9183 = CARTESIAN_POINT ( 'NONE',  ( 9.629772704453449350, -18.63330705237584439, -26.23951421163814501 ) ) ;
#9184 = AXIS2_PLACEMENT_3D ( 'NONE', #12786, #31875, #19087 ) ;
#9185 = CARTESIAN_POINT ( 'NONE',  ( -13.94482798346716557, 26.50521816028930289, 11.00000000000000000 ) ) ;
#9186 = ORIENTED_EDGE ( 'NONE', *, *, #19305, .T. ) ;
#9187 = ORIENTED_EDGE ( 'NONE', *, *, #2099, .F. ) ;
#9188 = CARTESIAN_POINT ( 'NONE',  ( -10.11312864869621286, 18.12346847508388237, -27.37340818524439001 ) ) ;
#9189 = CARTESIAN_POINT ( 'NONE',  ( -20.43668249186664454, -27.04690955953348208, -6.800953625143487002 ) ) ;
#9190 = CARTESIAN_POINT ( 'NONE',  ( 13.97557076678965693, 21.53386246193694475, 7.500000000000010658 ) ) ;
#9191 = ORIENTED_EDGE ( 'NONE', *, *, #21052, .T. ) ;
#9192 = CARTESIAN_POINT ( 'NONE',  ( -19.96736081760328574, -5.571863482751658658, -27.79030427704988071 ) ) ;
#9193 = CARTESIAN_POINT ( 'NONE',  ( -11.76341657271260743, -21.49608334009564814, -18.46619230194481887 ) ) ;
#9194 = CARTESIAN_POINT ( 'NONE',  ( -12.80736835487442349, 15.68301270189233954, 7.499999999999993783 ) ) ;
#9195 = ORIENTED_EDGE ( 'NONE', *, *, #39045, .F. ) ;
#9196 = CARTESIAN_POINT ( 'NONE',  ( 24.67560003803047408, 1.382580745444311088, -17.53657882121196465 ) ) ;
#9197 = CARTESIAN_POINT ( 'NONE',  ( -7.014595103779441843, 35.79644522156330311, 10.50000000000000355 ) ) ;
#9198 = DIRECTION ( 'NONE',  ( 0.000000000000000000, 0.000000000000000000, 1.000000000000000000 ) ) ;
#9199 = B_SPLINE_CURVE_WITH_KNOTS ( 'NONE', 3,
 ( #38809, #7519, #29665, #25811, #35564, #29062 ),
 .UNSPECIFIED., .F., .F.,
 ( 4, 2, 4 ),
 ( 0.000000000000000000, 0.5000000000000000000, 1.000000000000000000 ),
 .UNSPECIFIED. ) ;
#9200 = B_SPLINE_CURVE_WITH_KNOTS ( 'NONE', 3,
 ( #38497, #1530, #16364, #10673, #10466, #20019 ),
 .UNSPECIFIED., .F., .F.,
 ( 4, 2, 4 ),
 ( 0.000000000000000000, 0.5000000000000000000, 1.000000000000000000 ),
 .UNSPECIFIED. ) ;
#9201 = ORIENTED_EDGE ( 'NONE', *, *, #39040, .T. ) ;
#9202 = CARTESIAN_POINT ( 'NONE',  ( -22.74375665350138220, 0.5678067076679078617, -21.61155036081104086 ) ) ;
#9203 = VERTEX_POINT ( 'NONE', #40043 ) ;
#9204 = CARTESIAN_POINT ( 'NONE',  ( 32.43268799775532329, -2.266782117739180258, -7.289905317446092603 ) ) ;
#9205 = VECTOR ( 'NONE', #9918, 1000.000000000000227 ) ;
#9206 = CARTESIAN_POINT ( 'NONE',  ( -12.11431921870781281, -16.53859995802357474, -30.00000000000001066 ) ) ;
#9207 = CARTESIAN_POINT ( 'NONE',  ( 15.74227866053861469, -25.75916161678320648, 17.42190598798392642 ) ) ;
#9208 = EDGE_CURVE ( 'NONE', #26791, #30382, #21050, .T. ) ;
#9209 = VERTEX_POINT ( 'NONE', #27659 ) ;
#9210 = CARTESIAN_POINT ( 'NONE',  ( -20.30511407948876013, 2.906241227738919353, -29.99999999999999645 ) ) ;
#9211 = FACE_OUTER_BOUND ( 'NONE', #15019, .T. ) ;
#9212 = CARTESIAN_POINT ( 'NONE',  ( 13.24038105676655164, 15.43301270189216368, 11.00000000000000000 ) ) ;
#9213 = CARTESIAN_POINT ( 'NONE',  ( -6.354454053420243831, 35.54304081427989814, 7.000000000000000000 ) ) ;
#9214 = AXIS2_PLACEMENT_3D ( 'NONE', #2759, #33260, #26946 ) ;
#9215 = CARTESIAN_POINT ( 'NONE',  ( 13.05736835487433467, 16.11602540378438420, 11.00000000000000000 ) ) ;
#9216 = FACE_BOUND ( 'NONE', #34566, .T. ) ;
#9217 = CARTESIAN_POINT ( 'NONE',  ( 18.17912400184410160, 22.26280294335838406, 13.92931973826196490 ) ) ;
#9218 = ORIENTED_EDGE ( 'NONE', *, *, #355, .F. ) ;
#9219 = CARTESIAN_POINT ( 'NONE',  ( -23.53005843440588052, 6.935657865434798452, -12.82094700181943558 ) ) ;
#9220 = CARTESIAN_POINT ( 'NONE',  ( 15.02235689379175732, 21.92659494635341844, 11.00000000000000000 ) ) ;
#9221 = CARTESIAN_POINT ( 'NONE',  ( 0.6417673702184640838, 33.31072022568110924, 6.000000000000000000 ) ) ;
#9222 = CARTESIAN_POINT ( 'NONE',  ( 15.12372412105587571, -15.73678478649937595, -24.44085377604933029 ) ) ;
#9223 = CARTESIAN_POINT ( 'NONE',  ( 5.473344025737212348, 14.11593743010426572, 10.49999999999999822 ) ) ;
#9224 = CARTESIAN_POINT ( 'NONE',  ( 10.82761120373386099, 17.56290797765107925, -28.06474652081093879 ) ) ;
#9225 = ORIENTED_EDGE ( 'NONE', *, *, #27995, .F. ) ;
#9226 = CARTESIAN_POINT ( 'NONE',  ( -12.87412475669415102, 16.08929808775789638, -28.17534248950969200 ) ) ;
#9227 = AXIS2_PLACEMENT_3D ( 'NONE', #5722, #27660, #27862 ) ;
#9228 = CARTESIAN_POINT ( 'NONE',  ( -20.82679924176412811, -18.60878591099491786, 20.82122704794066337 ) ) ;
#9229 = EDGE_CURVE ( 'NONE', #35064, #10849, #39649, .T. ) ;
#9230 = CARTESIAN_POINT ( 'NONE',  ( -10.16521142134453548, 24.66068167190384841, 13.00000000000000178 ) ) ;
#9231 = CARTESIAN_POINT ( 'NONE',  ( 11.91420444604188233, 19.35880423362332436, -21.62089463913763865 ) ) ;
#9232 = ORIENTED_EDGE ( 'NONE', *, *, #31119, .T. ) ;
#9233 = DIRECTION ( 'NONE',  ( -0.000000000000000000, -0.000000000000000000, -1.000000000000000000 ) ) ;
#9234 = ORIENTED_EDGE ( 'NONE', *, *, #29646, .F. ) ;
#9236 = CARTESIAN_POINT ( 'NONE',  ( -4.706342468480190000, 20.64589803375067945, 6.000000000000000000 ) ) ;
#9235 = CARTESIAN_POINT ( 'NONE',  ( -10.88833724461483321, 17.42332960106011797, -28.70205193506265573 ) ) ;
#9237 = CARTESIAN_POINT ( 'NONE',  ( -13.19604288844774054, -23.10384307990375419, -15.43186663979633977 ) ) ;
#9238 = DIRECTION ( 'NONE',  ( -0.9135454576426046414, -0.4067366430757919371, 0.000000000000000000 ) ) ;
#9239 = CARTESIAN_POINT ( 'NONE',  ( -18.98149992151875054, -9.954718304477847113, -25.58083087282487611 ) ) ;
#9240 = CARTESIAN_POINT ( 'NONE',  ( -8.776592290562826193, -18.65192578191585326, -28.11862783572077618 ) ) ;
#9241 = CARTESIAN_POINT ( 'NONE',  ( 14.31603901957230462, 19.98981538725069740, 11.00000000000000000 ) ) ;
#9242 = CARTESIAN_POINT ( 'NONE',  ( 14.89222191165484155, 22.99967983981807862, -12.60792089205823174 ) ) ;
#9243 = ADVANCED_FACE ( 'NONE', ( #24412 ), #8977, .T. ) ;
#9244 = VERTEX_POINT ( 'NONE', #9176 ) ;
#9245 = CARTESIAN_POINT ( 'NONE',  ( 26.63862888549859065, 4.673691467239231123, -6.432048232843499136 ) ) ;
#9246 = CARTESIAN_POINT ( 'NONE',  ( 10.10646936306337729, 32.94553861768082470, 7.000000000000000000 ) ) ;
#9247 = AXIS2_PLACEMENT_3D ( 'NONE', #19690, #37979, #9950 ) ;
#9248 = DIRECTION ( 'NONE',  ( 0.9510565162951504226, -0.3090169943749573322, 0.000000000000000000 ) ) ;
#9249 = ADVANCED_FACE ( 'NONE', ( #6118 ), #9579, .F. ) ;
#9250 = CARTESIAN_POINT ( 'NONE',  ( -18.98517864108453068, -25.27528660209288702, -11.33194676435389248 ) ) ;
#9251 = ORIENTED_EDGE ( 'NONE', *, *, #24548, .F. ) ;
#9252 = CARTESIAN_POINT ( 'NONE',  ( -21.06315986593275369, -0.5327104372337403415, -26.10652535518945427 ) ) ;
#9253 = CARTESIAN_POINT ( 'NONE',  ( 26.72259468233993118, -0.05410243562783979832, -15.41034757420027290 ) ) ;
#9254 = CIRCLE ( 'NONE', #37144, 6.000000000000014211 ) ;
#9255 = CARTESIAN_POINT ( 'NONE',  ( -38.62508484777313811, -17.24896845009202551, 11.00000000000000355 ) ) ;
#9256 = CARTESIAN_POINT ( 'NONE',  ( 26.01028601707371379, -6.099477938990075288, 20.69868183039873699 ) ) ;
#9257 = ORIENTED_EDGE ( 'NONE', *, *, #7539, .F. ) ;
#9258 = CARTESIAN_POINT ( 'NONE',  ( 33.62187204924162387, 0.04418559750794539415, -5.000000000000000000 ) ) ;
#9259 = DIRECTION ( 'NONE',  ( -1.000000000000000000, 0.000000000000000000, 0.000000000000000000 ) ) ;
#9260 = EDGE_LOOP ( 'NONE', ( #1441, #6565, #16317, #17399 ) ) ;
#9261 = EDGE_CURVE ( 'NONE', #1897, #4338, #15669, .T. ) ;
#9262 = CARTESIAN_POINT ( 'NONE',  ( 6.688300058587269170, 16.47782454277055564, 13.00000000000000178 ) ) ;
#9263 = VECTOR ( 'NONE', #27940, 1000.000000000000000 ) ;
#9264 = VECTOR ( 'NONE', #4974, 1000.000000000000000 ) ;
#9265 = DIRECTION ( 'NONE',  ( -0.000000000000000000, -0.000000000000000000, 1.000000000000000000 ) ) ;
#9266 = CARTESIAN_POINT ( 'NONE',  ( 13.99633081586303796, 26.34670874090659609, 10.83333333333333215 ) ) ;
#9267 = CARTESIAN_POINT ( 'NONE',  ( 1.444440266932477401, 20.45847851156178265, -30.00000000000001066 ) ) ;
#9268 = CARTESIAN_POINT ( 'NONE',  ( -13.58430815669637859, 27.61478409596699279, 10.83333333333333570 ) ) ;
#9269 = CARTESIAN_POINT ( 'NONE',  ( 13.22516817658079802, 40.70288237343621063, 7.000000000000000000 ) ) ;
#9270 = AXIS2_PLACEMENT_3D ( 'NONE', #7170, #22612, #10429 ) ;
#9271 = LINE ( 'NONE', #22442, #11663 ) ;
#9272 = DIRECTION ( 'NONE',  ( 1.224646799147351235E-16, -1.000000000000000000, -0.000000000000000000 ) ) ;
#9273 = CARTESIAN_POINT ( 'NONE',  ( 7.096882951594525757, 29.56287847632727050, 10.50000000000000000 ) ) ;
#9274 = LINE ( 'NONE', #33674, #17137 ) ;
#9275 = CARTESIAN_POINT ( 'NONE',  ( 15.09524128205707072, 27.81033699783984403, -5.000000000000000000 ) ) ;
#9276 = DIRECTION ( 'NONE',  ( -0.8660254037844432595, -0.4999999999999920064, 0.000000000000000000 ) ) ;
#9277 = ORIENTED_EDGE ( 'NONE', *, *, #30760, .F. ) ;
#9278 = AXIS2_PLACEMENT_3D ( 'NONE', #898, #4545, #13480 ) ;
#9280 = CARTESIAN_POINT ( 'NONE',  ( 11.41267482483262619, 26.20820393249957192, 13.00000000000000178 ) ) ;
#9279 = CARTESIAN_POINT ( 'NONE',  ( -15.96198011527028626, 14.19337421597026605, -23.24198305949962418 ) ) ;
#9281 = CARTESIAN_POINT ( 'NONE',  ( 11.44473057578109199, 31.45924896672603310, 10.50000000000000178 ) ) ;
#9282 = CARTESIAN_POINT ( 'NONE',  ( 9.694524255575014848, -18.43926002963515742, -26.83009326277129603 ) ) ;
#9283 = CARTESIAN_POINT ( 'NONE',  ( -13.37002884985804840, -17.04744882218747648, -24.61733060730478684 ) ) ;
#9284 = CARTESIAN_POINT ( 'NONE',  ( 15.36806905513554788, 26.68643454456317698, -6.416988418440872088 ) ) ;
#9285 = CARTESIAN_POINT ( 'NONE',  ( 12.92457025990295527, 21.65936192259344750, -17.43674491296770057 ) ) ;
#9286 = ORIENTED_EDGE ( 'NONE', *, *, #6931, .T. ) ;
#9287 = CARTESIAN_POINT ( 'NONE',  ( -1.247473515615844075, 16.63111439559750693, 13.00000000000000178 ) ) ;
#9288 = EDGE_CURVE ( 'NONE', #19542, #8554, #6584, .T. ) ;
#9289 = CARTESIAN_POINT ( 'NONE',  ( -15.29737515392600322, -26.57080565899713775, -6.888077247771704492 ) ) ;
#9290 = CONICAL_SURFACE ( 'NONE', #13830, 1.000000000000011324, 0.7853981633974549403 ) ;
#9291 = CARTESIAN_POINT ( 'NONE',  ( -36.01431143412934688, -5.340261033854917017, 13.92931973827854719 ) ) ;
#9292 = CARTESIAN_POINT ( 'NONE',  ( -29.90225311088989812, -23.39525860678804037, -5.000000000000006217 ) ) ;
#9293 = CIRCLE ( 'NONE', #30055, 1.000000000000000000 ) ;
#9294 = CARTESIAN_POINT ( 'NONE',  ( -0.3741226908721868027, -24.24193228020686064, -10.38565774725202928 ) ) ;
#9295 = CARTESIAN_POINT ( 'NONE',  ( 11.19848097534155684, 17.17100607549662072, -29.35292330717537368 ) ) ;
#9296 = CARTESIAN_POINT ( 'NONE',  ( 22.78013759795664939, 10.15463924895263226, -5.966147905284203468 ) ) ;
#9297 = LINE ( 'NONE', #19229, #34841 ) ;
#9298 = ADVANCED_FACE ( 'NONE', ( #21562 ), #15870, .F. ) ;
#9299 = CARTESIAN_POINT ( 'NONE',  ( -5.301386336604020144, 37.38718629579432928, -6.707813491147157414 ) ) ;
#9300 = AXIS2_PLACEMENT_3D ( 'NONE', #11908, #30200, #24491 ) ;
#9301 = ORIENTED_EDGE ( 'NONE', *, *, #10524, .F. ) ;
#9302 = CARTESIAN_POINT ( 'NONE',  ( -23.51180566201336930, -4.338079614371764592, -21.05291888185874427 ) ) ;
#9303 = AXIS2_PLACEMENT_3D ( 'NONE', #25547, #28004, #19656 ) ;
#9304 = CARTESIAN_POINT ( 'NONE',  ( -19.89620541518657859, 17.40116461633755307, 14.53008259253898693 ) ) ;
#9305 = EDGE_LOOP ( 'NONE', ( #20390, #27864, #26888, #2883 ) ) ;
#9306 = DIRECTION ( 'NONE',  ( 0.9945218953682742891, 0.1045284632676437425, -0.000000000000000000 ) ) ;
#9307 = FACE_OUTER_BOUND ( 'NONE', #28594, .T. ) ;
#9308 = CARTESIAN_POINT ( 'NONE',  ( -29.40640376299546688, 0.6751206212795356487, -9.249095237612971587 ) ) ;
#9309 = CARTESIAN_POINT ( 'NONE',  ( 21.49173964087244570, -7.212581857489289483, -23.10824091391128476 ) ) ;
#9310 = CIRCLE ( 'NONE', #32005, 1.000000000000000000 ) ;
#9311 = EDGE_LOOP ( 'NONE', ( #34775, #17167, #38553, #29028, #33776, #23985, #35306 ) ) ;
#9312 = EDGE_CURVE ( 'NONE', #31096, #31127, #27387, .T. ) ;
#9313 = CARTESIAN_POINT ( 'NONE',  ( -8.633502029282189127, 11.46765470489704342, 10.00000000000000000 ) ) ;
#9314 = VERTEX_POINT ( 'NONE', #18919 ) ;
#9315 = EDGE_CURVE ( 'NONE', #19145, #23249, #15068, .T. ) ;
#9316 = CARTESIAN_POINT ( 'NONE',  ( 0.7500000000000004441, 33.00000000000000000, 10.75000000000000000 ) ) ;
#9317 = CARTESIAN_POINT ( 'NONE',  ( 20.57678504259613561, 23.15270735499986898, 22.99999999999999645 ) ) ;
#9318 = AXIS2_PLACEMENT_3D ( 'NONE', #33228, #1943, #27114 ) ;
#9319 = PLANE ( 'NONE',  #31147 ) ;
#9320 = ORIENTED_EDGE ( 'NONE', *, *, #22924, .F. ) ;
#9321 = AXIS2_PLACEMENT_3D ( 'NONE', #35044, #19598, #31993 ) ;
#9322 = CARTESIAN_POINT ( 'NONE',  ( -2.282314974550741837, 20.78572398550833000, -26.98632778830081236 ) ) ;
#9323 = FACE_OUTER_BOUND ( 'NONE', #3407, .T. ) ;
#9324 = LINE ( 'NONE', #34108, #14396 ) ;
#9325 = CARTESIAN_POINT ( 'NONE',  ( 0.000000000000000000, 22.50000000000000355, 7.000000000000000000 ) ) ;
#9326 = CARTESIAN_POINT ( 'NONE',  ( 22.88038781354014262, -17.60680147475983759, -16.66587105011879544 ) ) ;
#9327 = CARTESIAN_POINT ( 'NONE',  ( 17.03883565536520450, 14.60776677102190213, -18.99045918486842410 ) ) ;
#9328 = AXIS2_PLACEMENT_3D ( 'NONE', #12518, #37700, #31205 ) ;
#9329 = CARTESIAN_POINT ( 'NONE',  ( 12.90021850856434327, 31.07188364411424786, -8.136059182505970711 ) ) ;
#9330 = ORIENTED_EDGE ( 'NONE', *, *, #30869, .F. ) ;
#9331 = CARTESIAN_POINT ( 'NONE',  ( -20.43794256383087671, 11.06939829604054992, -14.91976663991167662 ) ) ;
#9332 = CARTESIAN_POINT ( 'NONE',  ( 0.5415361484146484772, 27.50000000000004974, 23.00000000000000000 ) ) ;
#9333 =( GEOMETRIC_REPRESENTATION_CONTEXT ( 3 ) GLOBAL_UNCERTAINTY_ASSIGNED_CONTEXT ( ( #29484 ) ) GLOBAL_UNIT_ASSIGNED_CONTEXT ( ( #33951, #22743, #818 ) ) REPRESENTATION_CONTEXT ( 'NONE', 'WORKASPACE' ) );
#9334 = CARTESIAN_POINT ( 'NONE',  ( 10.61757206484970517, -19.55229676520039561, -22.72432018335026171 ) ) ;
#9335 = CARTESIAN_POINT ( 'NONE',  ( -2.587667106213709101, 35.31811204475769728, 12.00000000000000000 ) ) ;
#9336 = CARTESIAN_POINT ( 'NONE',  ( -11.41987377193683528, -19.41918266173334828, -30.00000000000000000 ) ) ;
#9337 = ADVANCED_FACE ( 'NONE', ( #3078 ), #2862, .T. ) ;
#9338 = DIRECTION ( 'NONE',  ( 0.1045284632676569680, 0.9945218953682729568, -0.000000000000000000 ) ) ;
#9339 = CARTESIAN_POINT ( 'NONE',  ( -11.66966591706341383, 18.92733846212934878, -22.73230586722390356 ) ) ;
#9340 = CARTESIAN_POINT ( 'NONE',  ( -19.41909531571028324, -23.12033621153826957, -14.04196714719246231 ) ) ;
#9341 = CARTESIAN_POINT ( 'NONE',  ( 9.856402666990103256, -24.08899994559548574, -12.70246950836210331 ) ) ;
#9342 = CARTESIAN_POINT ( 'NONE',  ( 11.46110508464496824, 32.14680900553369014, 10.68306113187827933 ) ) ;
#9343 = ORIENTED_EDGE ( 'NONE', *, *, #12440, .F. ) ;
#9344 = CARTESIAN_POINT ( 'NONE',  ( -8.712598976131317841, 26.30495431820440899, -16.88202031406565240 ) ) ;
#9345 = CARTESIAN_POINT ( 'NONE',  ( 0.5000000000000000000, 37.18846563620834189, 10.96580507645519909 ) ) ;
#9346 = CARTESIAN_POINT ( 'NONE',  ( -0.2655091840902661926, 8.754836972118123839, 6.000000000000000000 ) ) ;
#9347 = CONICAL_SURFACE ( 'NONE', #14538, 1.000000000000004441, 0.7853981633974522758 ) ;
#9348 = CARTESIAN_POINT ( 'NONE',  ( 0.6108529249775871417, 37.48755679569043053, 7.500000000000000888 ) ) ;
#9349 = ORIENTED_EDGE ( 'NONE', *, *, #16852, .F. ) ;
#9350 = CARTESIAN_POINT ( 'NONE',  ( 20.52661814301616161, 0.8646301841086654338, -28.70720715481454377 ) ) ;
#9351 = CARTESIAN_POINT ( 'NONE',  ( -1.732915686479672868, 38.50000000000000711, -4.999999999999999112 ) ) ;
#9352 = DIRECTION ( 'NONE',  ( 0.000000000000000000, 0.000000000000000000, -1.000000000000000000 ) ) ;
#9353 = B_SPLINE_SURFACE_WITH_KNOTS ( 'NONE', 1, 3, ( 
 ( #15037, #3046, #30490, #11795, #6089, #30288, #27430, #33932, #24585, #37175 ),
 ( #5691, #18102, #21727, #24777, #34135, #40012, #24181, #17904, #6286, #18296 ) ),
 .UNSPECIFIED., .F., .F., .F.,
 ( 2, 2 ),
 ( 4, 2, 2, 2, 4 ),
 ( 0.000000000000000000, 1.000000000000000000 ),
 ( -1.096214744126235097, -0.7035156624275106241, -0.3108165807287861515, 0.08188250096993832106, 0.4745815826686627936 ),
 .UNSPECIFIED. ) ;
#9354 = EDGE_LOOP ( 'NONE', ( #9915, #39060, #34537 ) ) ;
#9355 = CARTESIAN_POINT ( 'NONE',  ( -20.48102978849703604, 0.8817738089609830077, -29.34878050620392642 ) ) ;
#9356 = CYLINDRICAL_SURFACE ( 'NONE', #30008, 6.000000000000001776 ) ;
#9357 = VERTEX_POINT ( 'NONE', #31307 ) ;
#9358 = CARTESIAN_POINT ( 'NONE',  ( 26.18805396461011981, -5.413810846952083367, -17.87313096885579355 ) ) ;
#9359 = AXIS2_PLACEMENT_3D ( 'NONE', #7769, #20171, #32568 ) ;
#9360 = ORIENTED_EDGE ( 'NONE', *, *, #30488, .T. ) ;
#9361 = LINE ( 'NONE', #12576, #10307 ) ;
#9362 = MANIFOLD_SOLID_BREP ( 'Extrude-Thin3', #11266 ) ;
#9363 = CARTESIAN_POINT ( 'NONE',  ( -9.237168799398533636, 37.83823547837186396, 12.73282698324810625 ) ) ;
#9364 = CARTESIAN_POINT ( 'NONE',  ( 1.204925152852602155, 12.02153850147726999, 11.00000000000000000 ) ) ;
#9365 = LINE ( 'NONE', #31100, #33209 ) ;
#9366 = ADVANCED_FACE ( 'NONE', ( #19511 ), #27860, .F. ) ;
#9367 = CARTESIAN_POINT ( 'NONE',  ( -10.03134041160988943, 26.49437744576609788, 19.99202127657076744 ) ) ;
#9368 = CIRCLE ( 'NONE', #6735, 6.000000000000003553 ) ;
#9369 = CARTESIAN_POINT ( 'NONE',  ( 10.77090408390491127, 15.39748370681878775, 13.00000000000000178 ) ) ;
#9370 = ORIENTED_EDGE ( 'NONE', *, *, #19463, .F. ) ;
#9371 = CARTESIAN_POINT ( 'NONE',  ( 3.574287532905564557, 8.089166425130672522, 10.87262190629281022 ) ) ;
#9372 = CARTESIAN_POINT ( 'NONE',  ( -10.34254640628272348, 25.37474234119853023, 19.99202127657103745 ) ) ;
#9373 = CARTESIAN_POINT ( 'NONE',  ( 12.63210941633768947, 14.41074797273250496, 7.485699520496975623 ) ) ;
#9374 = DIRECTION ( 'NONE',  ( 1.000000000000000000, 0.000000000000000000, 0.000000000000000000 ) ) ;
#9375 = CARTESIAN_POINT ( 'NONE',  ( 6.036156669524302743, 23.50249717186115106, -20.88789013247724924 ) ) ;
#9376 = CARTESIAN_POINT ( 'NONE',  ( 16.74105887149018201, -25.99454892381202598, -10.07209973717082008 ) ) ;
#9377 = CARTESIAN_POINT ( 'NONE',  ( -12.67493120981686516, 14.45362483784325924, 10.49999999999999822 ) ) ;
#9378 = ADVANCED_FACE ( 'NONE', ( #9777 ), #29061, .F. ) ;
#9379 = AXIS2_PLACEMENT_3D ( 'NONE', #39998, #39606, #11978 ) ;
#9380 = ORIENTED_EDGE ( 'NONE', *, *, #34744, .T. ) ;
#9381 = CARTESIAN_POINT ( 'NONE',  ( -13.50669571649333456, 22.78588612237093614, -15.45264257089643500 ) ) ;
#9382 = CARTESIAN_POINT ( 'NONE',  ( -31.31527935466932888, -1.911037205182263943, 17.42190598798389800 ) ) ;
#9383 = CARTESIAN_POINT ( 'NONE',  ( 14.22552846898557632, -25.04752998104490302, -11.60275637146618344 ) ) ;
#9384 = EDGE_CURVE ( 'NONE', #33679, #31336, #17819, .T. ) ;
#9385 = CARTESIAN_POINT ( 'NONE',  ( 3.503793317224329851, 8.420815634768676006, 7.499999999999990230 ) ) ;
#9386 = ORIENTED_EDGE ( 'NONE', *, *, #13443, .T. ) ;
#9387 = VERTEX_POINT ( 'NONE', #4480 ) ;
#9388 = CARTESIAN_POINT ( 'NONE',  ( -12.03032039410056697, 24.14510420486799092, -16.21622471958081491 ) ) ;
#9389 = CIRCLE ( 'NONE', #405, 1.000000000000000000 ) ;
#9390 = CARTESIAN_POINT ( 'NONE',  ( -19.71199086647830967, -26.17691209112436113, -9.501020231640085356 ) ) ;
#9391 = FACE_BOUND ( 'NONE', #24982, .T. ) ;
#9392 = CIRCLE ( 'NONE', #32096, 15.00000000000000000 ) ;
#9393 = EDGE_LOOP ( 'NONE', ( #7135, #3014, #33637, #34960 ) ) ;
#9394 = ADVANCED_FACE ( 'NONE', ( #22960 ), #25602, .T. ) ;
#9395 = CARTESIAN_POINT ( 'NONE',  ( -27.12574315244719614, -8.434033646970773290, -16.74782370223186589 ) ) ;
#9396 = CARTESIAN_POINT ( 'NONE',  ( -11.30698307648105860, -21.00710847950110249, -19.52216458991920689 ) ) ;
#9397 = CARTESIAN_POINT ( 'NONE',  ( -3.503793317224518145, 8.420815634768723967, 7.000000000000000000 ) ) ;
#9398 = EDGE_LOOP ( 'NONE', ( #38012, #13522, #30840, #28037 ) ) ;
#9399 = CARTESIAN_POINT ( 'NONE',  ( 30.47359799298996208, 0.2308879069823202845, -6.888633799088443865 ) ) ;
#9400 = DIRECTION ( 'NONE',  ( 1.000000000000000000, 0.000000000000000000, 0.000000000000000000 ) ) ;
#9401 = DIRECTION ( 'NONE',  ( 1.000000000000000000, 0.000000000000000000, 0.000000000000000000 ) ) ;
#9402 = ORIENTED_EDGE ( 'NONE', *, *, #3945, .F. ) ;
#9403 = CARTESIAN_POINT ( 'NONE',  ( -20.48278845350746380, 0.8398715278162421916, -30.00000000000000000 ) ) ;
#9404 = ORIENTED_EDGE ( 'NONE', *, *, #24047, .T. ) ;
#9405 = CARTESIAN_POINT ( 'NONE',  ( 32.32777460232222211, -1.841093328404687313, -6.383748192902252150 ) ) ;
#9406 = CARTESIAN_POINT ( 'NONE',  ( 24.08646667827958154, -13.28101593840524153, 20.99999999999998934 ) ) ;
#9407 = CARTESIAN_POINT ( 'NONE',  ( 28.56250045050212805, -21.55178514600707373, 18.42518152272109333 ) ) ;
#9408 = ORIENTED_EDGE ( 'NONE', *, *, #34109, .T. ) ;
#9409 = CARTESIAN_POINT ( 'NONE',  ( -20.13976743542029979, 4.300193810599860278, -28.21449245398771666 ) ) ;
#9410 = EDGE_CURVE ( 'NONE', #3673, #21094, #36646, .T. ) ;
#9411 = CARTESIAN_POINT ( 'NONE',  ( -14.52537758579311067, 26.24401664712872062, 7.365694256298322529 ) ) ;
#9412 = EDGE_CURVE ( 'NONE', #18297, #7799, #4654, .T. ) ;
#9413 = AXIS2_PLACEMENT_3D ( 'NONE', #5034, #8078, #36122 ) ;
#9414 = CARTESIAN_POINT ( 'NONE',  ( 4.672335726383261445, 24.36080358023195913, 20.99999999999999645 ) ) ;
#9415 = CARTESIAN_POINT ( 'NONE',  ( 13.16028273094469014, 27.30176617939681449, 7.500000000000000888 ) ) ;
#9416 = DIRECTION ( 'NONE',  ( 1.000000000000000000, 0.000000000000000000, 0.000000000000000000 ) ) ;
#9417 = AXIS2_PLACEMENT_3D ( 'NONE', #5708, #5311, #18118 ) ;
#9418 = AXIS2_PLACEMENT_3D ( 'NONE', #40190, #2823, #17682 ) ;
#9419 = VECTOR ( 'NONE', #2744, 1000.000000000000000 ) ;
#9420 = DIRECTION ( 'NONE',  ( 1.000000000000000000, 0.000000000000000000, 0.000000000000000000 ) ) ;
#9421 = FACE_OUTER_BOUND ( 'NONE', #8457, .T. ) ;
#9422 = CARTESIAN_POINT ( 'NONE',  ( -24.83346892669243289, 7.119045183397740395, -5.960013684747799800 ) ) ;
#9423 = DIRECTION ( 'NONE',  ( -0.2876062384759393020, -0.6459741880212640508, -0.7071067811865402453 ) ) ;
#9424 = DIRECTION ( 'NONE',  ( 0.000000000000000000, 0.000000000000000000, 1.000000000000000000 ) ) ;
#9425 = CARTESIAN_POINT ( 'NONE',  ( 22.95410551231090679, -26.66747533545364135, -6.768454890417195280 ) ) ;
#9426 = LINE ( 'NONE', #27509, #14420 ) ;
#9427 = EDGE_CURVE ( 'NONE', #15350, #19729, #31904, .T. ) ;
#9428 = CARTESIAN_POINT ( 'NONE',  ( 15.13821314949306185, 26.72040169015227562, -7.817432155278004835 ) ) ;
#9429 = EDGE_LOOP ( 'NONE', ( #37713, #27908, #5387, #15996 ) ) ;
#9430 = CARTESIAN_POINT ( 'NONE',  ( -14.26164166507406605, 20.40696190269933297, -16.59697255856162101 ) ) ;
#9431 = CARTESIAN_POINT ( 'NONE',  ( -26.87422832650623405, -16.65342898056120191, 20.50957957746005889 ) ) ;
#9432 = EDGE_CURVE ( 'NONE', #253, #17719, #24316, .T. ) ;
#9433 = DIRECTION ( 'NONE',  ( -0.000000000000000000, -0.000000000000000000, -1.000000000000000000 ) ) ;
#9434 = CARTESIAN_POINT ( 'NONE',  ( 15.31765784529594931, 26.43575136356594157, -7.358154011196789135 ) ) ;
#9435 = EDGE_LOOP ( 'NONE', ( #19856, #15033, #34938, #24783, #141 ) ) ;
#9436 = LINE ( 'NONE', #24669, #21614 ) ;
#9437 = EDGE_LOOP ( 'NONE', ( #3959, #8838, #21772, #13764 ) ) ;
#9439 = CARTESIAN_POINT ( 'NONE',  ( -12.83926296998453154, 26.67172942406192604, 7.000000000000000000 ) ) ;
#9438 = CARTESIAN_POINT ( 'NONE',  ( -11.07006266871842470, 17.83849166442784906, -26.21249532911198088 ) ) ;
#9440 = CARTESIAN_POINT ( 'NONE',  ( -15.39884463545014626, -26.43030500914523628, -7.822979998916790301 ) ) ;
#9441 = CARTESIAN_POINT ( 'NONE',  ( 12.74038105676659249, 14.56698729810780613, 10.59344459855566889 ) ) ;
#9442 = AXIS2_PLACEMENT_3D ( 'NONE', #23779, #32937, #20749 ) ;
#9443 = ORIENTED_EDGE ( 'NONE', *, *, #34083, .F. ) ;
#9444 = CARTESIAN_POINT ( 'NONE',  ( -21.03375321176811852, -11.02753040179103472, -21.84322230830700562 ) ) ;
#9445 = CARTESIAN_POINT ( 'NONE',  ( -13.92516281751823470, -26.33641981794989917, -5.946789951340505809 ) ) ;
#9446 = DIRECTION ( 'NONE',  ( 0.000000000000000000, 0.000000000000000000, 1.000000000000000000 ) ) ;
#9447 = CARTESIAN_POINT ( 'NONE',  ( 16.80931989995731968, 22.07997525327169086, -6.903476050494520955 ) ) ;
#9448 = ORIENTED_EDGE ( 'NONE', *, *, #8046, .T. ) ;
#9449 = CARTESIAN_POINT ( 'NONE',  ( 20.02244736892210497, 5.216203046238859997, -27.08051660729452692 ) ) ;
#9450 = CARTESIAN_POINT ( 'NONE',  ( -8.917741276437942233, 30.52956727630665057, 12.00000000000000000 ) ) ;
#9451 = DIRECTION ( 'NONE',  ( -1.000000000000000000, 0.000000000000000000, 0.000000000000000000 ) ) ;
#9452 = DIRECTION ( 'NONE',  ( 0.000000000000000000, 0.000000000000000000, 1.000000000000000000 ) ) ;
#9453 = AXIS2_PLACEMENT_3D ( 'NONE', #32830, #2347, #23472 ) ;
#9454 = ORIENTED_EDGE ( 'NONE', *, *, #35662, .T. ) ;
#9455 = CARTESIAN_POINT ( 'NONE',  ( -21.83110320996402010, 0.04483480959028030011, -23.77064350941624582 ) ) ;
#9456 = CARTESIAN_POINT ( 'NONE',  ( 31.24124332302707785, -0.3963250197696455701, -5.000000000000000888 ) ) ;
#9457 = CIRCLE ( 'NONE', #35401, 0.4999999999999997780 ) ;
#9458 = AXIS2_PLACEMENT_3D ( 'NONE', #21135, #11398, #30489 ) ;
#9459 = CARTESIAN_POINT ( 'NONE',  ( -5.537830610278340338, 36.16746786612513631, 10.94387467463486452 ) ) ;
#9460 = CARTESIAN_POINT ( 'NONE',  ( 18.28744585352691132, -19.47582948098743216, 20.69868183039766407 ) ) ;
#9461 = EDGE_LOOP ( 'NONE', ( #6938, #26733, #12735, #21537 ) ) ;
#9462 = CARTESIAN_POINT ( 'NONE',  ( 26.31271763591405133, -28.25584584496056806, -4.999999999999990230 ) ) ;
#9463 = DIRECTION ( 'NONE',  ( 1.000000000000000000, 0.000000000000000000, 0.000000000000000000 ) ) ;
#9464 = ORIENTED_EDGE ( 'NONE', *, *, #5871, .F. ) ;
#9465 = EDGE_CURVE ( 'NONE', #20052, #31246, #11990, .T. ) ;
#9466 = DIRECTION ( 'NONE',  ( 1.000000000000000000, 0.000000000000000000, -0.000000000000000000 ) ) ;
#9467 = CARTESIAN_POINT ( 'NONE',  ( -20.57678504272164943, 23.15270735504455146, 11.00000000000000000 ) ) ;
#9468 = LINE ( 'NONE', #28145, #9954 ) ;
#9469 = CARTESIAN_POINT ( 'NONE',  ( 2.331359131675258212, 32.30025893414131133, -13.81255405787268487 ) ) ;
#9470 = DIRECTION ( 'NONE',  ( -1.000000000000000000, 0.000000000000000000, 0.000000000000000000 ) ) ;
#9471 = CARTESIAN_POINT ( 'NONE',  ( 1.278175571583998860, 14.08178954835375940, 9.000000000000001776 ) ) ;
#9472 = CYLINDRICAL_SURFACE ( 'NONE', #22649, 1.000000000000000888 ) ;
#9473 = AXIS2_PLACEMENT_3D ( 'NONE', #25448, #7365, #31554 ) ;
#9474 = CARTESIAN_POINT ( 'NONE',  ( -1.623738443162547007, 19.56555719779890978, 6.000000000000000000 ) ) ;
#9475 = DIRECTION ( 'NONE',  ( -0.2185080122244101586, -0.6724985119639573794, -0.7071067811865475727 ) ) ;
#9476 = CARTESIAN_POINT ( 'NONE',  ( 2.118671991557230516, 37.17221401100731981, 6.000000000000000000 ) ) ;
#9477 = CARTESIAN_POINT ( 'NONE',  ( 14.09416554623298090, 26.10268081555338782, -11.51672208091659400 ) ) ;
#9479 = AXIS2_PLACEMENT_3D ( 'NONE', #1995, #20683, #1787 ) ;
#9478 = CARTESIAN_POINT ( 'NONE',  ( -6.789317288263781336, 35.87572455244716707, 7.455686640544902488 ) ) ;
#9480 = ORIENTED_EDGE ( 'NONE', *, *, #10443, .T. ) ;
#9483 = VECTOR ( 'NONE', #10280, 1000.000000000000000 ) ;
#9482 = CARTESIAN_POINT ( 'NONE',  ( 13.01837422881150452, 21.26636931122159169, 6.000000000000000000 ) ) ;
#9481 = CARTESIAN_POINT ( 'NONE',  ( -16.01922876754991876, 15.59330759611457218, -19.98676936076589428 ) ) ;
#9484 = FACE_OUTER_BOUND ( 'NONE', #11024, .T. ) ;
#9485 = AXIS2_PLACEMENT_3D ( 'NONE', #19876, #14378, #4632 ) ;
#9486 = CARTESIAN_POINT ( 'NONE',  ( 15.46971733045241670, -26.73784336799789330, -5.474200668421835836 ) ) ;
#9487 = CARTESIAN_POINT ( 'NONE',  ( -21.65417613035611311, -27.10241255109310998, -5.897512186717746019 ) ) ;
#9488 = CARTESIAN_POINT ( 'NONE',  ( 14.84347862571135224, 25.59847897344355161, -10.18086840633468348 ) ) ;
#9489 = CARTESIAN_POINT ( 'NONE',  ( 10.96874445820387223, 17.31868006298826046, -29.34801594517404411 ) ) ;
#9490 = ORIENTED_EDGE ( 'NONE', *, *, #29513, .T. ) ;
#9491 = DIRECTION ( 'NONE',  ( 0.000000000000000000, 0.000000000000000000, 1.000000000000000000 ) ) ;
#9492 = B_SPLINE_CURVE_WITH_KNOTS ( 'NONE', 3,
 ( #23395, #11609, #32749, #2068, #8149, #14444 ),
 .UNSPECIFIED., .F., .F.,
 ( 4, 2, 4 ),
 ( 0.000000000000000000, 0.5000000000000000000, 1.000000000000000000 ),
 .UNSPECIFIED. ) ;
#9493 = CARTESIAN_POINT ( 'NONE',  ( -12.94992061884572365, -23.08857923432204373, -15.45460198982821787 ) ) ;
#9494 = CARTESIAN_POINT ( 'NONE',  ( -35.65094714181024216, -16.36533849799707596, 15.13084544680223509 ) ) ;
#9495 = CARTESIAN_POINT ( 'NONE',  ( -24.80417270723568279, -17.12426492970035241, -15.69038464299936386 ) ) ;
#9496 = CARTESIAN_POINT ( 'NONE',  ( 1.610546824266047006, -23.23319193122145165, -14.92450978981246656 ) ) ;
#9497 = CARTESIAN_POINT ( 'NONE',  ( 15.58097433184440206, 25.94823047040191710, -6.417925113058433162 ) ) ;
#9498 = CARTESIAN_POINT ( 'NONE',  ( 21.51745293842607509, 9.710779523656842827, -13.89343078686114552 ) ) ;
#9499 = CARTESIAN_POINT ( 'NONE',  ( -18.23649648353780961, -16.09146789626143814, 20.99999999999999645 ) ) ;
#9500 = EDGE_CURVE ( 'NONE', #1586, #11592, #16270, .T. ) ;
#9501 = ORIENTED_EDGE ( 'NONE', *, *, #37681, .F. ) ;
#9502 = CARTESIAN_POINT ( 'NONE',  ( -31.67765172404683227, -3.222148243870730511, -10.44267939193049877 ) ) ;
#9503 = CARTESIAN_POINT ( 'NONE',  ( -30.17922767059062039, -0.7536324250866187624, 17.42190598798392998 ) ) ;
#9504 = EDGE_LOOP ( 'NONE', ( #12246, #23818, #22175 ) ) ;
#9505 = DIRECTION ( 'NONE',  ( 0.000000000000000000, 0.000000000000000000, 1.000000000000000000 ) ) ;
#9506 = CARTESIAN_POINT ( 'NONE',  ( 10.73859285986296541, 31.49625607628530588, 10.00000000000000000 ) ) ;
#9507 = CARTESIAN_POINT ( 'NONE',  ( -20.50889864978784161, 1.192488855597985564, -28.71852165833594484 ) ) ;
#9508 = CARTESIAN_POINT ( 'NONE',  ( 35.37860232752390743, -13.03546680616358877, -5.863704084091365232 ) ) ;
#9509 = CARTESIAN_POINT ( 'NONE',  ( 34.11403513953423783, -2.099922846023814849, 14.53008259254038848 ) ) ;
#9510 = AXIS2_PLACEMENT_3D ( 'NONE', #9439, #30971, #21818 ) ;
#9511 = VECTOR ( 'NONE', #32585, 1000.000000000000114 ) ;
#9512 = EDGE_CURVE ( 'NONE', #30503, #6957, #32319, .T. ) ;
#9513 = ORIENTED_EDGE ( 'NONE', *, *, #28950, .T. ) ;
#9514 = LINE ( 'NONE', #24945, #7681 ) ;
#9515 = EDGE_LOOP ( 'NONE', ( #25770, #8440, #23741, #22359 ) ) ;
#9516 = CARTESIAN_POINT ( 'NONE',  ( -14.47283171447380035, 21.48159823030330884, 9.000000000000001776 ) ) ;
#9517 = DIRECTION ( 'NONE',  ( 0.000000000000000000, 0.000000000000000000, -1.000000000000000000 ) ) ;
#9518 = EDGE_CURVE ( 'NONE', #3967, #18163, #8540, .T. ) ;
#9519 = DIRECTION ( 'NONE',  ( 0.9510565162951543083, 0.3090169943749450088, 0.000000000000000000 ) ) ;
#9520 = ORIENTED_EDGE ( 'NONE', *, *, #16972, .F. ) ;
#9521 = ADVANCED_FACE ( 'NONE', ( #39402 ), #35767, .T. ) ;
#9522 = CARTESIAN_POINT ( 'NONE',  ( -3.585224264196515520, 32.04905365121025795, -13.82507829668538868 ) ) ;
#9523 = CARTESIAN_POINT ( 'NONE',  ( 3.295881626406581777, 9.398963235502485247, 9.500000000000000000 ) ) ;
#9524 = DIRECTION ( 'NONE',  ( -0.9135454576426059736, -0.4067366430757888285, -0.000000000000000000 ) ) ;
#9525 = EDGE_CURVE ( 'NONE', #16948, #11613, #26250, .T. ) ;
#9526 = DIRECTION ( 'NONE',  ( -1.000000000000000000, 0.000000000000000000, 0.000000000000000000 ) ) ;
#9527 = CARTESIAN_POINT ( 'NONE',  ( 13.63581098909226874, 27.45627467658428955, 7.000000000000000000 ) ) ;
#9528 = DIRECTION ( 'NONE',  ( 0.000000000000000000, 0.000000000000000000, 1.000000000000000000 ) ) ;
#9529 = CARTESIAN_POINT ( 'NONE',  ( 12.27639651543910837, 27.18797350401429824, -13.23837527007015602 ) ) ;
#9530 = ORIENTED_EDGE ( 'NONE', *, *, #20537, .F. ) ;
#9531 = CARTESIAN_POINT ( 'NONE',  ( -21.25484840722362279, 12.72181903587277318, -5.000000000000000000 ) ) ;
#9532 = CARTESIAN_POINT ( 'NONE',  ( -34.47241746879593904, 3.460351812918829761, 0.000000000000000000 ) ) ;
#9533 = CARTESIAN_POINT ( 'NONE',  ( 10.08869499956528415, -18.76399072035841442, -25.00021918992353775 ) ) ;
#9534 = LINE ( 'NONE', #15227, #15874 ) ;
#9535 = CARTESIAN_POINT ( 'NONE',  ( 11.25614974650753375, 18.08000221745906089, -25.00715939995231096 ) ) ;
#9536 = CARTESIAN_POINT ( 'NONE',  ( 21.88499642459564143, -5.528038495964486820, -20.11584339644707597 ) ) ;
#9537 = CYLINDRICAL_SURFACE ( 'NONE', #27829, 1.000000000000000888 ) ;
#9538 = AXIS2_PLACEMENT_3D ( 'NONE', #37478, #40117, #24683 ) ;
#9539 = CARTESIAN_POINT ( 'NONE',  ( -10.96701088540842761, 17.31978028264472513, -29.99999999999999645 ) ) ;
#9540 = CARTESIAN_POINT ( 'NONE',  ( -14.45284558077854520, -15.31887616786443296, -26.42903543862076177 ) ) ;
#9541 = CARTESIAN_POINT ( 'NONE',  ( 9.204648767762177997, -22.95956739582980077, -15.68808466976011040 ) ) ;
#9542 = CARTESIAN_POINT ( 'NONE',  ( 14.98023422679249528, 25.65947670479530984, -9.711130374113162489 ) ) ;
#9543 = CARTESIAN_POINT ( 'NONE',  ( 30.66924623482115209, -20.77338707453388977, -8.848560859720739913 ) ) ;
#9544 = ADVANCED_FACE ( 'NONE', ( #8336 ), #23164, .F. ) ;
#9545 = LINE ( 'NONE', #6281, #7934 ) ;
#9546 = ADVANCED_FACE ( 'NONE', ( #2045 ), #13250, .T. ) ;
#9547 = EDGE_LOOP ( 'NONE', ( #17102, #26780, #22670 ) ) ;
#9548 = CARTESIAN_POINT ( 'NONE',  ( -10.07745175218284217, 33.85409929753423341, -8.493742715255910625 ) ) ;
#9549 = FACE_OUTER_BOUND ( 'NONE', #19529, .T. ) ;
#9550 = CARTESIAN_POINT ( 'NONE',  ( 9.997483185316555776, 21.95197631500757041, 10.50000000000000355 ) ) ;
#9551 = CARTESIAN_POINT ( 'NONE',  ( -5.082607396026893376, 23.58034083595207875, 13.00000000000000178 ) ) ;
#9552 = ORIENTED_EDGE ( 'NONE', *, *, #31848, .T. ) ;
#9553 = CARTESIAN_POINT ( 'NONE',  ( 29.32892909551985028, 0.1034583756683473688, -10.65428865362305721 ) ) ;
#9554 = LINE ( 'NONE', #12985, #38160 ) ;
#9555 = DIRECTION ( 'NONE',  ( 1.000000000000000000, 0.000000000000000000, 0.000000000000000000 ) ) ;
#9556 = EDGE_LOOP ( 'NONE', ( #21139, #6770, #30253, #34296 ) ) ;
#9557 = CARTESIAN_POINT ( 'NONE',  ( -20.96646152425979537, 0.8383472484117416856, -26.22754307947055707 ) ) ;
#9558 = CARTESIAN_POINT ( 'NONE',  ( 2.421689871081641687, 8.701977744317826335, 7.499999999999991118 ) ) ;
#9559 = ORIENTED_EDGE ( 'NONE', *, *, #16715, .T. ) ;
#9560 = CARTESIAN_POINT ( 'NONE',  ( 20.71247045076932736, -3.585883499709318745, -26.50471444526433373 ) ) ;
#9561 = ORIENTED_EDGE ( 'NONE', *, *, #8273, .T. ) ;
#9562 = CARTESIAN_POINT ( 'NONE',  ( 16.76301160834832871, 29.17407194212043464, 12.14047268033043103 ) ) ;
#9563 = DIRECTION ( 'NONE',  ( -0.9781476007338069101, -0.2079116908177532919, 0.000000000000000000 ) ) ;
#9564 = CARTESIAN_POINT ( 'NONE',  ( -11.54666566735211752, 32.07468077621347646, 7.500000000000004441 ) ) ;
#9565 = EDGE_CURVE ( 'NONE', #12651, #13548, #38583, .T. ) ;
#9566 = CARTESIAN_POINT ( 'NONE',  ( -10.24445352883136984, 27.94073041968543691, 19.66345542862531204 ) ) ;
#9567 = AXIS2_PLACEMENT_3D ( 'NONE', #8087, #20496, #20699 ) ;
#9568 = CARTESIAN_POINT ( 'NONE',  ( 9.183240348400453001, 28.21559575157615996, 6.000000000000000000 ) ) ;
#9569 = VERTEX_POINT ( 'NONE', #2244 ) ;
#9570 = DIRECTION ( 'NONE',  ( 0.000000000000000000, 0.000000000000000000, 1.000000000000000000 ) ) ;
#9571 = CARTESIAN_POINT ( 'NONE',  ( -16.74436491739946575, 11.83083178865852148, -30.00000000000000000 ) ) ;
#9572 = CARTESIAN_POINT ( 'NONE',  ( 0.5000000000000001110, 37.00000000000000711, 9.000000000000001776 ) ) ;
#9573 = CIRCLE ( 'NONE', #36200, 1.000000000000000000 ) ;
#9574 = FACE_OUTER_BOUND ( 'NONE', #26180, .T. ) ;
#9575 = CARTESIAN_POINT ( 'NONE',  ( 18.10616661872212418, 18.94352981041244277, -6.438559219923253529 ) ) ;
#9576 = AXIS2_PLACEMENT_3D ( 'NONE', #4367, #7614, #29157 ) ;
#9577 = CARTESIAN_POINT ( 'NONE',  ( 8.932770706806998362, 34.72274584801672859, -8.469836187294838226 ) ) ;
#9578 = CARTESIAN_POINT ( 'NONE',  ( 11.86460666947250964, -19.15457323191094119, -22.56163012647707333 ) ) ;
#9579 = CYLINDRICAL_SURFACE ( 'NONE', #32711, 1.000000000000000000 ) ;
#9580 = DIRECTION ( 'NONE',  ( -0.9945218953682742891, -0.1045284632676437425, 0.000000000000000000 ) ) ;
#9581 = VERTEX_POINT ( 'NONE', #8531 ) ;
#9582 = CARTESIAN_POINT ( 'NONE',  ( -15.24722010801124839, 26.35548338364083421, -7.828046445912475448 ) ) ;
#9583 = CARTESIAN_POINT ( 'NONE',  ( -34.90004137879623158, -9.293601764824154898, 16.87380292611441490 ) ) ;
#9584 = CARTESIAN_POINT ( 'NONE',  ( 13.59058049318332806, -24.10307348923517523, -13.51868193062158063 ) ) ;
#9585 = CYLINDRICAL_SURFACE ( 'NONE', #3639, 1.000000000000000000 ) ;
#9586 = ADVANCED_FACE ( 'NONE', ( #14631 ), #8122, .F. ) ;
#9587 = ORIENTED_EDGE ( 'NONE', *, *, #9882, .F. ) ;
#9588 = VERTEX_POINT ( 'NONE', #1847 ) ;
#9589 = CARTESIAN_POINT ( 'NONE',  ( -10.02826340246190640, 19.59635890697872895, -23.63231146289030704 ) ) ;
#9590 = CARTESIAN_POINT ( 'NONE',  ( -13.55038157627658002, -20.63826655719205760, -19.25262925335620778 ) ) ;
#9591 = FACE_BOUND ( 'NONE', #35840, .T. ) ;
#9592 = AXIS2_PLACEMENT_3D ( 'NONE', #37380, #24782, #15042 ) ;
#9593 = CIRCLE ( 'NONE', #18045, 0.5000000000000004441 ) ;
#9594 = ORIENTED_EDGE ( 'NONE', *, *, #10139, .T. ) ;
#9595 = CARTESIAN_POINT ( 'NONE',  ( -19.64501015271085294, -6.129868598536533320, -28.49191429157074396 ) ) ;
#9596 = CARTESIAN_POINT ( 'NONE',  ( -9.413550212251061922, -18.21086026825004112, -30.00000000000000000 ) ) ;
#9597 = CARTESIAN_POINT ( 'NONE',  ( 5.644276917315719899, 36.40655018617690786, 11.00000000000000000 ) ) ;
#9598 = EDGE_LOOP ( 'NONE', ( #29349, #20623, #12877, #10726 ) ) ;
#9599 = CARTESIAN_POINT ( 'NONE',  ( 20.59811166339096644, 1.045058112078671941, -28.08708561988663988 ) ) ;
#9600 = DIRECTION ( 'NONE',  ( 0.000000000000000000, 0.000000000000000000, 1.000000000000000000 ) ) ;
#9601 = CARTESIAN_POINT ( 'NONE',  ( -12.05736835487443415, 14.38397459621567442, 11.00000000000000000 ) ) ;
#9602 = AXIS2_PLACEMENT_3D ( 'NONE', #35948, #8315, #8713 ) ;
#9603 = EDGE_LOOP ( 'NONE', ( #1246, #6791, #17794, #38599, #24819, #21333 ) ) ;
#9604 = CARTESIAN_POINT ( 'NONE',  ( -24.57004144261168932, 0.4099649594921800921, -18.44930745607893741 ) ) ;
#9605 = VERTEX_POINT ( 'NONE', #33332 ) ;
#9606 = CARTESIAN_POINT ( 'NONE',  ( 31.98272768806592481, -1.800652305183228830, -7.760027792917767009 ) ) ;
#9607 = CIRCLE ( 'NONE', #40073, 1.000000000000000000 ) ;
#9608 = CARTESIAN_POINT ( 'NONE',  ( 16.15629783291639399, -12.69278426743109200, -30.00000000000003908 ) ) ;
#9609 = CARTESIAN_POINT ( 'NONE',  ( 20.61005271883062306, -26.74738414229423000, 16.87380292611441845 ) ) ;
#9610 = EDGE_LOOP ( 'NONE', ( #18549, #35645, #34311, #33005, #23421, #29085 ) ) ;
#9611 = CARTESIAN_POINT ( 'NONE',  ( -24.83189327688484838, 4.353783615239871452, -13.73059695307320105 ) ) ;
#9612 = DIRECTION ( 'NONE',  ( -0.000000000000000000, -0.000000000000000000, -1.000000000000000000 ) ) ;
#9613 = ADVANCED_FACE ( 'NONE', ( #1434, #7724 ), #17085, .T. ) ;
#9614 = DIRECTION ( 'NONE',  ( 1.000000000000000000, 0.000000000000000000, 0.000000000000000000 ) ) ;
#9615 = FACE_OUTER_BOUND ( 'NONE', #4614, .T. ) ;
#9616 = EDGE_CURVE ( 'NONE', #5670, #38335, #1616, .T. ) ;
#9617 = EDGE_CURVE ( 'NONE', #20501, #38258, #35339, .T. ) ;
#9618 = FACE_OUTER_BOUND ( 'NONE', #20340, .T. ) ;
#9619 = CIRCLE ( 'NONE', #20658, 1.000000000000002665 ) ;
#9620 = AXIS2_PLACEMENT_3D ( 'NONE', #37230, #31326, #6335 ) ;
#9621 = EDGE_CURVE ( 'NONE', #40046, #15493, #29459, .T. ) ;
#9622 = FACE_BOUND ( 'NONE', #1815, .T. ) ;
#9623 = CARTESIAN_POINT ( 'NONE',  ( 20.66414367076000858, 17.76245163070478839, 11.55979286843843390 ) ) ;
#9624 = CARTESIAN_POINT ( 'NONE',  ( -21.79696480337856812, 7.571043879021812195, -16.91776734276888305 ) ) ;
#9625 = CARTESIAN_POINT ( 'NONE',  ( 7.111215932167701759, 17.81698729810774751, 7.000000000000000000 ) ) ;
#9626 = CARTESIAN_POINT ( 'NONE',  ( 7.611215932167711529, 18.68301270189218855, 9.000000000000001776 ) ) ;
#9627 = CARTESIAN_POINT ( 'NONE',  ( 23.17353744146408800, -25.53105782170328553, -9.399317870189824120 ) ) ;
#9628 = LINE ( 'NONE', #9223, #870 ) ;
#9629 = CARTESIAN_POINT ( 'NONE',  ( 15.32268921037612586, 27.10638078547256669, -5.472625680277237947 ) ) ;
#9630 = AXIS2_PLACEMENT_3D ( 'NONE', #21930, #6092, #15441 ) ;
#9631 = ORIENTED_EDGE ( 'NONE', *, *, #21441, .F. ) ;
#9632 = CARTESIAN_POINT ( 'NONE',  ( -14.50975249381452592, 20.88454814334572163, -15.58843137732770856 ) ) ;
#9633 = CARTESIAN_POINT ( 'NONE',  ( -28.41077021456755958, -6.925791943820290619, 20.25080042701566541 ) ) ;
#9634 = DIRECTION ( 'NONE',  ( 0.000000000000000000, 0.000000000000000000, -1.000000000000000000 ) ) ;
#9635 = CARTESIAN_POINT ( 'NONE',  ( 15.43643446434663069, 26.70998168114506299, -4.999999999999998224 ) ) ;
#9636 = ORIENTED_EDGE ( 'NONE', *, *, #14389, .T. ) ;
#9637 = CARTESIAN_POINT ( 'NONE',  ( -3.357189294653177836, 32.49896394832315849, 11.00000000000000000 ) ) ;
#9638 = EDGE_CURVE ( 'NONE', #2968, #14160, #22553, .T. ) ;
#9639 = VERTEX_POINT ( 'NONE', #33129 ) ;
#9641 = DIRECTION ( 'NONE',  ( -0.1045284632676569680, -0.9945218953682730678, 0.000000000000000000 ) ) ;
#9640 = CARTESIAN_POINT ( 'NONE',  ( -13.93471959586060649, 24.16489319529103241, -13.49162670121266139 ) ) ;
#9642 = EDGE_CURVE ( 'NONE', #2072, #13470, #28193, .T. ) ;
#9643 = CARTESIAN_POINT ( 'NONE',  ( -15.07802003622312270, -25.87832397125552220, -9.698090967223700787 ) ) ;
#9644 = CARTESIAN_POINT ( 'NONE',  ( 12.29179778625991304, 14.31343464431668799, 10.49999999999999822 ) ) ;
#9645 = EDGE_CURVE ( 'NONE', #21571, #3398, #18677, .T. ) ;
#9646 = ORIENTED_EDGE ( 'NONE', *, *, #28865, .F. ) ;
#9647 = CARTESIAN_POINT ( 'NONE',  ( -27.13442240602560318, -13.17128934651453598, -15.68741833354276416 ) ) ;
#9648 = CARTESIAN_POINT ( 'NONE',  ( -8.888899028085873510, -18.51857346408734273, -28.73058333705254341 ) ) ;
#9649 = DIRECTION ( 'NONE',  ( 0.000000000000000000, 1.000000000000000000, 0.000000000000000000 ) ) ;
#9650 = CARTESIAN_POINT ( 'NONE',  ( 12.46547198588941896, 16.48917403503523005, -27.54678004591448470 ) ) ;
#9651 = ORIENTED_EDGE ( 'NONE', *, *, #1227, .F. ) ;
#9652 = CARTESIAN_POINT ( 'NONE',  ( 25.76556103975890721, 5.561561074672148663, -7.879988086958064741 ) ) ;
#9653 = CARTESIAN_POINT ( 'NONE',  ( -0.5000000000000004441, 37.00000000000000711, 9.000000000000001776 ) ) ;
#9654 = CARTESIAN_POINT ( 'NONE',  ( 0.000000000000000000, 22.50000000000000355, 13.00000000000000178 ) ) ;
#9655 = CARTESIAN_POINT ( 'NONE',  ( -14.02522273992627078, -18.92975101292878293, -21.21400966844822378 ) ) ;
#9656 = B_SPLINE_CURVE_WITH_KNOTS ( 'NONE', 3,
 ( #25325, #12734, #15590, #6041, #3392, #6828 ),
 .UNSPECIFIED., .F., .F.,
 ( 4, 2, 4 ),
 ( 0.000000000000000000, 0.5000000000000000000, 1.000000000000000000 ),
 .UNSPECIFIED. ) ;
#9657 = ORIENTED_EDGE ( 'NONE', *, *, #27246, .T. ) ;
#9658 = CARTESIAN_POINT ( 'NONE',  ( -24.88924877381098355, -0.2642620682496472084, -18.35903378176135803 ) ) ;
#9660 = CARTESIAN_POINT ( 'NONE',  ( 29.57816538328471268, -0.1796088123746400478, -10.63313785040832293 ) ) ;
#9659 = AXIS2_PLACEMENT_3D ( 'NONE', #12970, #16026, #31666 ) ;
#9661 = AXIS2_PLACEMENT_3D ( 'NONE', #22501, #34911, #35513 ) ;
#9662 = CARTESIAN_POINT ( 'NONE',  ( 27.85940672053917311, -14.94704994757669780, 20.50957957746029336 ) ) ;
#9663 = EDGE_LOOP ( 'NONE', ( #38524, #7589 ) ) ;
#9664 = VECTOR ( 'NONE', #14258, 1000.000000000000000 ) ;
#9665 = CARTESIAN_POINT ( 'NONE',  ( 26.31271763591406909, -28.25584584496056451, -14.26382729546506667 ) ) ;
#9666 = ADVANCED_FACE ( 'NONE', ( #15424 ), #23653, .T. ) ;
#9667 = DIRECTION ( 'NONE',  ( 1.000000000000000000, 0.000000000000000000, 0.000000000000000000 ) ) ;
#9668 = ADVANCED_FACE ( 'NONE', ( #31069 ), #15024, .F. ) ;
#9669 = ORIENTED_EDGE ( 'NONE', *, *, #24746, .F. ) ;
#9670 = FACE_OUTER_BOUND ( 'NONE', #8000, .T. ) ;
#9671 = DIRECTION ( 'NONE',  ( -1.000000000000000000, 0.000000000000000000, 0.000000000000000000 ) ) ;
#9672 = DIRECTION ( 'NONE',  ( 0.000000000000000000, 0.000000000000000000, 1.000000000000000000 ) ) ;
#9673 = CARTESIAN_POINT ( 'NONE',  ( 2.406064665179193263, 33.30697029628942119, -12.89611003825230107 ) ) ;
#9674 = CARTESIAN_POINT ( 'NONE',  ( 14.91650131011209268, 21.43496667674292055, 10.76099332938163577 ) ) ;
#9675 = CARTESIAN_POINT ( 'NONE',  ( 14.86556419889023672, 20.43481210330075726, 10.59344459855564935 ) ) ;
#9676 = CARTESIAN_POINT ( 'NONE',  ( 8.183240348400453001, 28.21559575157615996, 6.000000000000000000 ) ) ;
#9677 = DIRECTION ( 'NONE',  ( -0.000000000000000000, -0.000000000000000000, -1.000000000000000000 ) ) ;
#9678 = CARTESIAN_POINT ( 'NONE',  ( -7.929471891321301591, 25.60217271033470610, 9.000000000000001776 ) ) ;
#9679 = CARTESIAN_POINT ( 'NONE',  ( -5.953812613386785912, 14.77701242934787906, 6.000000000000000000 ) ) ;
#9680 = VECTOR ( 'NONE', #14470, 1000.000000000000000 ) ;
#9681 = CARTESIAN_POINT ( 'NONE',  ( 10.27379371539876907, 17.74076016529687649, -30.00000000000000000 ) ) ;
#9682 = CARTESIAN_POINT ( 'NONE',  ( -35.48538791413474769, -11.24999995268676933, -5.000000000000001776 ) ) ;
#9683 = AXIS2_PLACEMENT_3D ( 'NONE', #11336, #7872, #21077 ) ;
#9684 = EDGE_LOOP ( 'NONE', ( #1207, #28331 ) ) ;
#9686 = CARTESIAN_POINT ( 'NONE',  ( 5.362728154695970417, 13.41753630677055753, 10.50000000000000000 ) ) ;
#9685 = CARTESIAN_POINT ( 'NONE',  ( -15.46485185209717628, 13.55220689985132410, -28.26754509741839527 ) ) ;
#9687 = CARTESIAN_POINT ( 'NONE',  ( 33.69589222704784248, -0.03122585499641188089, 11.00000000000003908 ) ) ;
#9688 = CARTESIAN_POINT ( 'NONE',  ( 9.552972388026635286, -18.28221569941723601, -28.07838513181713225 ) ) ;
#9689 = CARTESIAN_POINT ( 'NONE',  ( -14.02522273755474380, -18.92975100993347581, -21.21400967388834857 ) ) ;
#9690 = CARTESIAN_POINT ( 'NONE',  ( 11.04317535683834883, 17.42292179296065413, -28.07760017567576583 ) ) ;
#9691 = CARTESIAN_POINT ( 'NONE',  ( 15.40885724145108249, 26.80895719503613606, -5.474085382006591338 ) ) ;
#9692 = VECTOR ( 'NONE', #30053, 1000.000000000000114 ) ;
#9693 = B_SPLINE_SURFACE_WITH_KNOTS ( 'NONE', 1, 3, ( 
 ( #20629, #17184, #23267, #23666, #35661, #7819, #20828, #32823, #20222, #23865 ),
 ( #29559, #1738, #14520, #26913, #4978, #17390, #29764, #5375, #36268, #8431 ) ),
 .UNSPECIFIED., .F., .F., .F.,
 ( 2, 2 ),
 ( 4, 2, 2, 2, 4 ),
 ( 0.000000000000000000, 1.000000000000000000 ),
 ( -1.496612791730154157, -1.103913710031430906, -0.7112146283327074325, -0.3185155466339841257, 0.07418353506473918113 ),
 .UNSPECIFIED. ) ;
#9694 = EDGE_LOOP ( 'NONE', ( #25430, #23181, #15380, #11571 ) ) ;
#9695 = CARTESIAN_POINT ( 'NONE',  ( -8.118377661053489902, 10.47536095541709322, 9.000000000000001776 ) ) ;
#9696 = CARTESIAN_POINT ( 'NONE',  ( -11.48389827485794434, -20.98450916179802306, -19.50346772467152334 ) ) ;
#9697 = CARTESIAN_POINT ( 'NONE',  ( -33.82738586796177316, -21.73727074213755728, 13.32518128616597153 ) ) ;
#9698 = CARTESIAN_POINT ( 'NONE',  ( -22.40361533374172964, -16.48201631266229228, -17.62577809116323380 ) ) ;
#9699 = CARTESIAN_POINT ( 'NONE',  ( -1.770315541423665318, -20.49735477589887367, -28.86146915265202750 ) ) ;
#9700 = CARTESIAN_POINT ( 'NONE',  ( 14.44003496283569810, 22.99600343737122898, -13.55926162218559128 ) ) ;
#9701 = VERTEX_POINT ( 'NONE', #28011 ) ;
#9702 = CARTESIAN_POINT ( 'NONE',  ( 19.27723472360040091, 8.927243194702443319, -23.31752901678017054 ) ) ;
#9703 = CARTESIAN_POINT ( 'NONE',  ( 2.476901250629512941, 26.36149378532653031, 6.000000000000000000 ) ) ;
#9704 = VERTEX_POINT ( 'NONE', #18480 ) ;
#9705 = CARTESIAN_POINT ( 'NONE',  ( -28.41830146766454845, -3.622177512335159388, -15.08422308592607131 ) ) ;
#9706 = CARTESIAN_POINT ( 'NONE',  ( -26.89145897433321863, 3.386615419929385418, 16.87380292612052202 ) ) ;
#9707 = EDGE_LOOP ( 'NONE', ( #26526, #30380, #26386, #17885 ) ) ;
#9708 = LINE ( 'NONE', #22088, #33663 ) ;
#9709 = CARTESIAN_POINT ( 'NONE',  ( 3.399837471815457590, 8.909889435135580626, 7.499999999999990230 ) ) ;
#9710 = B_SPLINE_CURVE_WITH_KNOTS ( 'NONE', 3,
 ( #4259, #35950, #32910, #19700, #10561, #32092 ),
 .UNSPECIFIED., .F., .F.,
 ( 4, 2, 4 ),
 ( 0.000000000000000000, 0.5000000000000001110, 1.000000000000000000 ),
 .UNSPECIFIED. ) ;
#9711 = CARTESIAN_POINT ( 'NONE',  ( -27.84741259050295170, 0.7654686433649292576, -12.57911469547112304 ) ) ;
#9712 = CARTESIAN_POINT ( 'NONE',  ( 19.43389763942624882, -6.523976669268585660, -29.99999999999999645 ) ) ;
#9713 = CARTESIAN_POINT ( 'NONE',  ( 33.65490896085587735, -21.61118400457290534, 13.92931973827805336 ) ) ;
#9714 = EDGE_LOOP ( 'NONE', ( #24557, #30762, #16743, #6004 ) ) ;
#9715 = DIRECTION ( 'NONE',  ( 0.6691306063588569053, -0.7431448254773954654, 0.000000000000000000 ) ) ;
#9716 = ORIENTED_EDGE ( 'NONE', *, *, #26517, .T. ) ;
#9717 = DIRECTION ( 'NONE',  ( 1.000000000000000000, 0.000000000000000000, 0.000000000000000000 ) ) ;
#9718 = CARTESIAN_POINT ( 'NONE',  ( 6.462764152049920163, 17.91932574229958419, 23.00000000000000000 ) ) ;
#9719 = DIRECTION ( 'NONE',  ( 0.4999999999999912292, -0.8660254037844437036, 0.000000000000000000 ) ) ;
#9720 = VERTEX_POINT ( 'NONE', #15625 ) ;
#9721 = CARTESIAN_POINT ( 'NONE',  ( -3.003906060479351936, 37.17650976190002865, -8.411038520408236963 ) ) ;
#9722 = CARTESIAN_POINT ( 'NONE',  ( -12.77091082532341382, 29.60251629318183575, 13.00000000000000178 ) ) ;
#9723 = LINE ( 'NONE', #22104, #37095 ) ;
#9724 = LINE ( 'NONE', #6653, #28611 ) ;
#9725 = CARTESIAN_POINT ( 'NONE',  ( -12.39464589777671044, 26.66807349098043289, 6.000000000000000000 ) ) ;
#9726 = CARTESIAN_POINT ( 'NONE',  ( -10.44103466624267540, 32.57396620494226624, 11.00000000000000000 ) ) ;
#9727 = CARTESIAN_POINT ( 'NONE',  ( 8.118011562862880837, 18.90506291166681052, -28.59249439703800988 ) ) ;
#9728 = ORIENTED_EDGE ( 'NONE', *, *, #38799, .T. ) ;
#9729 = CARTESIAN_POINT ( 'NONE',  ( -19.25317702551486576, 10.46635355190964844, -20.12010506014689426 ) ) ;
#9730 = CARTESIAN_POINT ( 'NONE',  ( 10.37659644360210542, 39.73422260060681310, 11.00000000000000000 ) ) ;
#9731 = CARTESIAN_POINT ( 'NONE',  ( 10.27113998026189989, -19.14829838377831805, -23.84809487166246811 ) ) ;
#9732 = DIRECTION ( 'NONE',  ( 0.8090169943749504489, 0.5877852522924690293, 0.000000000000000000 ) ) ;
#9733 = CARTESIAN_POINT ( 'NONE',  ( 13.45276934512811806, 22.89459220598109113, -15.44166492943546309 ) ) ;
#9734 = CARTESIAN_POINT ( 'NONE',  ( 26.31271763591405133, -28.25584584496056806, -4.999999999999990230 ) ) ;
#9735 = CARTESIAN_POINT ( 'NONE',  ( -8.312041872459065672, 25.58773265502866678, 12.00000000000000000 ) ) ;
#9736 = CARTESIAN_POINT ( 'NONE',  ( -27.01125781910978318, -25.31691801271181674, -5.870809593036823593 ) ) ;
#9737 = CARTESIAN_POINT ( 'NONE',  ( 8.856982299079746213, -19.61396123686068549, -24.00676120555290183 ) ) ;
#9738 = CARTESIAN_POINT ( 'NONE',  ( 15.47833181635298772, 26.56067009156167558, -4.999999999999998224 ) ) ;
#9739 = CARTESIAN_POINT ( 'NONE',  ( 19.66024882222950509, -13.28965305365858818, -21.85380848813069576 ) ) ;
#9740 = EDGE_CURVE ( 'NONE', #13272, #39672, #184, .T. ) ;
#9741 = CARTESIAN_POINT ( 'NONE',  ( 13.81505241748941515, 27.51451374705149888, 10.96580508970281542 ) ) ;
#9742 = CARTESIAN_POINT ( 'NONE',  ( -14.70623423376111738, 19.54590544129804286, 7.000000000000000000 ) ) ;
#9743 = EDGE_LOOP ( 'NONE', ( #14601, #38030, #16125 ) ) ;
#9744 = AXIS2_PLACEMENT_3D ( 'NONE', #22047, #6403, #9671 ) ;
#9745 = CARTESIAN_POINT ( 'NONE',  ( -7.666838832020851591, 32.44533431280383695, -12.05124513101535655 ) ) ;
#9746 = CARTESIAN_POINT ( 'NONE',  ( 10.03245514394483706, 31.53326318584457510, 7.000000000000000000 ) ) ;
#9747 = DIRECTION ( 'NONE',  ( 0.000000000000000000, 0.000000000000000000, 1.000000000000000000 ) ) ;
#9748 = VERTEX_POINT ( 'NONE', #27817 ) ;
#9749 = CARTESIAN_POINT ( 'NONE',  ( 30.71313057055191820, -0.01776306241125666374, -6.887927186766908072 ) ) ;
#9750 = ADVANCED_FACE ( 'NONE', ( #17891 ), #30871, .F. ) ;
#9751 = CARTESIAN_POINT ( 'NONE',  ( 14.53551886312849994, 26.20443074943802841, 7.338691926023212631 ) ) ;
#9752 = CARTESIAN_POINT ( 'NONE',  ( -16.00000000000000000, 22.50000000000000711, 12.00000000000000000 ) ) ;
#9753 = EDGE_CURVE ( 'NONE', #39323, #14045, #16515, .T. ) ;
#9754 = EDGE_LOOP ( 'NONE', ( #1603, #1414, #16253, #35134 ) ) ;
#9755 = CARTESIAN_POINT ( 'NONE',  ( -20.69195238456651964, 0.8693669606531726490, -27.44980246086476683 ) ) ;
#9756 = CARTESIAN_POINT ( 'NONE',  ( -2.118678732975735279, 7.827785988993307242, 12.00000000000000000 ) ) ;
#9757 = VERTEX_POINT ( 'NONE', #2636 ) ;
#9758 = CARTESIAN_POINT ( 'NONE',  ( 35.04727437832835335, -7.360793022001182351, -5.447201208417698837 ) ) ;
#9759 = VECTOR ( 'NONE', #11165, 1000.000000000000000 ) ;
#9760 = ORIENTED_EDGE ( 'NONE', *, *, #12309, .T. ) ;
#9761 = CARTESIAN_POINT ( 'NONE',  ( -14.73160032165950284, 32.49283138996943165, 12.73282698324853079 ) ) ;
#9762 = DIRECTION ( 'NONE',  ( 0.000000000000000000, 0.000000000000000000, 1.000000000000000000 ) ) ;
#9763 = CARTESIAN_POINT ( 'NONE',  ( 12.30736835487432757, 14.81698729810772441, 9.500000000000000000 ) ) ;
#9764 = CARTESIAN_POINT ( 'NONE',  ( 3.920592112299155829, 34.13862021880822084, 19.27171037444156809 ) ) ;
#9765 = CYLINDRICAL_SURFACE ( 'NONE', #24614, 0.5000000000000004441 ) ;
#9766 = ORIENTED_EDGE ( 'NONE', *, *, #15111, .F. ) ;
#9767 = CARTESIAN_POINT ( 'NONE',  ( 3.900351417861458003, 8.105760029628141794, 10.49999999999999822 ) ) ;
#9768 = CARTESIAN_POINT ( 'NONE',  ( -19.95996515113903769, 4.687952722032478370, -30.00000000000001066 ) ) ;
#9769 = EDGE_CURVE ( 'NONE', #7636, #37730, #9534, .T. ) ;
#9770 = DIRECTION ( 'NONE',  ( 1.000000000000000000, 0.000000000000000000, 0.000000000000000000 ) ) ;
#9771 = EDGE_CURVE ( 'NONE', #8098, #34344, #15212, .T. ) ;
#9772 = AXIS2_PLACEMENT_3D ( 'NONE', #2179, #14563, #26955 ) ;
#9773 = CYLINDRICAL_SURFACE ( 'NONE', #39633, 1.000000000000000000 ) ;
#9774 = CARTESIAN_POINT ( 'NONE',  ( 17.90821008046413354, 18.66479283707571213, -8.856698538950956490 ) ) ;
#9775 = CARTESIAN_POINT ( 'NONE',  ( 6.745778725514791851, 29.76450411120941908, -14.82904111780637280 ) ) ;
#9776 = CARTESIAN_POINT ( 'NONE',  ( 17.60569237627828443, -25.83491465451036362, -10.48832399961285411 ) ) ;
#9777 = FACE_OUTER_BOUND ( 'NONE', #35539, .T. ) ;
#9778 = LINE ( 'NONE', #37613, #512 ) ;
#9779 = ORIENTED_EDGE ( 'NONE', *, *, #23736, .T. ) ;
#9780 = CARTESIAN_POINT ( 'NONE',  ( -12.14918073411995003, 19.90232399862620127, -20.54428201483505134 ) ) ;
#9781 = CIRCLE ( 'NONE', #37680, 1.000000000000000000 ) ;
#9782 = CARTESIAN_POINT ( 'NONE',  ( -33.72852460920479700, -9.442290196615397591, 17.92354375535250810 ) ) ;
#9783 = CARTESIAN_POINT ( 'NONE',  ( 15.03134232453200347, -26.43346543218465783, -7.358877968120621560 ) ) ;
#9784 = AXIS2_PLACEMENT_3D ( 'NONE', #10261, #29154, #22642 ) ;
#9785 = LINE ( 'NONE', #28463, #36074 ) ;
#9786 = ORIENTED_EDGE ( 'NONE', *, *, #34397, .F. ) ;
#9787 = ORIENTED_EDGE ( 'NONE', *, *, #13414, .T. ) ;
#9788 = CARTESIAN_POINT ( 'NONE',  ( -14.39563127090040062, 29.49628440365493276, -5.920050663511798206 ) ) ;
#9789 = FACE_OUTER_BOUND ( 'NONE', #14905, .T. ) ;
#9790 = EDGE_CURVE ( 'NONE', #8575, #24087, #37160, .T. ) ;
#9791 = FACE_BOUND ( 'NONE', #16095, .T. ) ;
#9792 = CARTESIAN_POINT ( 'NONE',  ( -31.91225982942368233, -8.858501497912342870, -12.06783560505458297 ) ) ;
#9793 = CARTESIAN_POINT ( 'NONE',  ( -15.20174574604959616, -26.47514097219373141, -7.358271501857936769 ) ) ;
#9794 = FACE_OUTER_BOUND ( 'NONE', #33540, .T. ) ;
#9795 = ORIENTED_EDGE ( 'NONE', *, *, #35085, .T. ) ;
#9796 = CARTESIAN_POINT ( 'NONE',  ( 29.76485216031830205, 0.2778845579280027622, -9.242486094669974506 ) ) ;
#9797 = DIRECTION ( 'NONE',  ( 0.000000000000000000, 0.000000000000000000, 1.000000000000000000 ) ) ;
#9798 = DIRECTION ( 'NONE',  ( 1.000000000000000000, 0.000000000000000000, 0.000000000000000000 ) ) ;
#9799 = AXIS2_PLACEMENT_3D ( 'NONE', #1230, #10170, #29654 ) ;
#9800 = ORIENTED_EDGE ( 'NONE', *, *, #22586, .F. ) ;
#9801 = CARTESIAN_POINT ( 'NONE',  ( -21.71446517679514088, 0.7002016955605907533, -23.85068631983916987 ) ) ;
#9802 = ORIENTED_EDGE ( 'NONE', *, *, #6314, .F. ) ;
#9803 = CARTESIAN_POINT ( 'NONE',  ( 29.30903811477968546, -1.149447832272777248, -12.42997963733888334 ) ) ;
#9804 = CARTESIAN_POINT ( 'NONE',  ( 10.78893975237932956, 23.27376113029817617, 6.000000000000000000 ) ) ;
#9805 = CARTESIAN_POINT ( 'NONE',  ( 17.16434664249021225, -27.18154623538450565, 16.30093088680120417 ) ) ;
#9806 = ORIENTED_EDGE ( 'NONE', *, *, #11747, .F. ) ;
#9807 = B_SPLINE_CURVE_WITH_KNOTS ( 'NONE', 3,
 ( #14079, #13678, #26066, #26477, #38466, #10639, #23022, #38873 ),
 .UNSPECIFIED., .F., .F.,
 ( 4, 2, 2, 4 ),
 ( 0.000000000000000000, 0.0004726692273637142245, 0.0007090038410455722041, 0.0009453384547274302921 ),
 .UNSPECIFIED. ) ;
#9808 = LINE ( 'NONE', #31540, #20852 ) ;
#9809 = CARTESIAN_POINT ( 'NONE',  ( 2.787905735463452661, 28.53453732066309811, 20.94377226548378701 ) ) ;
#9810 = VECTOR ( 'NONE', #14666, 1000.000000000000000 ) ;
#9811 = PLANE ( 'NONE',  #40158 ) ;
#9812 = VECTOR ( 'NONE', #3061, 1000.000000000000114 ) ;
#9813 = EDGE_CURVE ( 'NONE', #26679, #33392, #2882, .T. ) ;
#9814 = CARTESIAN_POINT ( 'NONE',  ( 3.458865582155095986, 18.48521636184714012, 12.00000000000000000 ) ) ;
#9815 = EDGE_CURVE ( 'NONE', #17253, #4988, #26897, .T. ) ;
#9816 = FACE_BOUND ( 'NONE', #24433, .T. ) ;
#9817 = CARTESIAN_POINT ( 'NONE',  ( 28.79337657215624802, 4.963436916936684540, 10.99999999998960654 ) ) ;
#9818 = CARTESIAN_POINT ( 'NONE',  ( -22.97007816870513608, 9.885904127924739271, -4.999999999999999112 ) ) ;
#9819 = CARTESIAN_POINT ( 'NONE',  ( 19.94105029877223600, -22.02225129578359031, -14.93283766574777616 ) ) ;
#9820 = DIRECTION ( 'NONE',  ( 1.000000000000000000, 0.000000000000000000, 0.000000000000000000 ) ) ;
#9821 = CARTESIAN_POINT ( 'NONE',  ( 10.93269978972138823, 17.59616206544103889, -27.43687381419555038 ) ) ;
#9822 = EDGE_LOOP ( 'NONE', ( #20590, #1411, #37169 ) ) ;
#9823 = CARTESIAN_POINT ( 'NONE',  ( -16.11342241529700914, 23.89935148421658440, -7.369744296171617748 ) ) ;
#9824 = CARTESIAN_POINT ( 'NONE',  ( -28.99614216520755150, -14.25990928191762919, 20.25080042701565120 ) ) ;
#9825 = CARTESIAN_POINT ( 'NONE',  ( 10.10646936306337906, 32.94553861768082470, 10.49999999999999822 ) ) ;
#9826 = CARTESIAN_POINT ( 'NONE',  ( 14.54923841115265759, 24.92455583907450034, -11.60034771649255703 ) ) ;
#9827 = ORIENTED_EDGE ( 'NONE', *, *, #5642, .T. ) ;
#9828 = FACE_OUTER_BOUND ( 'NONE', #33710, .T. ) ;
#9829 = ORIENTED_EDGE ( 'NONE', *, *, #19717, .T. ) ;
#9831 = LINE ( 'NONE', #890, #16674 ) ;
#9830 = CARTESIAN_POINT ( 'NONE',  ( -15.23769845792880950, 26.95939586459985549, -6.880603932344942386 ) ) ;
#9832 = CARTESIAN_POINT ( 'NONE',  ( -10.32384819220336958, -19.12984685317730182, -23.84136453349647766 ) ) ;
#9833 = EDGE_CURVE ( 'NONE', #2411, #37016, #32088, .T. ) ;
#9834 = DIRECTION ( 'NONE',  ( 0.000000000000000000, -0.000000000000000000, -1.000000000000000000 ) ) ;
#9835 = ORIENTED_EDGE ( 'NONE', *, *, #25365, .T. ) ;
#9836 = CARTESIAN_POINT ( 'NONE',  ( -32.80859633437859202, -14.68931420806718435, -10.18384796241277712 ) ) ;
#9837 = CARTESIAN_POINT ( 'NONE',  ( -11.36062271840278903, -22.05499941633807381, -17.51679325157146039 ) ) ;
#9838 = CARTESIAN_POINT ( 'NONE',  ( 10.14716901145161465, 12.46304090461738667, 13.00000000000000178 ) ) ;
#9839 = CARTESIAN_POINT ( 'NONE',  ( 12.83478968634269712, 16.45627959073583568, -26.38328025063007232 ) ) ;
#9840 = ORIENTED_EDGE ( 'NONE', *, *, #33524, .F. ) ;
#9841 = CARTESIAN_POINT ( 'NONE',  ( 26.59269643126366489, 4.672196685667098670, -6.910430442841478893 ) ) ;
#9842 = CIRCLE ( 'NONE', #7807, 1.000000000000000888 ) ;
#9843 = FACE_OUTER_BOUND ( 'NONE', #4588, .T. ) ;
#9844 = EDGE_CURVE ( 'NONE', #35248, #4321, #14575, .T. ) ;
#9845 = CARTESIAN_POINT ( 'NONE',  ( 9.427394655428274817, 11.06314620770945290, 11.00000000000000000 ) ) ;
#9846 = DIRECTION ( 'NONE',  ( -0.1045284632676569680, -0.9945218953682729568, 0.000000000000000000 ) ) ;
#9847 = ORIENTED_EDGE ( 'NONE', *, *, #18062, .T. ) ;
#9848 = CARTESIAN_POINT ( 'NONE',  ( -24.08328761345742208, 0.1459235441318743887, -19.45002103222414647 ) ) ;
#9849 = CARTESIAN_POINT ( 'NONE',  ( 22.79849040394648441, 0.3847677357643901619, -21.58657492048318716 ) ) ;
#9850 = CARTESIAN_POINT ( 'NONE',  ( 30.00904163739988206, -13.36872314231647607, 19.99202127657103389 ) ) ;
#9851 = ORIENTED_EDGE ( 'NONE', *, *, #26135, .T. ) ;
#9852 = AXIS2_PLACEMENT_3D ( 'NONE', #21341, #36777, #8544 ) ;
#9853 = CARTESIAN_POINT ( 'NONE',  ( -31.47283671532261806, -25.12609584734821766, -14.45070082761205477 ) ) ;
#9854 = CARTESIAN_POINT ( 'NONE',  ( 6.354454053420411697, 35.54304081427980577, 7.500000000000000888 ) ) ;
#9855 = ORIENTED_EDGE ( 'NONE', *, *, #39775, .F. ) ;
#9856 = CARTESIAN_POINT ( 'NONE',  ( 75.15099915297797395, 43.38844959084117647, 0.000000000000000000 ) ) ;
#9857 = EDGE_CURVE ( 'NONE', #14734, #2755, #27613, .T. ) ;
#9858 = EDGE_CURVE ( 'NONE', #32934, #16598, #24950, .T. ) ;
#9859 = CARTESIAN_POINT ( 'NONE',  ( -1.000000000000000000, 37.50000000000000711, 10.50000000000000178 ) ) ;
#9860 = FACE_OUTER_BOUND ( 'NONE', #15537, .T. ) ;
#9861 = CARTESIAN_POINT ( 'NONE',  ( 3.805984881634391748, 28.61912022499797104, -16.66590632089457458 ) ) ;
#9862 = DIRECTION ( 'NONE',  ( 0.000000000000000000, 0.000000000000000000, 1.000000000000000000 ) ) ;
#9863 = CARTESIAN_POINT ( 'NONE',  ( 14.36203778474857806, 19.98498072221368815, 10.49999999999999822 ) ) ;
#9864 = DIRECTION ( 'NONE',  ( 1.000000000000000000, 0.000000000000000000, 0.000000000000000000 ) ) ;
#9865 = DIRECTION ( 'NONE',  ( 0.000000000000000000, 0.000000000000000000, 1.000000000000000000 ) ) ;
#9866 = FACE_OUTER_BOUND ( 'NONE', #17960, .T. ) ;
#9867 = CARTESIAN_POINT ( 'NONE',  ( 10.22725543094859013, 18.04229054158819423, -27.38248356850343512 ) ) ;
#9868 = DIRECTION ( 'NONE',  ( 0.000000000000000000, 0.000000000000000000, 1.000000000000000000 ) ) ;
#9869 = ORIENTED_EDGE ( 'NONE', *, *, #8268, .F. ) ;
#9871 = CARTESIAN_POINT ( 'NONE',  ( 2.629601561899429285, 7.723830143584023311, 10.59344459855566889 ) ) ;
#9870 = CARTESIAN_POINT ( 'NONE',  ( -17.97959330666300559, 18.28784316811839972, -9.349175424125363065 ) ) ;
#9872 = CARTESIAN_POINT ( 'NONE',  ( 36.53369576860742995, -5.154516326609290822, 11.00000000000008527 ) ) ;
#9873 = AXIS2_PLACEMENT_3D ( 'NONE', #21247, #2569, #33657 ) ;
#9874 = CARTESIAN_POINT ( 'NONE',  ( 9.960472199639074375, -18.81618559987053985, -25.01525443589214248 ) ) ;
#9875 = CARTESIAN_POINT ( 'NONE',  ( -5.982165713378357452, 28.55918256678905465, 9.000000000000001776 ) ) ;
#9876 = CARTESIAN_POINT ( 'NONE',  ( 14.74364839002157979, 25.37821730288758459, -10.65361825091638615 ) ) ;
#9877 = ORIENTED_EDGE ( 'NONE', *, *, #10314, .T. ) ;
#9878 = CARTESIAN_POINT ( 'NONE',  ( 15.33243761980678599, 26.63804497122816528, -6.887548222410910803 ) ) ;
#9879 = EDGE_LOOP ( 'NONE', ( #19015, #23541 ) ) ;
#9880 = CARTESIAN_POINT ( 'NONE',  ( 0.000000000000000000, 22.50000000000000355, 12.00000000000000000 ) ) ;
#9881 = CARTESIAN_POINT ( 'NONE',  ( -13.97427186057036863, -24.60121427642448921, -12.55298982698177390 ) ) ;
#9882 = EDGE_CURVE ( 'NONE', #25824, #8022, #7427, .T. ) ;
#9883 = CARTESIAN_POINT ( 'NONE',  ( -26.37421498764311778, -27.66411951031046357, 12.73282698324853257 ) ) ;
#9884 = AXIS2_PLACEMENT_3D ( 'NONE', #5591, #2556, #22717 ) ;
#9885 = CARTESIAN_POINT ( 'NONE',  ( -29.03261643272151815, -20.06036525406060633, -11.07436732675348523 ) ) ;
#9886 = CARTESIAN_POINT ( 'NONE',  ( -1.996201064919716606, -21.64193600980604515, -21.17403543307457170 ) ) ;
#9887 = CARTESIAN_POINT ( 'NONE',  ( 13.28169970595349803, 21.08631984670124027, -17.49495114793986161 ) ) ;
#9889 = EDGE_CURVE ( 'NONE', #27233, #35146, #21326, .T. ) ;
#9888 = ORIENTED_EDGE ( 'NONE', *, *, #17590, .T. ) ;
#9890 = CARTESIAN_POINT ( 'NONE',  ( 19.72017037454142141, 9.080320345084325950, -21.16391035189845482 ) ) ;
#9891 = CARTESIAN_POINT ( 'NONE',  ( 9.038010526469520300, 11.76154733104316819, 9.500000000000000000 ) ) ;
#9892 = CARTESIAN_POINT ( 'NONE',  ( 13.31084379716732613, 29.56959138546320887, 17.42190598798392287 ) ) ;
#9893 = ORIENTED_EDGE ( 'NONE', *, *, #23942, .T. ) ;
#9894 = CARTESIAN_POINT ( 'NONE',  ( -31.96359514549918757, -3.261425111024537582, -9.982721131112327839 ) ) ;
#9895 = ADVANCED_FACE ( 'NONE', ( #16423 ), #3548, .T. ) ;
#9896 = CARTESIAN_POINT ( 'NONE',  ( -14.01880647376396993, 20.72057097100359968, 18.87996532025877627 ) ) ;
#9897 = VECTOR ( 'NONE', #30571, 1000.000000000000000 ) ;
#9898 = VERTEX_POINT ( 'NONE', #10326 ) ;
#9899 = CARTESIAN_POINT ( 'NONE',  ( 1.838889047819958655, 31.15129278236397781, 9.000000000000001776 ) ) ;
#9900 = CARTESIAN_POINT ( 'NONE',  ( 7.559505275947156377, 25.28115294937476065, 13.00000000000000178 ) ) ;
#9901 = B_SPLINE_CURVE_WITH_KNOTS ( 'NONE', 3,
 ( #38445, #32762, #11221, #11025, #23611, #19962, #22795, #22997 ),
 .UNSPECIFIED., .F., .F.,
 ( 4, 2, 2, 4 ),
 ( 0.000000000000000000, 0.0004726692273637109177, 0.0007090038410455688431, 0.0009453384547274268227 ),
 .UNSPECIFIED. ) ;
#9902 = CARTESIAN_POINT ( 'NONE',  ( -20.42898406783283960, 2.211777317264515652, -28.75134568260269674 ) ) ;
#9903 = CARTESIAN_POINT ( 'NONE',  ( 34.24928854971908976, -14.99804081630860608, -7.982871076175817926 ) ) ;
#9904 = AXIS2_PLACEMENT_3D ( 'NONE', #10374, #6168, #15915 ) ;
#9905 = CARTESIAN_POINT ( 'NONE',  ( 29.72906145568107306, -25.76693493179220340, 13.32518128616587560 ) ) ;
#9906 = ORIENTED_EDGE ( 'NONE', *, *, #13876, .T. ) ;
#9907 = CIRCLE ( 'NONE', #1471, 15.00000000000000000 ) ;
#9908 = ORIENTED_EDGE ( 'NONE', *, *, #36332, .F. ) ;
#9909 = DIRECTION ( 'NONE',  ( -0.3535533905932713994, 0.6123724356958013537, -0.7071067811865427988 ) ) ;
#9910 = DIRECTION ( 'NONE',  ( 0.000000000000000000, 0.000000000000000000, 1.000000000000000000 ) ) ;
#9911 = EDGE_CURVE ( 'NONE', #2500, #5105, #10690, .T. ) ;
#9912 = ADVANCED_FACE ( 'NONE', ( #15823 ), #12967, .F. ) ;
#9913 = CIRCLE ( 'NONE', #26119, 1.000000000000000000 ) ;
#9914 = DIRECTION ( 'NONE',  ( 0.000000000000000000, 0.000000000000000000, 1.000000000000000000 ) ) ;
#9915 = ORIENTED_EDGE ( 'NONE', *, *, #11064, .T. ) ;
#9916 = CARTESIAN_POINT ( 'NONE',  ( -0.4101013132653836823, 21.15020722337806447, -26.25491541755722480 ) ) ;
#9917 = CARTESIAN_POINT ( 'NONE',  ( 8.412270287199559604, 10.07085245822950981, 10.49999999999999822 ) ) ;
#9918 = DIRECTION ( 'NONE',  ( 0.2079116908177533474, -0.9781476007338067991, 0.000000000000000000 ) ) ;
#9919 = LINE ( 'NONE', #30862, #19533 ) ;
#9920 = DIRECTION ( 'NONE',  ( 0.000000000000000000, 0.000000000000000000, 1.000000000000000000 ) ) ;
#9921 = LINE ( 'NONE', #22301, #17781 ) ;
#9922 = CARTESIAN_POINT ( 'NONE',  ( 11.66971972310407146, 25.75749872935682561, -15.14234555051886666 ) ) ;
#9923 = CARTESIAN_POINT ( 'NONE',  ( 2.143544478356361971, 7.864861742947437229, 10.49999999999999645 ) ) ;
#9924 = VERTEX_POINT ( 'NONE', #389 ) ;
#9925 = CARTESIAN_POINT ( 'NONE',  ( -21.19257405417214812, 12.68336146040521761, -6.940464740854612735 ) ) ;
#9926 = VECTOR ( 'NONE', #33961, 1000.000000000000227 ) ;
#9927 = CARTESIAN_POINT ( 'NONE',  ( 18.68934290553362132, 29.94321432092800350, 11.00000000000000000 ) ) ;
#9928 = CARTESIAN_POINT ( 'NONE',  ( 10.00997369995331177, -18.79612801155203883, -25.00947302926656235 ) ) ;
#9929 = LINE ( 'NONE', #25557, #15264 ) ;
#9930 = CARTESIAN_POINT ( 'NONE',  ( 15.31424333055854170, 26.70176439337667773, -6.886156298975530277 ) ) ;
#9931 = CARTESIAN_POINT ( 'NONE',  ( 19.54664213359407654, -11.28525909758385914, -30.00000000000003908 ) ) ;
#9932 = DIRECTION ( 'NONE',  ( 0.000000000000000000, 0.000000000000000000, -1.000000000000000000 ) ) ;
#9933 = MECHANICAL_DESIGN_GEOMETRIC_PRESENTATION_REPRESENTATION (  '', ( #222 ), #22915 ) ;
#9934 = CARTESIAN_POINT ( 'NONE',  ( -21.19775588263476251, -22.46636194237366269, -13.96214201008129763 ) ) ;
#9935 = CARTESIAN_POINT ( 'NONE',  ( 6.152249614461454463, -24.82641286710474660, -8.379856565498640109 ) ) ;
#9936 = CARTESIAN_POINT ( 'NONE',  ( 11.28733053642023698, 17.68149975644739058, -26.23582624851832534 ) ) ;
#9937 = EDGE_CURVE ( 'NONE', #26679, #21646, #988, .T. ) ;
#9938 = CARTESIAN_POINT ( 'NONE',  ( 17.85505465768944333, -12.86254080347576512, -24.24539029509336885 ) ) ;
#9939 = CARTESIAN_POINT ( 'NONE',  ( 9.331903152615748098, 11.35703883385568780, 11.00000000000000000 ) ) ;
#9940 = CARTESIAN_POINT ( 'NONE',  ( -10.49474413300070097, 21.89971208337388120, 10.50000000000000000 ) ) ;
#9941 = ORIENTED_EDGE ( 'NONE', *, *, #11540, .T. ) ;
#9942 = CARTESIAN_POINT ( 'NONE',  ( -8.350843205241419653, 35.56854215007076903, -7.588859392928601011 ) ) ;
#9943 = CARTESIAN_POINT ( 'NONE',  ( 6.354454053420409920, 35.54304081427980577, 9.500000000000000000 ) ) ;
#9944 = VERTEX_POINT ( 'NONE', #7066 ) ;
#9945 = CARTESIAN_POINT ( 'NONE',  ( 22.22902049279901959, 0.6319665380888792594, -22.73092917304706972 ) ) ;
#9946 = CARTESIAN_POINT ( 'NONE',  ( -3.465511072935358428, 38.21601825462828828, -5.000000000000000000 ) ) ;
#9947 = CARTESIAN_POINT ( 'NONE',  ( -23.05386822411323422, -7.747535282638357224, 20.99999999999999645 ) ) ;
#9948 = VERTEX_POINT ( 'NONE', #19262 ) ;
#9949 = CARTESIAN_POINT ( 'NONE',  ( -29.76070246994180479, 0.08935854291201565658, -9.710064343477942117 ) ) ;
#9950 = DIRECTION ( 'NONE',  ( 1.000000000000000000, 0.000000000000000000, 0.000000000000000000 ) ) ;
#9951 = CIRCLE ( 'NONE', #24849, 0.5000000000000004441 ) ;
#9952 = ORIENTED_EDGE ( 'NONE', *, *, #34721, .T. ) ;
#9953 = CARTESIAN_POINT ( 'NONE',  ( 20.48269730678144995, -4.854230542895870748, -26.43053413679163555 ) ) ;
#9954 = VECTOR ( 'NONE', #27751, 1000.000000000000000 ) ;
#9955 = EDGE_LOOP ( 'NONE', ( #21237, #5705, #32790, #23349, #17257, #24327, #12684 ) ) ;
#9956 = CARTESIAN_POINT ( 'NONE',  ( -15.98961535660673938, 30.99268274074335494, 11.55979286843903608 ) ) ;
#9957 = FACE_OUTER_BOUND ( 'NONE', #16339, .T. ) ;
#9958 = CARTESIAN_POINT ( 'NONE',  ( -18.72695399103857739, -3.339292870217068998, 23.00000000000000355 ) ) ;
#9959 = CARTESIAN_POINT ( 'NONE',  ( -1.410291641398624174, 35.53022820328502007, 18.87996532025784546 ) ) ;
#9960 = STYLED_ITEM ( 'NONE', ( #21657 ), #8826 ) ;
#9961 = DIRECTION ( 'NONE',  ( 1.000000000000000000, 0.000000000000000000, 0.000000000000000000 ) ) ;
#9962 = ORIENTED_EDGE ( 'NONE', *, *, #27023, .F. ) ;
#9963 = DIRECTION ( 'NONE',  ( 0.5000000000000038858, 0.8660254037844363761, 0.000000000000000000 ) ) ;
#9964 = CARTESIAN_POINT ( 'NONE',  ( -18.68149877921488766, -8.466985313562505056, -30.00000000000001421 ) ) ;
#9965 = CARTESIAN_POINT ( 'NONE',  ( 12.74038105676653920, 14.56698729810772619, 10.50000000000000000 ) ) ;
#9966 = EDGE_CURVE ( 'NONE', #5508, #35565, #16022, .T. ) ;
#9967 = CARTESIAN_POINT ( 'NONE',  ( -9.541476348891238857, 27.59512447410525127, 12.00000000000000000 ) ) ;
#9968 = CARTESIAN_POINT ( 'NONE',  ( 14.27219392008591292, 14.71651433334269043, -29.40509136628979547 ) ) ;
#9969 = CARTESIAN_POINT ( 'NONE',  ( 8.657666503606854747, 33.55139795693855831, -10.25229396191044273 ) ) ;
#9970 = AXIS2_PLACEMENT_3D ( 'NONE', #15607, #24948, #3608 ) ;
#9971 = EDGE_LOOP ( 'NONE', ( #3286, #4263, #21759, #1641 ) ) ;
#9972 = CARTESIAN_POINT ( 'NONE',  ( 15.74238530928792201, -25.84026302488051385, -10.12512499451556813 ) ) ;
#9973 = CARTESIAN_POINT ( 'NONE',  ( 1.082972213713614407, 27.41125570341916529, 20.99999999999998934 ) ) ;
#9974 = DIRECTION ( 'NONE',  ( 1.000000000000000000, 0.000000000000000000, 0.000000000000000000 ) ) ;
#9975 = EDGE_LOOP ( 'NONE', ( #14329, #13582 ) ) ;
#9976 = CARTESIAN_POINT ( 'NONE',  ( -15.41471391286399317, 26.78795929021520550, -5.000000000000001776 ) ) ;
#9977 = AXIS2_PLACEMENT_3D ( 'NONE', #16157, #15959, #26090 ) ;
#9978 = CARTESIAN_POINT ( 'NONE',  ( -33.08367492452225633, -6.388370399452986348, 17.92354375535292021 ) ) ;
#9979 = CARTESIAN_POINT ( 'NONE',  ( 14.19115657440825728, -25.54240891117661860, -10.19065319804806258 ) ) ;
#9980 = CARTESIAN_POINT ( 'NONE',  ( 1.605696033269625955, 17.55816537872232530, 13.00000000000000178 ) ) ;
#9981 = ORIENTED_EDGE ( 'NONE', *, *, #26713, .T. ) ;
#9982 = EDGE_LOOP ( 'NONE', ( #21450, #20856, #27677 ) ) ;
#9983 = CARTESIAN_POINT ( 'NONE',  ( -8.291215257814828377, 18.82905498736118588, -28.59874454941313360 ) ) ;
#9984 = LINE ( 'NONE', #19731, #26931 ) ;
#9985 = CARTESIAN_POINT ( 'NONE',  ( -14.98890121934603314, -28.67928442654204346, 11.00000000000000000 ) ) ;
#9986 = CONICAL_SURFACE ( 'NONE', #19097, 1.000000000000006883, 0.7853981633974547183 ) ;
#9987 = CARTESIAN_POINT ( 'NONE',  ( -28.12294647621138921, -8.736892962676476415, -15.78945194607744895 ) ) ;
#9988 = CYLINDRICAL_SURFACE ( 'NONE', #39751, 1.000000000000000000 ) ;
#9989 = VERTEX_POINT ( 'NONE', #19071 ) ;
#9990 = CARTESIAN_POINT ( 'NONE',  ( 20.60369210407207063, 0.9606588650137843910, -28.08297012610058019 ) ) ;
#9991 = CARTESIAN_POINT ( 'NONE',  ( -2.229437847141422679, 24.50739181907689712, 6.000000000000000000 ) ) ;
#9992 = CARTESIAN_POINT ( 'NONE',  ( 6.572794801194151049, 16.58182897866491956, 9.000000000000001776 ) ) ;
#9993 = EDGE_CURVE ( 'NONE', #22329, #11380, #22113, .T. ) ;
#9994 = ORIENTED_EDGE ( 'NONE', *, *, #23785, .F. ) ;
#9995 = CARTESIAN_POINT ( 'NONE',  ( -21.71849452838645789, 0.6790819573452312463, -23.84809452429628607 ) ) ;
#9996 = ORIENTED_EDGE ( 'NONE', *, *, #22037, .T. ) ;
#9997 = CARTESIAN_POINT ( 'NONE',  ( 25.83202993258364089, -0.8389207943029072245, -17.28593405758972779 ) ) ;
#9998 = AXIS2_PLACEMENT_3D ( 'NONE', #11117, #4003, #17015 ) ;
#9999 = DIRECTION ( 'NONE',  ( -0.000000000000000000, -0.000000000000000000, -1.000000000000000000 ) ) ;
#10000 = CARTESIAN_POINT ( 'NONE',  ( 33.34742602403141376, -19.25314539175541384, 16.30093088680190405 ) ) ;
#10001 = VERTEX_POINT ( 'NONE', #7264 ) ;
#10002 = CARTESIAN_POINT ( 'NONE',  ( -11.38745366800335646, 34.53793118711397625, 15.72805884749017835 ) ) ;
#10003 = LINE ( 'NONE', #35188, #21495 ) ;
#10004 = CARTESIAN_POINT ( 'NONE',  ( 6.175735745372842089, 24.95935742585800199, 20.94377226548417781 ) ) ;
#10005 = AXIS2_PLACEMENT_3D ( 'NONE', #26151, #29405, #35507 ) ;
#10006 = CARTESIAN_POINT ( 'NONE',  ( -12.74038105676665289, 14.56698729810790027, 7.000000000000000000 ) ) ;
#10007 = EDGE_CURVE ( 'NONE', #36443, #11532, #31662, .T. ) ;
#10008 = DIRECTION ( 'NONE',  ( 1.000000000000000000, 0.000000000000000000, -0.000000000000000000 ) ) ;
#10009 = B_SPLINE_SURFACE_WITH_KNOTS ( 'NONE', 1, 3, ( 
 ( #18686, #31077, #3244, #15635, #19273, #34720, #31672, #34325, #18884, #31274 ),
 ( #22124, #34524, #31472, #20648, #39321, #2360, #13579, #36082, #23127, #33049 ) ),
 .UNSPECIFIED., .F., .F., .F.,
 ( 2, 2 ),
 ( 4, 2, 2, 2, 4 ),
 ( 0.000000000000000000, 1.000000000000000000 ),
 ( 1.265795420569473695, 1.658494502268196502, 2.051193583966919309, 2.443892665665642117, 2.836591747364364924 ),
 .UNSPECIFIED. ) ;
#10010 = VECTOR ( 'NONE', #24965, 1000.000000000000000 ) ;
#10011 = DIRECTION ( 'NONE',  ( 1.000000000000000000, 0.000000000000000000, -0.000000000000000000 ) ) ;
#10012 = EDGE_CURVE ( 'NONE', #29252, #697, #32802, .T. ) ;
#10013 = CARTESIAN_POINT ( 'NONE',  ( 20.48347041321109430, 17.67745015983098966, 12.73282698324788953 ) ) ;
#10014 = CARTESIAN_POINT ( 'NONE',  ( -19.34217367975503876, 7.121619937563573366, -27.70688438477295179 ) ) ;
#10015 = EDGE_CURVE ( 'NONE', #7168, #27126, #38154, .T. ) ;
#10016 = CARTESIAN_POINT ( 'NONE',  ( 15.00527517599701710, -17.60829065308229247, -22.19583011995415589 ) ) ;
#10017 = DIRECTION ( 'NONE',  ( 0.000000000000000000, 0.000000000000000000, 1.000000000000000000 ) ) ;
#10018 = CARTESIAN_POINT ( 'NONE',  ( 11.04596197333746055, 17.85565203605465001, -26.20988823588121619 ) ) ;
#10019 = EDGE_LOOP ( 'NONE', ( #35480, #20043, #37666, #26433 ) ) ;
#10020 = CIRCLE ( 'NONE', #28205, 0.5000000000000013323 ) ;
#10021 = CARTESIAN_POINT ( 'NONE',  ( -15.22570016247339808, 24.01659300293151489, -10.68444636275925141 ) ) ;
#10022 = CARTESIAN_POINT ( 'NONE',  ( -23.50870743262444762, -18.52420134090459314, 20.69868183039763210 ) ) ;
#10023 = DIRECTION ( 'NONE',  ( 1.000000000000000000, 0.000000000000000000, 0.000000000000000000 ) ) ;
#10024 = CARTESIAN_POINT ( 'NONE',  ( 14.05306866902358820, 23.88062157653425643, -13.51576454616971645 ) ) ;
#10025 = ORIENTED_EDGE ( 'NONE', *, *, #30939, .F. ) ;
#10026 = CARTESIAN_POINT ( 'NONE',  ( 27.88439565352735272, -14.28169649418448728, -14.73373279294286498 ) ) ;
#10027 = CARTESIAN_POINT ( 'NONE',  ( 2.587660364795204782, 9.681887955242936883, 6.000000000000000000 ) ) ;
#10028 = EDGE_LOOP ( 'NONE', ( #10422, #32834, #19828, #20633 ) ) ;
#10030 = FACE_OUTER_BOUND ( 'NONE', #35411, .T. ) ;
#10029 = CARTESIAN_POINT ( 'NONE',  ( -15.05229008872046670, 26.98958926311531670, -7.808750500632839930 ) ) ;
#10031 = CARTESIAN_POINT ( 'NONE',  ( -12.83236629447386079, -21.40442163443030310, -18.34045313207591832 ) ) ;
#10032 = DIRECTION ( 'NONE',  ( 0.000000000000000000, 0.000000000000000000, 1.000000000000000000 ) ) ;
#10033 = ORIENTED_EDGE ( 'NONE', *, *, #20080, .T. ) ;
#10034 = CARTESIAN_POINT ( 'NONE',  ( -21.35353645564259750, -10.38814595318204326, -21.85098217641707308 ) ) ;
#10035 = CARTESIAN_POINT ( 'NONE',  ( -9.453848434180018856, -19.01651734649589898, -25.07122770737407080 ) ) ;
#10036 = DIRECTION ( 'NONE',  ( 0.6123724356958029080, 0.3535533905932708998, -0.7071067811865417996 ) ) ;
#10037 = CARTESIAN_POINT ( 'NONE',  ( 15.79381377564608613, 22.93146731034228480, -10.23294722842091353 ) ) ;
#10038 = VERTEX_POINT ( 'NONE', #22707 ) ;
#10039 = CARTESIAN_POINT ( 'NONE',  ( 24.48878357941496375, 5.471706907836950684, -12.77386761934589288 ) ) ;
#10040 = CARTESIAN_POINT ( 'NONE',  ( -12.37435565298220119, 15.93301270189233598, 10.00000000000000000 ) ) ;
#10041 = EDGE_CURVE ( 'NONE', #11410, #2015, #12769, .T. ) ;
#10042 = FACE_OUTER_BOUND ( 'NONE', #36056, .T. ) ;
#10043 = ADVANCED_FACE ( 'NONE', ( #29013 ), #3627, .F. ) ;
#10044 = CARTESIAN_POINT ( 'NONE',  ( -10.79197459925262947, 32.88995393993013749, 10.68306085400104699 ) ) ;
#10045 = ORIENTED_EDGE ( 'NONE', *, *, #17021, .T. ) ;
#10046 = CARTESIAN_POINT ( 'NONE',  ( -30.14783002406086609, -0.3420316433952748647, -9.682860013783926689 ) ) ;
#10047 = VECTOR ( 'NONE', #13209, 1000.000000000000227 ) ;
#10048 = CARTESIAN_POINT ( 'NONE',  ( 30.85995981617431028, -0.2746738912069357497, -7.348642656983717991 ) ) ;
#10049 = CARTESIAN_POINT ( 'NONE',  ( 28.99614216520691912, -14.25990928191685470, 20.25080042701567606 ) ) ;
#10050 = VERTEX_POINT ( 'NONE', #781 ) ;
#10051 = CIRCLE ( 'NONE', #36651, 1.000000000000000000 ) ;
#10052 = CARTESIAN_POINT ( 'NONE',  ( 7.289639608743135213, -27.06962010326278190, -5.000000000000004441 ) ) ;
#10053 = DIRECTION ( 'NONE',  ( 1.000000000000000000, 0.000000000000000000, 0.000000000000000000 ) ) ;
#10054 = ORIENTED_EDGE ( 'NONE', *, *, #17470, .F. ) ;
#10055 = DIRECTION ( 'NONE',  ( 0.6691306063588671194, 0.7431448254773863615, -0.000000000000000000 ) ) ;
#10056 = EDGE_CURVE ( 'NONE', #18776, #9701, #13163, .T. ) ;
#10057 = DIRECTION ( 'NONE',  ( -1.000000000000000000, 0.000000000000000000, 0.000000000000000000 ) ) ;
#10058 = CARTESIAN_POINT ( 'NONE',  ( 19.07667540469735101, 16.81475038977109548, -5.000000000000001776 ) ) ;
#10059 = CARTESIAN_POINT ( 'NONE',  ( 2.790657799059328426, 21.23657145591617379, -25.61566959286999179 ) ) ;
#10060 = FACE_BOUND ( 'NONE', #21032, .T. ) ;
#10061 = ORIENTED_EDGE ( 'NONE', *, *, #4044, .T. ) ;
#10062 = CARTESIAN_POINT ( 'NONE',  ( 0.2655024426717602637, 36.24516302788250499, 6.000000000000000000 ) ) ;
#10063 = CARTESIAN_POINT ( 'NONE',  ( -8.927394655428429360, 11.06314620770957191, 9.500000000000000000 ) ) ;
#10064 = CARTESIAN_POINT ( 'NONE',  ( 29.26826387686844910, -23.91120845623157010, -5.000000000000000888 ) ) ;
#10065 = CARTESIAN_POINT ( 'NONE',  ( 7.824485034907089798, 10.87986945260445992, 9.500000000000000000 ) ) ;
#10066 = DIRECTION ( 'NONE',  ( 0.000000000000000000, 0.000000000000000000, 1.000000000000000000 ) ) ;
#10067 = CYLINDRICAL_SURFACE ( 'NONE', #7395, 0.4999999999999983902 ) ;
#10068 = AXIS2_PLACEMENT_3D ( 'NONE', #11737, #27174, #15179 ) ;
#10069 = CARTESIAN_POINT ( 'NONE',  ( 10.76512838780859660, 18.45021222265605232, -24.94022975695240874 ) ) ;
#10070 = DIRECTION ( 'NONE',  ( -0.9510565162951503115, 0.3090169943749573878, -0.000000000000000000 ) ) ;
#10071 = ORIENTED_EDGE ( 'NONE', *, *, #4143, .T. ) ;
#10073 = CARTESIAN_POINT ( 'NONE',  ( 2.291516524179206815, 7.763791616332271772, 10.49999999999999822 ) ) ;
#10072 = CARTESIAN_POINT ( 'NONE',  ( -15.67910400704473517, 18.03213292446707783, -16.76744236533109245 ) ) ;
#10074 = CARTESIAN_POINT ( 'NONE',  ( 34.10020663062358182, -21.93670956716295350, 10.99999999999994138 ) ) ;
#10075 = CARTESIAN_POINT ( 'NONE',  ( 12.99182960350822214, -23.09069332813563946, -15.45185403630547150 ) ) ;
#10076 = DIRECTION ( 'NONE',  ( 0.000000000000000000, 0.000000000000000000, 1.000000000000000000 ) ) ;
#10077 = CARTESIAN_POINT ( 'NONE',  ( 14.84680087938761872, 25.58880802702974933, -10.18073488593564413 ) ) ;
#10078 = VERTEX_POINT ( 'NONE', #1188 ) ;
#10079 = CARTESIAN_POINT ( 'NONE',  ( 14.52843121217837030, 24.98140828273265157, -11.59866322938457728 ) ) ;
#10080 = ORIENTED_EDGE ( 'NONE', *, *, #20930, .F. ) ;
#10081 = CIRCLE ( 'NONE', #28234, 0.5000000000000004441 ) ;
#10082 = CARTESIAN_POINT ( 'NONE',  ( 14.44923221060104090, 26.57085556310762087, 10.49999999999999822 ) ) ;
#10083 = CARTESIAN_POINT ( 'NONE',  ( -13.70756163817629414, -24.11668832361970161, -13.51384470570144458 ) ) ;
#10084 = CARTESIAN_POINT ( 'NONE',  ( -31.16314261583334044, -24.50336240592838521, 13.32518128616608699 ) ) ;
#10085 = AXIS2_PLACEMENT_3D ( 'NONE', #25300, #324, #9470 ) ;
#10086 = CIRCLE ( 'NONE', #25014, 5.999999999999994671 ) ;
#10087 = CARTESIAN_POINT ( 'NONE',  ( -23.30856450506559341, -17.15677614324469502, -16.65319078585623913 ) ) ;
#10088 = CARTESIAN_POINT ( 'NONE',  ( -2.199171785053767980, -22.69879091448489916, -16.97731724952892662 ) ) ;
#10089 = CARTESIAN_POINT ( 'NONE',  ( 12.45205971826092473, 19.54394706486126054, -20.59674335405842882 ) ) ;
#10090 = VERTEX_POINT ( 'NONE', #6862 ) ;
#10091 = CARTESIAN_POINT ( 'NONE',  ( 18.28802337575010384, 9.378636759438260029, -28.29756235655922225 ) ) ;
#10092 = CARTESIAN_POINT ( 'NONE',  ( 35.48557158694710978, -12.46552367096746217, -4.999999999999999112 ) ) ;
#10093 = CARTESIAN_POINT ( 'NONE',  ( -12.85888779259178705, 31.22252129899196049, 16.87380292611441135 ) ) ;
#10094 = EDGE_LOOP ( 'NONE', ( #207, #38168, #1233 ) ) ;
#10095 = CARTESIAN_POINT ( 'NONE',  ( -33.12478769974119786, -4.346059658142014115, -8.586455447396705409 ) ) ;
#10096 = EDGE_CURVE ( 'NONE', #23174, #20519, #6468, .T. ) ;
#10097 = CARTESIAN_POINT ( 'NONE',  ( -23.68624114773478695, 7.604278122839970955, 16.87380292611488741 ) ) ;
#10098 = ORIENTED_EDGE ( 'NONE', *, *, #13544, .T. ) ;
#10099 = CYLINDRICAL_SURFACE ( 'NONE', #22603, 1.000000000000000888 ) ;
#10100 = PLANE ( 'NONE',  #13494 ) ;
#10101 = CARTESIAN_POINT ( 'NONE',  ( 22.52679405684453329, -9.890575151869189341, -20.72956160231121103 ) ) ;
#10102 = CARTESIAN_POINT ( 'NONE',  ( 18.84567888139518388, -29.34375185562596045, 11.55979286843977327 ) ) ;
#10103 = ORIENTED_EDGE ( 'NONE', *, *, #18716, .F. ) ;
#10104 = VERTEX_POINT ( 'NONE', #25356 ) ;
#10105 = DIRECTION ( 'NONE',  ( -0.7071067811865500152, 1.645406930227287500E-16, 0.7071067811865451302 ) ) ;
#10106 = AXIS2_PLACEMENT_3D ( 'NONE', #24421, #11641, #40 ) ;
#10107 = CARTESIAN_POINT ( 'NONE',  ( 0.6056960332696259552, 17.55816537872232530, 13.00000000000000178 ) ) ;
#10108 = EDGE_CURVE ( 'NONE', #7803, #172, #15905, .T. ) ;
#10109 = VECTOR ( 'NONE', #30714, 1000.000000000000227 ) ;
#10110 = AXIS2_PLACEMENT_3D ( 'NONE', #11539, #23726, #8080 ) ;
#10111 = DIRECTION ( 'NONE',  ( -1.000000000000000000, 0.000000000000000000, 0.000000000000000000 ) ) ;
#10112 = ORIENTED_EDGE ( 'NONE', *, *, #23517, .T. ) ;
#10113 = EDGE_CURVE ( 'NONE', #3294, #32472, #9929, .T. ) ;
#10114 = CARTESIAN_POINT ( 'NONE',  ( -1.894380261295754098, 37.63992458223975746, -7.973046867981261165 ) ) ;
#10115 = PLANE ( 'NONE',  #32125 ) ;
#10116 = AXIS2_PLACEMENT_3D ( 'NONE', #25113, #534, #35057 ) ;
#10117 = PLANE ( 'NONE',  #18862 ) ;
#10118 = CARTESIAN_POINT ( 'NONE',  ( 3.992867117591230919, 8.524771480177550487, 7.499999999999990230 ) ) ;
#10119 = CARTESIAN_POINT ( 'NONE',  ( -14.52509594610762456, 21.97885917798744870, 10.49999999999999467 ) ) ;
#10120 = CARTESIAN_POINT ( 'NONE',  ( -13.37378135583787220, 20.59160479820268108, 7.000000000000000000 ) ) ;
#10121 = CARTESIAN_POINT ( 'NONE',  ( 9.285927727562647505, 18.34037923570121009, -28.63677830487614528 ) ) ;
#10122 = CARTESIAN_POINT ( 'NONE',  ( -3.000488737322915878, 30.46850471150003159, 7.000000000000000000 ) ) ;
#10123 = ORIENTED_EDGE ( 'NONE', *, *, #17055, .F. ) ;
#10124 = ADVANCED_FACE ( 'NONE', ( #4022 ), #585, .T. ) ;
#10126 = CARTESIAN_POINT ( 'NONE',  ( -5.767236651883564491, 13.71142893291686349, 11.00000000000000000 ) ) ;
#10125 = CARTESIAN_POINT ( 'NONE',  ( -18.22877391798860458, 10.85510818490154250, -23.33390808761037860 ) ) ;
#10127 = CARTESIAN_POINT ( 'NONE',  ( -15.33540832684527544, 35.51988609203762337, 22.99999999999999289 ) ) ;
#10128 = CARTESIAN_POINT ( 'NONE',  ( 14.09698363156053524, -24.62026783164278498, -12.54657184365754752 ) ) ;
#10129 = CARTESIAN_POINT ( 'NONE',  ( -11.14717575287011542, 32.53695909538323860, 13.00000000000000178 ) ) ;
#10130 = CARTESIAN_POINT ( 'NONE',  ( 10.94214493613176664, 17.33550160327741096, -29.34744205922653393 ) ) ;
#10131 = CARTESIAN_POINT ( 'NONE',  ( -19.79815887584811307, 19.84782313723621883, -4.999999999999999112 ) ) ;
#10132 = CARTESIAN_POINT ( 'NONE',  ( -10.20374679324127776, 33.03312760923218150, 10.49999999999999822 ) ) ;
#10133 = CARTESIAN_POINT ( 'NONE',  ( -19.86385295935389550, -21.04324079092269173, -15.86974588982537782 ) ) ;
#10134 = CARTESIAN_POINT ( 'NONE',  ( 7.644341925271119997, -20.35065011595537499, -23.04646567544028812 ) ) ;
#10135 = CARTESIAN_POINT ( 'NONE',  ( 11.40938548045612499, 17.96021580865084744, -25.02785325939463235 ) ) ;
#10136 = CARTESIAN_POINT ( 'NONE',  ( 20.81850934979185652, -15.01608711947214481, -19.65698525133124264 ) ) ;
#10137 = CARTESIAN_POINT ( 'NONE',  ( 7.852310722358922135, 10.04909572729066269, 10.49999999999999822 ) ) ;
#10138 = CARTESIAN_POINT ( 'NONE',  ( 11.22168704032814013, 31.70696390855182756, 10.83333333333333393 ) ) ;
#10140 = ORIENTED_EDGE ( 'NONE', *, *, #6400, .T. ) ;
#10139 = EDGE_CURVE ( 'NONE', #22765, #19611, #21101, .T. ) ;
#10141 = CARTESIAN_POINT ( 'NONE',  ( -8.279978381213238592, 30.99040824897319979, -13.00426055310639839 ) ) ;
#10142 = CIRCLE ( 'NONE', #39976, 1.000000000000000000 ) ;
#10143 = EDGE_CURVE ( 'NONE', #32505, #33425, #4880, .T. ) ;
#10144 = EDGE_CURVE ( 'NONE', #14996, #15350, #28860, .T. ) ;
#10145 = AXIS2_PLACEMENT_3D ( 'NONE', #22864, #3980, #19832 ) ;
#10146 = CARTESIAN_POINT ( 'NONE',  ( -3.503793317224518145, 8.420815634768723967, 7.000000000000000000 ) ) ;
#10147 = ORIENTED_EDGE ( 'NONE', *, *, #26670, .T. ) ;
#10148 = CARTESIAN_POINT ( 'NONE',  ( 25.22159695029489512, 0.3595918362293377135, -17.43676678839515759 ) ) ;
#10149 = CYLINDRICAL_SURFACE ( 'NONE', #34919, 6.000000000000001776 ) ;
#10150 = AXIS2_PLACEMENT_3D ( 'NONE', #36675, #8845, #9238 ) ;
#10151 = CARTESIAN_POINT ( 'NONE',  ( -12.80736835487442349, 15.68301270189233954, 9.000000000000001776 ) ) ;
#10152 = VERTEX_POINT ( 'NONE', #38963 ) ;
#10153 = CARTESIAN_POINT ( 'NONE',  ( -28.21771817255893566, 0.2928912805552565390, -12.55734437234891132 ) ) ;
#10154 = CARTESIAN_POINT ( 'NONE',  ( -19.35675341420076023, -25.73740943626670585, -10.41501234953343946 ) ) ;
#10155 = ORIENTED_EDGE ( 'NONE', *, *, #30745, .T. ) ;
#10156 = CARTESIAN_POINT ( 'NONE',  ( 35.24432775889728475, -8.480040233932975013, -5.000000000000009770 ) ) ;
#10157 = ORIENTED_EDGE ( 'NONE', *, *, #4307, .T. ) ;
#10158 = PRODUCT_CONTEXT ( 'NONE', #26987, 'mechanical' ) ;
#10159 = CARTESIAN_POINT ( 'NONE',  ( -10.85362879025592342, 36.78189293023367412, 12.14047268033097282 ) ) ;
#10160 = LINE ( 'NONE', #7097, #11892 ) ;
#10161 = CARTESIAN_POINT ( 'NONE',  ( -4.360894802593465513, 8.147407145008980223, 7.102474990965859547 ) ) ;
#10162 = EDGE_CURVE ( 'NONE', #7910, #13732, #37938, .T. ) ;
#10163 = CARTESIAN_POINT ( 'NONE',  ( 11.57511119655671372, 28.64756621199167697, 18.87996532025786678 ) ) ;
#10164 = FACE_OUTER_BOUND ( 'NONE', #38501, .T. ) ;
#10165 = ORIENTED_EDGE ( 'NONE', *, *, #32101, .T. ) ;
#10166 = EDGE_CURVE ( 'NONE', #15787, #19280, #330, .T. ) ;
#10167 =( NAMED_UNIT ( * ) SI_UNIT ( $, .STERADIAN. ) SOLID_ANGLE_UNIT ( ) );
#10168 = CARTESIAN_POINT ( 'NONE',  ( 10.98647152928294446, 17.30743895948372213, -29.99999999999999289 ) ) ;
#10169 = CARTESIAN_POINT ( 'NONE',  ( 12.37161151015161842, 14.01709413980860219, 7.202682876670052359 ) ) ;
#10170 = DIRECTION ( 'NONE',  ( 0.000000000000000000, 0.000000000000000000, -1.000000000000000000 ) ) ;
#10171 = CARTESIAN_POINT ( 'NONE',  ( 16.91443829427942092, 17.27418336307699320, -14.80451719960429102 ) ) ;
#10172 = AXIS2_PLACEMENT_3D ( 'NONE', #36485, #15145, #36089 ) ;
#10173 = CARTESIAN_POINT ( 'NONE',  ( 6.063091157267137099, 20.95441350364335875, -24.44308551677271879 ) ) ;
#10174 = AXIS2_PLACEMENT_3D ( 'NONE', #34811, #6964, #28513 ) ;
#10175 = ORIENTED_EDGE ( 'NONE', *, *, #12408, .F. ) ;
#10176 = CARTESIAN_POINT ( 'NONE',  ( 11.03529696084846456, -19.42597325127027830, -22.66960005987283466 ) ) ;
#10177 = CARTESIAN_POINT ( 'NONE',  ( -5.440908595777636414, 35.94977745735568675, 7.000000000000000000 ) ) ;
#10178 = DIRECTION ( 'NONE',  ( 1.000000000000000000, 0.000000000000000000, 0.000000000000000000 ) ) ;
#10179 = ORIENTED_EDGE ( 'NONE', *, *, #12037, .F. ) ;
#10180 = CARTESIAN_POINT ( 'NONE',  ( -11.19888719761758722, 17.74582991396291831, -26.22643622722658563 ) ) ;
#10181 = CARTESIAN_POINT ( 'NONE',  ( -35.82891851945787209, -9.175709056024100363, 15.72805884748939498 ) ) ;
#10182 = CARTESIAN_POINT ( 'NONE',  ( 9.268250591559597851, -18.42220998856590697, -28.09379604205451741 ) ) ;
#10183 = DIRECTION ( 'NONE',  ( 0.000000000000000000, 0.000000000000000000, 1.000000000000000000 ) ) ;
#10184 = ORIENTED_EDGE ( 'NONE', *, *, #7842, .F. ) ;
#10185 = EDGE_LOOP ( 'NONE', ( #2026, #21465 ) ) ;
#10186 = CARTESIAN_POINT ( 'NONE',  ( -8.267738057345434655, 18.77097771606736032, -29.99999999999997868 ) ) ;
#10187 = DIRECTION ( 'NONE',  ( -1.000000000000000000, 0.000000000000000000, 0.000000000000000000 ) ) ;
#10188 = CARTESIAN_POINT ( 'NONE',  ( 14.44622163125243830, 19.97613264340516537, 10.49999999999999822 ) ) ;
#10189 = CARTESIAN_POINT ( 'NONE',  ( -34.15174964376215883, -8.447579901654981072, -8.931880151306236471 ) ) ;
#10190 = CARTESIAN_POINT ( 'NONE',  ( -13.41480434723648685, 15.78756373729235740, 7.392564007638123158 ) ) ;
#10191 = VERTEX_POINT ( 'NONE', #4834 ) ;
#10192 = CARTESIAN_POINT ( 'NONE',  ( 27.01856200969307054, 0.4099118485097461573, -14.48824044023039015 ) ) ;
#10193 = DIRECTION ( 'NONE',  ( 1.000000000000000000, 0.000000000000000000, 0.000000000000000000 ) ) ;
#10194 = DIRECTION ( 'NONE',  ( -0.000000000000000000, -0.000000000000000000, -1.000000000000000000 ) ) ;
#10195 = EDGE_LOOP ( 'NONE', ( #34104, #39769, #1296, #19566 ) ) ;
#10196 = CARTESIAN_POINT ( 'NONE',  ( -29.80962035732523674, 0.03519742696252582681, -9.709001665780544243 ) ) ;
#10197 = DIRECTION ( 'NONE',  ( 1.000000000000000000, 0.000000000000000000, 0.000000000000000000 ) ) ;
#10198 = VERTEX_POINT ( 'NONE', #5237 ) ;
#10199 = CARTESIAN_POINT ( 'NONE',  ( 31.72491548083144508, -2.179369429322845164, -9.120202422530157449 ) ) ;
#10200 = AXIS2_PLACEMENT_3D ( 'NONE', #36131, #14991, #27378 ) ;
#10201 = CARTESIAN_POINT ( 'NONE',  ( 19.79988521532547807, 5.489632757569235189, -30.00000000000001421 ) ) ;
#10202 = CARTESIAN_POINT ( 'NONE',  ( 17.09641143070718172, -27.64751350299042443, 15.72805884748858318 ) ) ;
#10203 = ORIENTED_EDGE ( 'NONE', *, *, #5548, .F. ) ;
#10204 = CARTESIAN_POINT ( 'NONE',  ( 14.97434053993231196, 30.45331253196302512, 15.13084544680209831 ) ) ;
#10205 = CARTESIAN_POINT ( 'NONE',  ( 37.48557158514988430, -11.25000000000009237, 3.000000000000000000 ) ) ;
#10206 = CARTESIAN_POINT ( 'NONE',  ( -5.469228652590086170, 26.20992143183283574, 20.94377226548378346 ) ) ;
#10207 = CIRCLE ( 'NONE', #1131, 6.000000000000005329 ) ;
#10208 = CYLINDRICAL_SURFACE ( 'NONE', #35611, 1.000000000000000000 ) ;
#10209 = CARTESIAN_POINT ( 'NONE',  ( -5.440836655099179353, 34.39106106163288246, 6.000000000000000000 ) ) ;
#10210 = FACE_BOUND ( 'NONE', #30267, .T. ) ;
#10211 = CARTESIAN_POINT ( 'NONE',  ( 28.14004025856615954, 4.421764093219024083, 14.53008259254450429 ) ) ;
#10212 = CARTESIAN_POINT ( 'NONE',  ( -22.92528781977826569, 9.871412332755808094, -6.451104567815622914 ) ) ;
#10213 = CARTESIAN_POINT ( 'NONE',  ( 14.50529647024089286, -17.03828888122068363, -23.33609894585849531 ) ) ;
#10214 = CARTESIAN_POINT ( 'NONE',  ( -22.57773860910944919, -27.07565175416711512, -4.999999999999999112 ) ) ;
#10215 = CARTESIAN_POINT ( 'NONE',  ( 10.93330143339572125, 17.49474783767401220, -28.07104482051876815 ) ) ;
#10216 = AXIS2_PLACEMENT_3D ( 'NONE', #31923, #35384, #4091 ) ;
#10217 = EDGE_LOOP ( 'NONE', ( #9330, #25774, #2520, #14074, #36247, #16003 ) ) ;
#10219 = VECTOR ( 'NONE', #29982, 1000.000000000000000 ) ;
#10218 = CARTESIAN_POINT ( 'NONE',  ( -14.60464479478044808, 23.69115059860245864, -12.58079236048715188 ) ) ;
#10220 = CARTESIAN_POINT ( 'NONE',  ( -27.45400382858790067, -18.53605996571844727, 19.99202127657103745 ) ) ;
#10221 = DIRECTION ( 'NONE',  ( 1.000000000000000000, 0.000000000000000000, 0.000000000000000000 ) ) ;
#10222 = CARTESIAN_POINT ( 'NONE',  ( 15.25363860433223806, 26.33374284506462715, -7.828164261976985117 ) ) ;
#10223 = EDGE_LOOP ( 'NONE', ( #11765, #10470, #25039 ) ) ;
#10224 = CARTESIAN_POINT ( 'NONE',  ( 20.31494021939268535, -10.42483993722323454, -22.98956373470440440 ) ) ;
#10225 = CARTESIAN_POINT ( 'NONE',  ( 8.293999462566144842, 11.53598992149257008, 6.000000000000000000 ) ) ;
#10226 = VERTEX_POINT ( 'NONE', #38558 ) ;
#10228 = CARTESIAN_POINT ( 'NONE',  ( 0.4999999999999990563, 31.00000000000000355, 9.000000000000001776 ) ) ;
#10227 = CARTESIAN_POINT ( 'NONE',  ( -14.65523368257949066, 26.15792607398499570, -10.14769008996043986 ) ) ;
#10229 = CARTESIAN_POINT ( 'NONE',  ( -15.03157439599174694, -25.19314163198803769, -11.55082534625164037 ) ) ;
#10230 = LINE ( 'NONE', #6571, #18598 ) ;
#10231 = TOROIDAL_SURFACE ( 'NONE', #32962, 1.000000000000000000, 0.5000000000000000000 ) ;
#10232 = ORIENTED_EDGE ( 'NONE', *, *, #39941, .F. ) ;
#10233 = CARTESIAN_POINT ( 'NONE',  ( -31.52559900738557985, -12.98691925735731978, -11.99846548842175586 ) ) ;
#10234 = CARTESIAN_POINT ( 'NONE',  ( -12.90570201017717267, -24.02570373875013843, -13.54976151863601785 ) ) ;
#10235 = DIRECTION ( 'NONE',  ( -0.9510565162951543083, -0.3090169943749450088, 0.000000000000000000 ) ) ;
#10236 = CARTESIAN_POINT ( 'NONE',  ( 14.11158459539261401, 18.94724806458638255, -18.68180965987205866 ) ) ;
#10237 = EDGE_LOOP ( 'NONE', ( #1097, #34185, #31821, #6536 ) ) ;
#10238 = CARTESIAN_POINT ( 'NONE',  ( 20.01208193039519756, 4.507116686654150328, -29.40064677792853232 ) ) ;
#10239 = ADVANCED_FACE ( 'NONE', ( #7679 ), #26289, .T. ) ;
#10240 = CARTESIAN_POINT ( 'NONE',  ( 3.610593701936713806, 31.83882289796390097, 10.49999999999999645 ) ) ;
#10241 = CARTESIAN_POINT ( 'NONE',  ( 0.9819609608163288872, 14.62372257652092422, 6.000000000000000000 ) ) ;
#10242 = ORIENTED_EDGE ( 'NONE', *, *, #20795, .F. ) ;
#10243 = CARTESIAN_POINT ( 'NONE',  ( -30.98040994848943086, -0.4068539715029224624, -7.344088399820972057 ) ) ;
#10244 = CARTESIAN_POINT ( 'NONE',  ( 30.98810501497172964, -0.5565724573307553324, -7.804721584860615735 ) ) ;
#10245 = ADVANCED_FACE ( 'NONE', ( #1793 ), #14176, .F. ) ;
#10246 = CARTESIAN_POINT ( 'NONE',  ( 27.10945576260617429, -19.90266412673917529, 19.66345542862529783 ) ) ;
#10247 = VERTEX_POINT ( 'NONE', #30022 ) ;
#10248 = ADVANCED_FACE ( 'NONE', ( #32267 ), #39361, .F. ) ;
#10249 = AXIS2_PLACEMENT_3D ( 'NONE', #7314, #35768, #32528 ) ;
#10250 = CARTESIAN_POINT ( 'NONE',  ( 17.81784622497951176, -13.85677843414110555, -30.00000000000001421 ) ) ;
#10251 = DIRECTION ( 'NONE',  ( -0.9135454576426059736, -0.4067366430757888285, 0.000000000000000000 ) ) ;
#10252 = TOROIDAL_SURFACE ( 'NONE', #30400, 1.000000000000000000, 0.5000000000000000000 ) ;
#10253 = CARTESIAN_POINT ( 'NONE',  ( -14.26584774442725845, 27.13525491562436542, 7.000000000000000000 ) ) ;
#10254 = VECTOR ( 'NONE', #29747, 999.9999999999998863 ) ;
#10255 = AXIS2_PLACEMENT_3D ( 'NONE', #24780, #12789, #18695 ) ;
#10256 = CARTESIAN_POINT ( 'NONE',  ( -11.36213480545077736, 32.05769576588223657, 10.87262190629438408 ) ) ;
#10257 = DIRECTION ( 'NONE',  ( 1.000000000000000000, 0.000000000000000000, 0.000000000000000000 ) ) ;
#10258 = DIRECTION ( 'NONE',  ( 0.9510565162951543083, 0.3090169943749450088, 0.000000000000000000 ) ) ;
#10259 = VERTEX_POINT ( 'NONE', #29416 ) ;
#10260 = EDGE_CURVE ( 'NONE', #24757, #27796, #30182, .T. ) ;
#10261 = CARTESIAN_POINT ( 'NONE',  ( 12.39463915635820612, 18.33192650902018883, 6.000000000000000000 ) ) ;
#10262 = ADVANCED_FACE ( 'NONE', ( #13771 ), #7471, .T. ) ;
#10263 = CARTESIAN_POINT ( 'NONE',  ( 3.666817917346630207, 8.455467583238284845, 10.83333333333332860 ) ) ;
#10264 = CARTESIAN_POINT ( 'NONE',  ( 23.83838753405464317, -22.06766206393824703, -12.96906389866784259 ) ) ;
#10265 = DIRECTION ( 'NONE',  ( -1.000000000000000000, 0.000000000000000000, 0.000000000000000000 ) ) ;
#10266 = LINE ( 'NONE', #13509, #22900 ) ;
#10267 = CARTESIAN_POINT ( 'NONE',  ( 14.07479620741808191, 25.02281174304687639, -12.50432048929940976 ) ) ;
#10268 = CARTESIAN_POINT ( 'NONE',  ( -1.828660225306043108, 9.087095699275881344, 9.500000000000000000 ) ) ;
#10269 = ORIENTED_EDGE ( 'NONE', *, *, #32149, .F. ) ;
#10271 = CARTESIAN_POINT ( 'NONE',  ( 0.000000000000000000, 22.50000000000000355, 6.000000000000000000 ) ) ;
#10270 = CARTESIAN_POINT ( 'NONE',  ( -16.58243014776942204, 17.87902810744316184, -14.77884403044956763 ) ) ;
#10272 = DIRECTION ( 'NONE',  ( 0.000000000000000000, -0.000000000000000000, -1.000000000000000000 ) ) ;
#10273 = CARTESIAN_POINT ( 'NONE',  ( 14.94392118707002126, -25.98235010733188588, -9.238761082775399203 ) ) ;
#10274 = CARTESIAN_POINT ( 'NONE',  ( 7.824485034907088021, 10.87986945260446170, 7.499999999999999112 ) ) ;
#10275 = CARTESIAN_POINT ( 'NONE',  ( 12.93407688617792495, 21.64341771708264517, -17.43892928429220035 ) ) ;
#10276 = ORIENTED_EDGE ( 'NONE', *, *, #4738, .F. ) ;
#10277 = CARTESIAN_POINT ( 'NONE',  ( 15.01557101168928909, 25.97699093630907541, -9.238213213168704030 ) ) ;
#10278 = EDGE_LOOP ( 'NONE', ( #26952, #32956, #21131, #9286 ) ) ;
#10280 = DIRECTION ( 'NONE',  ( 0.000000000000000000, 0.000000000000000000, 1.000000000000000000 ) ) ;
#10279 = CARTESIAN_POINT ( 'NONE',  ( -14.50572258746885623, 25.04706427101906741, -11.59331239428562021 ) ) ;
#10281 = CARTESIAN_POINT ( 'NONE',  ( -15.03457768504921610, -26.13549839691439658, -8.768128526806304279 ) ) ;
#10282 = CARTESIAN_POINT ( 'NONE',  ( -28.08361064019272391, -26.79812557672154938, 13.32518128616592001 ) ) ;
#10283 = VECTOR ( 'NONE', #19661, 1000.000000000000114 ) ;
#10284 = CARTESIAN_POINT ( 'NONE',  ( -20.67042552518347875, -15.19177032836172003, -19.66260926008852650 ) ) ;
#10285 = CARTESIAN_POINT ( 'NONE',  ( -2.438111228425578592, -23.95987689082008743, -11.87913270965556123 ) ) ;
#10286 = CARTESIAN_POINT ( 'NONE',  ( 11.33961468246317139, 17.07831742606941461, -30.00000000000000000 ) ) ;
#10287 = ORIENTED_EDGE ( 'NONE', *, *, #14868, .T. ) ;
#10288 = CARTESIAN_POINT ( 'NONE',  ( 23.89591241149270218, 8.281799400457325433, -7.415685632315970999 ) ) ;
#10289 = CARTESIAN_POINT ( 'NONE',  ( 32.65693615964542573, -20.41475057477927280, -4.999999999999999112 ) ) ;
#10290 = CARTESIAN_POINT ( 'NONE',  ( 2.518583951651052644, 7.712953814960687104, 7.000000000000000000 ) ) ;
#10291 = CARTESIAN_POINT ( 'NONE',  ( -4.783493507398182132, 36.70021839994218027, 17.42190598798394063 ) ) ;
#10292 = CIRCLE ( 'NONE', #26503, 1.000000000000000888 ) ;
#10293 = ORIENTED_EDGE ( 'NONE', *, *, #712, .T. ) ;
#10294 = CARTESIAN_POINT ( 'NONE',  ( -24.11176595098584841, -2.272178682370984415, -20.18870583158593490 ) ) ;
#10295 = EDGE_CURVE ( 'NONE', #5543, #5069, #13976, .T. ) ;
#10296 = VECTOR ( 'NONE', #27345, 1000.000000000000114 ) ;
#10297 = CARTESIAN_POINT ( 'NONE',  ( -29.28423149095161904, -1.632116715639065241, 18.42518152272108978 ) ) ;
#10298 = VERTEX_POINT ( 'NONE', #38760 ) ;
#10299 = CARTESIAN_POINT ( 'NONE',  ( 23.19735768193471870, -14.64350930037810095, 20.99999999999999645 ) ) ;
#10300 = CARTESIAN_POINT ( 'NONE',  ( -13.30736791469135483, 15.68301270237671474, 10.49999999999999822 ) ) ;
#10301 = CARTESIAN_POINT ( 'NONE',  ( 23.73065287294122783, -9.570089218292375577, -19.68554350756277671 ) ) ;
#10302 = CARTESIAN_POINT ( 'NONE',  ( 16.87498849720631711, -29.16588574430777925, 11.55979286843775000 ) ) ;
#10303 = ORIENTED_EDGE ( 'NONE', *, *, #34779, .F. ) ;
#10304 = EDGE_LOOP ( 'NONE', ( #12126, #9349, #3081, #28928 ) ) ;
#10305 = DIRECTION ( 'NONE',  ( -0.1045284632676569680, -0.9945218953682730678, 0.000000000000000000 ) ) ;
#10306 = CARTESIAN_POINT ( 'NONE',  ( -12.14717575287011719, 32.53695909538323860, 6.000000000000000000 ) ) ;
#10307 = VECTOR ( 'NONE', #6666, 999.9999999999998863 ) ;
#10308 = AXIS2_PLACEMENT_3D ( 'NONE', #14774, #21459, #2184 ) ;
#10309 = CARTESIAN_POINT ( 'NONE',  ( 18.00000000000000000, 22.50000000000000711, 13.00000000000000178 ) ) ;
#10310 = ORIENTED_EDGE ( 'NONE', *, *, #7349, .F. ) ;
#10311 = CARTESIAN_POINT ( 'NONE',  ( -1.918774233022853437, 38.27677537973431043, -6.276859307182877323 ) ) ;
#10312 = DIRECTION ( 'NONE',  ( -0.2876062384759508483, 0.6459741880212531706, -0.7071067811865455743 ) ) ;
#10313 = FACE_OUTER_BOUND ( 'NONE', #28838, .T. ) ;
#10314 = EDGE_CURVE ( 'NONE', #29868, #39481, #13956, .T. ) ;
#10315 = VECTOR ( 'NONE', #15057, 1000.000000000000114 ) ;
#10316 = CARTESIAN_POINT ( 'NONE',  ( -11.11016527260153808, 31.83082137946488643, 7.000000000000000000 ) ) ;
#10317 = LINE ( 'NONE', #13154, #37243 ) ;
#10318 = DIRECTION ( 'NONE',  ( 1.000000000000000000, 0.000000000000000000, 0.000000000000000000 ) ) ;
#10319 = CARTESIAN_POINT ( 'NONE',  ( 10.10147183288163220, 20.27820810593225076, -22.48066845728959251 ) ) ;
#10320 = CARTESIAN_POINT ( 'NONE',  ( 16.00000000000000000, 22.50000000000000711, 6.000000000000000000 ) ) ;
#10321 = VERTEX_POINT ( 'NONE', #32882 ) ;
#10323 = DIRECTION ( 'NONE',  ( -0.9781476007338041345, 0.2079116908177664202, 0.000000000000000000 ) ) ;
#10322 = CARTESIAN_POINT ( 'NONE',  ( -16.91065988350933935, 11.83293620019187919, -27.16773465279506894 ) ) ;
#10324 = DIRECTION ( 'NONE',  ( 0.000000000000000000, 0.000000000000000000, 1.000000000000000000 ) ) ;
#10325 = CARTESIAN_POINT ( 'NONE',  ( 9.596601641187952225, -18.16644679415211172, -28.70396621286603533 ) ) ;
#10326 = CARTESIAN_POINT ( 'NONE',  ( 2.317734025672765430, 9.191051544684729180, 10.00000000000000000 ) ) ;
#10327 = B_SPLINE_CURVE_WITH_KNOTS ( 'NONE', 3,
 ( #7666, #22696, #7863, #20069, #14163, #13962 ),
 .UNSPECIFIED., .F., .F.,
 ( 4, 2, 4 ),
 ( 0.000000000000000000, 0.5000000000000000000, 1.000000000000000000 ),
 .UNSPECIFIED. ) ;
#10328 = CARTESIAN_POINT ( 'NONE',  ( 15.08754104065838497, 26.18438373079535708, -8.765583629728475046 ) ) ;
#10329 = CARTESIAN_POINT ( 'NONE',  ( -22.45323650136969462, -2.382502413133420038, -30.00000000000000000 ) ) ;
#10330 = CARTESIAN_POINT ( 'NONE',  ( -12.37435565298220119, 15.93301270189233598, 7.499999999999993783 ) ) ;
#10331 = CARTESIAN_POINT ( 'NONE',  ( -19.21792407943181757, -19.17370927486487275, -17.77733382730791334 ) ) ;
#10332 = CARTESIAN_POINT ( 'NONE',  ( 5.642336087577458414, -23.56041604079663898, -13.82695612366311266 ) ) ;
#10333 = CARTESIAN_POINT ( 'NONE',  ( 11.58115104542198637, 18.35365690391862614, -23.86862541693199802 ) ) ;
#10334 = CARTESIAN_POINT ( 'NONE',  ( 30.18028009888747221, -21.81123660786073870, -8.413970242988657589 ) ) ;
#10335 = DIRECTION ( 'NONE',  ( 0.000000000000000000, 0.000000000000000000, 1.000000000000000000 ) ) ;
#10336 = CARTESIAN_POINT ( 'NONE',  ( -37.50916529491303919, -2.485117785107662680, 11.00000000000000000 ) ) ;
#10337 = VERTEX_POINT ( 'NONE', #35723 ) ;
#10338 = CARTESIAN_POINT ( 'NONE',  ( -5.356379776258165748, 22.86463390630803261, -22.00052314567535561 ) ) ;
#10339 = ORIENTED_EDGE ( 'NONE', *, *, #25010, .F. ) ;
#10340 = EDGE_CURVE ( 'NONE', #4096, #36923, #17445, .T. ) ;
#10341 = CIRCLE ( 'NONE', #33067, 1.000000000000000000 ) ;
#10342 = CARTESIAN_POINT ( 'NONE',  ( 14.47283171447378969, 21.48159823030311344, 10.99999999999999289 ) ) ;
#10343 = ORIENTED_EDGE ( 'NONE', *, *, #7448, .T. ) ;
#10344 = CARTESIAN_POINT ( 'NONE',  ( 20.97320688508112596, 0.7727878754155812491, -26.22179187276591961 ) ) ;
#10345 = EDGE_CURVE ( 'NONE', #34172, #18383, #2279, .T. ) ;
#10346 = CARTESIAN_POINT ( 'NONE',  ( 9.160254037844365982, 18.36602540378440196, 10.49999999999999822 ) ) ;
#10347 = EDGE_CURVE ( 'NONE', #21571, #31788, #25604, .T. ) ;
#10348 = CARTESIAN_POINT ( 'NONE',  ( -8.633502029282189127, 11.46765470489704164, 9.500000000000000000 ) ) ;
#10349 = AXIS2_PLACEMENT_3D ( 'NONE', #9568, #37788, #9961 ) ;
#10350 = B_SPLINE_SURFACE_WITH_KNOTS ( 'NONE', 1, 3, ( 
 ( #13119, #10082, #25715, #26324, #25508, #34869, #7019, #10687, #25914, #20035 ),
 ( #7423, #29369, #16788, #1341, #38109, #1546, #22663, #35066, #38718, #16585 ) ),
 .UNSPECIFIED., .F., .F., .F.,
 ( 2, 2 ),
 ( 4, 2, 2, 2, 4 ),
 ( 0.000000000000000000, 1.000000000000000000 ),
 ( 1.344962617103288904, 1.737661698802012822, 2.130360780500736961, 2.523059862199461101, 2.915758943898185240 ),
 .UNSPECIFIED. ) ;
#10351 = ORIENTED_EDGE ( 'NONE', *, *, #10476, .F. ) ;
#10352 = CARTESIAN_POINT ( 'NONE',  ( -27.07907469388687716, 0.3230542143888946449, -14.48244227824745245 ) ) ;
#10353 = CARTESIAN_POINT ( 'NONE',  ( -2.256323172317921788, 14.28970123917155277, 7.000000000000000000 ) ) ;
#10354 = ORIENTED_EDGE ( 'NONE', *, *, #34499, .T. ) ;
#10355 = CARTESIAN_POINT ( 'NONE',  ( 31.01063626114513738, -8.317636515201035863, -13.00212388364185223 ) ) ;
#10356 = EDGE_CURVE ( 'NONE', #25471, #20190, #15238, .T. ) ;
#10357 = VERTEX_POINT ( 'NONE', #2787 ) ;
#10358 = CARTESIAN_POINT ( 'NONE',  ( -14.84499459426757184, 32.56974970312059270, 12.14047268033097282 ) ) ;
#10359 = DIRECTION ( 'NONE',  ( -0.000000000000000000, -0.000000000000000000, -1.000000000000000000 ) ) ;
#10360 = PLANE ( 'NONE',  #36442 ) ;
#10361 = CARTESIAN_POINT ( 'NONE',  ( 6.977707682420476232, 31.68171018602294708, 19.66345542862528006 ) ) ;
#10362 = FACE_OUTER_BOUND ( 'NONE', #8191, .T. ) ;
#10363 = ORIENTED_EDGE ( 'NONE', *, *, #37200, .F. ) ;
#10364 = CARTESIAN_POINT ( 'NONE',  ( -2.256323172317922232, 14.28970123917155277, 7.000000000000000000 ) ) ;
#10365 = DIRECTION ( 'NONE',  ( 1.000000000000000000, 0.000000000000000000, 0.000000000000000000 ) ) ;
#10366 = EDGE_CURVE ( 'NONE', #10384, #38528, #26790, .T. ) ;
#10367 = ADVANCED_FACE ( 'NONE', ( #33686 ), #21669, .T. ) ;
#10368 = CARTESIAN_POINT ( 'NONE',  ( -9.183247089818959097, 16.78440424842446532, 6.000000000000000000 ) ) ;
#10369 = EDGE_CURVE ( 'NONE', #37600, #10337, #5439, .T. ) ;
#10370 = CARTESIAN_POINT ( 'NONE',  ( 13.82201771817531544, 15.33810796475532356, -27.62586602732605101 ) ) ;
#10372 = VECTOR ( 'NONE', #9424, 1000.000000000000000 ) ;
#10371 = CARTESIAN_POINT ( 'NONE',  ( 8.507170864035593638, 26.45108214636019639, -16.86777324031742253 ) ) ;
#10373 = ORIENTED_EDGE ( 'NONE', *, *, #29443, .T. ) ;
#10374 = CARTESIAN_POINT ( 'NONE',  ( -4.724378136954611840, 12.76962061027129458, 6.000000000000000000 ) ) ;
#10375 = CARTESIAN_POINT ( 'NONE',  ( 10.44103466624280507, 32.57396620494213124, 7.000000000000000000 ) ) ;
#10376 = CARTESIAN_POINT ( 'NONE',  ( 16.02147964071269115, -26.56717389092953852, -7.803345548162054612 ) ) ;
#10377 = CARTESIAN_POINT ( 'NONE',  ( 15.37000524124839274, -27.20210912714562212, 15.72805884748939498 ) ) ;
#10378 = LINE ( 'NONE', #23374, #5062 ) ;
#10379 = ORIENTED_EDGE ( 'NONE', *, *, #13164, .T. ) ;
#10380 = CARTESIAN_POINT ( 'NONE',  ( -13.77848933305083712, 23.37701899211078072, -14.47715019980521411 ) ) ;
#10381 = CARTESIAN_POINT ( 'NONE',  ( -17.16434664248912512, -27.18154623538578107, 16.30093088680177615 ) ) ;
#10382 = CARTESIAN_POINT ( 'NONE',  ( 13.20637083253811461, -24.05908822848580897, -13.53613500056979291 ) ) ;
#10383 = LINE ( 'NONE', #31314, #7518 ) ;
#10384 = VERTEX_POINT ( 'NONE', #21080 ) ;
#10385 = ORIENTED_EDGE ( 'NONE', *, *, #31204, .F. ) ;
#10386 = CARTESIAN_POINT ( 'NONE',  ( -8.874894838237054273, 18.54570556417430538, -28.62091128729561973 ) ) ;
#10387 = DIRECTION ( 'NONE',  ( 1.000000000000000000, 0.000000000000000000, 0.000000000000000000 ) ) ;
#10388 = EDGE_CURVE ( 'NONE', #19790, #28635, #36008, .T. ) ;
#10389 = DIRECTION ( 'NONE',  ( 1.000000000000000000, 0.000000000000000000, 0.000000000000000000 ) ) ;
#10390 = EDGE_CURVE ( 'NONE', #37016, #2411, #3571, .T. ) ;
#10391 = CARTESIAN_POINT ( 'NONE',  ( -33.05153516003798586, -7.169066213692435241, -10.30292366904723700 ) ) ;
#10392 = CARTESIAN_POINT ( 'NONE',  ( 11.81630298851978900, 31.79381426990546089, 10.49999999999999822 ) ) ;
#10393 = ORIENTED_EDGE ( 'NONE', *, *, #29147, .T. ) ;
#10394 = CARTESIAN_POINT ( 'NONE',  ( 30.81169820973430973, 0.05224243800113868852, -5.474171594225969883 ) ) ;
#10395 = ADVANCED_FACE ( 'NONE', ( #24519 ), #36922, .F. ) ;
#10396 = CARTESIAN_POINT ( 'NONE',  ( 2.672146553953313131, 12.33340603770390764, 10.50000000000000000 ) ) ;
#10397 = DIRECTION ( 'NONE',  ( 1.000000000000000000, 0.000000000000000000, 0.000000000000000000 ) ) ;
#10398 = VERTEX_POINT ( 'NONE', #28668 ) ;
#10399 = CARTESIAN_POINT ( 'NONE',  ( -20.52752421040557351, 0.8457101814844484311, -28.70654326211919027 ) ) ;
#10400 = B_SPLINE_CURVE_WITH_KNOTS ( 'NONE', 3,
 ( #29950, #13910, #32610, #36260, #10666, #8422 ),
 .UNSPECIFIED., .F., .F.,
 ( 4, 2, 4 ),
 ( 0.000000000000000000, 0.5000000000000000000, 1.000000000000000000 ),
 .UNSPECIFIED. ) ;
#10401 = DIRECTION ( 'NONE',  ( -1.000000000000000000, 0.000000000000000000, 0.000000000000000000 ) ) ;
#10402 = ORIENTED_EDGE ( 'NONE', *, *, #27524, .F. ) ;
#10403 = CARTESIAN_POINT ( 'NONE',  ( 20.47947323059178260, -0.9304062671392134831, -30.00000000000000000 ) ) ;
#10404 = ADVANCED_FACE ( 'NONE', ( #29071 ), #13024, .F. ) ;
#10405 = CARTESIAN_POINT ( 'NONE',  ( 18.58489934068024141, 8.677531291371142430, -30.00000000000000355 ) ) ;
#10406 = CARTESIAN_POINT ( 'NONE',  ( 34.21349446592028443, -17.75307084757209353, 16.30093088680191826 ) ) ;
#10407 = EDGE_LOOP ( 'NONE', ( #25265, #39680, #30251, #9941 ) ) ;
#10408 = CARTESIAN_POINT ( 'NONE',  ( -1.359097634403079240E-13, 39.35700678546972853, 15.13084544680213739 ) ) ;
#10409 = CARTESIAN_POINT ( 'NONE',  ( -2.036571916123810055, 8.108948098542073879, 7.000000000000000000 ) ) ;
#10410 = CARTESIAN_POINT ( 'NONE',  ( 2.109751222703333706, 28.76298082888545338, 20.94377226548378346 ) ) ;
#10411 = CARTESIAN_POINT ( 'NONE',  ( 1.000000000000000000, 37.00000000000000711, 11.00000000000000000 ) ) ;
#10412 = CARTESIAN_POINT ( 'NONE',  ( 0.000000000000000000, 22.50000000000000355, 7.000000000000000000 ) ) ;
#10413 = EDGE_CURVE ( 'NONE', #25213, #19790, #37813, .T. ) ;
#10414 = FACE_BOUND ( 'NONE', #11853, .T. ) ;
#10415 = CARTESIAN_POINT ( 'NONE',  ( 18.42861860568664056, 16.71074749267215154, 16.87380292611454280 ) ) ;
#10416 = CIRCLE ( 'NONE', #35075, 1.000000000000000000 ) ;
#10417 = CARTESIAN_POINT ( 'NONE',  ( -20.06104095114847041, 7.248907926436412019, -23.26760403684622602 ) ) ;
#10418 = CARTESIAN_POINT ( 'NONE',  ( 21.07929656120333917, -26.04002531597158310, -9.455788634464944664 ) ) ;
#10419 = CARTESIAN_POINT ( 'NONE',  ( -4.524139159579186220, 31.43208625488817276, 10.50000000000000000 ) ) ;
#10420 = VERTEX_POINT ( 'NONE', #31522 ) ;
#10421 = CARTESIAN_POINT ( 'NONE',  ( 12.01797261908369840, 20.05841915129454733, -20.51811533202489102 ) ) ;
#10422 = ORIENTED_EDGE ( 'NONE', *, *, #2271, .F. ) ;
#10423 = CARTESIAN_POINT ( 'NONE',  ( -15.74234945116950790, 25.02555085579499305, -7.363867029611805393 ) ) ;
#10424 = CARTESIAN_POINT ( 'NONE',  ( -20.26242815737374769, -21.95648885305439180, 19.99202127657103389 ) ) ;
#10425 = FACE_OUTER_BOUND ( 'NONE', #17393, .T. ) ;
#10426 = CARTESIAN_POINT ( 'NONE',  ( 14.86957149986643145, 25.52042674580396309, -10.18200345931521866 ) ) ;
#10427 = ORIENTED_EDGE ( 'NONE', *, *, #4068, .T. ) ;
#10428 = CARTESIAN_POINT ( 'NONE',  ( 33.57338286677032357, -18.51555322403216053, -6.276315919122906983 ) ) ;
#10429 = DIRECTION ( 'NONE',  ( 0.4999999999999920064, -0.8660254037844432595, 0.000000000000000000 ) ) ;
#10430 = VECTOR ( 'NONE', #21556, 999.9999999999998863 ) ;
#10431 = ORIENTED_EDGE ( 'NONE', *, *, #28150, .T. ) ;
#10433 = DIRECTION ( 'NONE',  ( 1.000000000000000000, 0.000000000000000000, 0.000000000000000000 ) ) ;
#10432 = CARTESIAN_POINT ( 'NONE',  ( -10.88717731418932289, 17.62612854685823649, -27.43333487934502557 ) ) ;
#10434 = CARTESIAN_POINT ( 'NONE',  ( -15.89382728895068553, -26.44918619828455775, -8.270623719106945160 ) ) ;
#10435 = DIRECTION ( 'NONE',  ( -0.000000000000000000, -0.000000000000000000, -1.000000000000000000 ) ) ;
#10436 = ORIENTED_EDGE ( 'NONE', *, *, #306, .T. ) ;
#10437 = CARTESIAN_POINT ( 'NONE',  ( -33.03998026049733028, -13.61677984810819275, -10.19367267226056484 ) ) ;
#10438 = CARTESIAN_POINT ( 'NONE',  ( -9.521033199116716972, -19.40341469932255691, -23.93640817374758711 ) ) ;
#10439 = CARTESIAN_POINT ( 'NONE',  ( -21.55328011382844977, 16.02264588471131646, 11.00000000000000000 ) ) ;
#10440 = CARTESIAN_POINT ( 'NONE',  ( 15.98076197519813668, 18.99300102774612498, -14.72676035881280043 ) ) ;
#10441 = EDGE_LOOP ( 'NONE', ( #18860, #26067 ) ) ;
#10442 = CARTESIAN_POINT ( 'NONE',  ( 26.35545874991313653, 3.770332275510887232, -10.75732149805491034 ) ) ;
#10443 = EDGE_CURVE ( 'NONE', #14016, #34496, #22767, .T. ) ;
#10444 = CARTESIAN_POINT ( 'NONE',  ( 0.5000000000000001110, 37.00000000000000711, 7.000000000000000000 ) ) ;
#10445 = LINE ( 'NONE', #13896, #2433 ) ;
#10446 = ORIENTED_EDGE ( 'NONE', *, *, #23335, .F. ) ;
#10447 = CARTESIAN_POINT ( 'NONE',  ( -21.74228451847596588, 0.5523326501866797633, -23.83255557727324714 ) ) ;
#10448 = CARTESIAN_POINT ( 'NONE',  ( 31.38436285448675989, -0.5902540978377334158, -5.938636948564323781 ) ) ;
#10449 = VECTOR ( 'NONE', #21158, 1000.000000000000000 ) ;
#10450 = CARTESIAN_POINT ( 'NONE',  ( 30.13477841296669979, -9.898407001805262340, 19.99202127657102679 ) ) ;
#10451 = AXIS2_PLACEMENT_3D ( 'NONE', #23999, #33762, #18310 ) ;
#10452 = ORIENTED_EDGE ( 'NONE', *, *, #4938, .F. ) ;
#10453 = CARTESIAN_POINT ( 'NONE',  ( 6.023418944065099367, 39.81932404830325112, -4.999999999999995559 ) ) ;
#10454 = DIRECTION ( 'NONE',  ( 0.000000000000000000, 0.000000000000000000, 1.000000000000000000 ) ) ;
#10455 = DIRECTION ( 'NONE',  ( -0.000000000000000000, -0.000000000000000000, 1.000000000000000000 ) ) ;
#10456 = AXIS2_PLACEMENT_3D ( 'NONE', #9122, #2826, #12565 ) ;
#10457 = DIRECTION ( 'NONE',  ( -0.6123724356957971349, 0.3535533905932787824, -0.7071067811865427988 ) ) ;
#10458 = CARTESIAN_POINT ( 'NONE',  ( -37.48557158514991272, -11.24999999999982414, 2.999999999999999112 ) ) ;
#10459 = FACE_OUTER_BOUND ( 'NONE', #23869, .T. ) ;
#10460 = CARTESIAN_POINT ( 'NONE',  ( 2.229431105722923245, 20.49260818092372460, 6.000000000000000000 ) ) ;
#10461 = ADVANCED_FACE ( 'NONE', ( #19525 ), #29277, .F. ) ;
#10462 = ORIENTED_EDGE ( 'NONE', *, *, #39478, .F. ) ;
#10463 = CARTESIAN_POINT ( 'NONE',  ( -6.832768599200551130, 35.70122713809554682, 10.49999999999999822 ) ) ;
#10464 = DIRECTION ( 'NONE',  ( 0.3090169943749573322, 0.9510565162951504226, 0.000000000000000000 ) ) ;
#10465 = CARTESIAN_POINT ( 'NONE',  ( 28.23631333451608683, -24.52731714411232744, -6.292009388830251737 ) ) ;
#10466 = CARTESIAN_POINT ( 'NONE',  ( 14.86556419889027048, 20.43481210330100595, 10.63089969389956835 ) ) ;
#10467 = CARTESIAN_POINT ( 'NONE',  ( 9.343266739736582949, 17.68301270189217433, 11.00000000000000000 ) ) ;
#10468 = CARTESIAN_POINT ( 'NONE',  ( 15.18041152575273500, 27.55477496851653640, -5.000000000000000000 ) ) ;
#10469 = FILL_AREA_STYLE_COLOUR ( '', #7436 ) ;
#10470 = ORIENTED_EDGE ( 'NONE', *, *, #3640, .T. ) ;
#10471 = AXIS2_PLACEMENT_3D ( 'NONE', #380, #31647, #24751 ) ;
#10472 = CARTESIAN_POINT ( 'NONE',  ( -17.83076603928403969, 19.73132804355285685, -5.477525253067689448 ) ) ;
#10473 = FACE_OUTER_BOUND ( 'NONE', #2903, .T. ) ;
#10474 = VECTOR ( 'NONE', #5265, 1000.000000000000114 ) ;
#10475 = CARTESIAN_POINT ( 'NONE',  ( 13.36832410447146380, -23.62212012520782523, -14.47646263800011113 ) ) ;
#10476 = EDGE_CURVE ( 'NONE', #5055, #36861, #9984, .T. ) ;
#10477 = DIRECTION ( 'NONE',  ( 0.6445931928399328825, 0.000000000000000000, -0.7645257456387070105 ) ) ;
#10478 = CARTESIAN_POINT ( 'NONE',  ( 11.05197910185074583, 17.41712326167257885, -28.07812360280739838 ) ) ;
#10479 = EDGE_LOOP ( 'NONE', ( #21474, #33482, #19231 ) ) ;
#10480 = CARTESIAN_POINT ( 'NONE',  ( 14.93249212465000397, 25.80697923307498698, -9.708869224783416740 ) ) ;
#10481 = ORIENTED_EDGE ( 'NONE', *, *, #8665, .F. ) ;
#10483 = DIRECTION ( 'NONE',  ( 0.3090169943749450643, -0.9510565162951544194, 0.000000000000000000 ) ) ;
#10482 = CARTESIAN_POINT ( 'NONE',  ( -10.97676730033676407, 17.36694328198177573, -28.70573505724077989 ) ) ;
#10484 = CARTESIAN_POINT ( 'NONE',  ( -15.12588299545583403, -26.27105592520571520, -8.298080420248476585 ) ) ;
#10485 = CARTESIAN_POINT ( 'NONE',  ( -36.42486030274168485, -16.61012894281843444, 13.32518128616628950 ) ) ;
#10486 = CARTESIAN_POINT ( 'NONE',  ( -16.96436027188408602, -11.67839957979620280, -28.44978934027107087 ) ) ;
#10487 = CARTESIAN_POINT ( 'NONE',  ( -3.323560782785250911, -20.43354657522463214, -27.15214811866635358 ) ) ;
#10488 = CARTESIAN_POINT ( 'NONE',  ( 15.30101822393199029, 24.69709018996960737, -9.726406352004691058 ) ) ;
#10489 = ORIENTED_EDGE ( 'NONE', *, *, #30406, .F. ) ;
#10490 = CARTESIAN_POINT ( 'NONE',  ( 19.25042232574495671, 7.324643854277566923, -27.70922511033380076 ) ) ;
#10491 = DIRECTION ( 'NONE',  ( 1.000000000000000000, 0.000000000000000000, 0.000000000000000000 ) ) ;
#10492 = AXIS2_PLACEMENT_3D ( 'NONE', #20295, #38777, #17256 ) ;
#10493 = CARTESIAN_POINT ( 'NONE',  ( 1.590043107810628076, 12.61456814725305442, 10.50000000000000000 ) ) ;
#10494 = CARTESIAN_POINT ( 'NONE',  ( 1.553811836244721745, 36.85721162268941242, 17.92354375535250810 ) ) ;
#10495 = VERTEX_POINT ( 'NONE', #3684 ) ;
#10496 = B_SPLINE_CURVE_WITH_KNOTS ( 'NONE', 3,
 ( #11803, #15446, #18110, #24989 ),
 .UNSPECIFIED., .F., .F.,
 ( 4, 4 ),
 ( 0.6000000000734145855, 1.000000000000000000 ),
 .UNSPECIFIED. ) ;
#10497 = CARTESIAN_POINT ( 'NONE',  ( -27.02112178989742119, -1.880880936477675069, -16.19440878182897237 ) ) ;
#10498 = CARTESIAN_POINT ( 'NONE',  ( -11.44473057578096942, 31.45924896672619298, 9.500000000000000000 ) ) ;
#10499 = EDGE_LOOP ( 'NONE', ( #1166, #20251, #26643, #11937 ) ) ;
#10500 = CYLINDRICAL_SURFACE ( 'NONE', #36798, 18.00000000000002132 ) ;
#10501 = CARTESIAN_POINT ( 'NONE',  ( 23.74719310098116765, -8.578385743975788458, 23.00000000000001066 ) ) ;
#10502 = EDGE_CURVE ( 'NONE', #23547, #25420, #12255, .T. ) ;
#10503 = CARTESIAN_POINT ( 'NONE',  ( 33.50338741967450318, -14.65902325991027411, -9.295247887544057619 ) ) ;
#10504 = CARTESIAN_POINT ( 'NONE',  ( 35.86478881511180816, -18.48242683698199329, 12.73282698324857876 ) ) ;
#10505 = AXIS2_PLACEMENT_3D ( 'NONE', #12563, #3417, #15813 ) ;
#10506 = ORIENTED_EDGE ( 'NONE', *, *, #4712, .F. ) ;
#10507 = CARTESIAN_POINT ( 'NONE',  ( -6.811226782241547539, 35.33967249274200384, 10.50000000000000355 ) ) ;
#10508 = CARTESIAN_POINT ( 'NONE',  ( -15.58309971386584536, 26.19172985869298742, -5.000000000000001776 ) ) ;
#10509 = CARTESIAN_POINT ( 'NONE',  ( 3.503793317224327186, 8.420815634768674229, 7.000000000000000000 ) ) ;
#10510 = ORIENTED_EDGE ( 'NONE', *, *, #618, .T. ) ;
#10511 = CARTESIAN_POINT ( 'NONE',  ( -1.824030652502988792, 36.09425736751438052, -10.17475919037218546 ) ) ;
#10512 = LINE ( 'NONE', #39143, #17211 ) ;
#10513 = ADVANCED_FACE ( 'NONE', ( #9789 ), #16080, .T. ) ;
#10514 = DIRECTION ( 'NONE',  ( -0.6691306063588570163, 0.7431448254773953543, -0.000000000000000000 ) ) ;
#10515 = DIRECTION ( 'NONE',  ( 0.000000000000000000, 0.000000000000000000, 1.000000000000000000 ) ) ;
#10516 = DIRECTION ( 'NONE',  ( 0.2079116908177657541, 0.9781476007338044676, -1.803346454958047642E-16 ) ) ;
#10517 = DIRECTION ( 'NONE',  ( 1.000000000000000000, 0.000000000000000000, 0.000000000000000000 ) ) ;
#10518 = CARTESIAN_POINT ( 'NONE',  ( 9.787798997179907090, 18.68458674667809660, -26.07733087769958047 ) ) ;
#10519 = CARTESIAN_POINT ( 'NONE',  ( 14.44277748876681855, 26.55045409923015853, 7.500000000000000888 ) ) ;
#10520 = ORIENTED_EDGE ( 'NONE', *, *, #20565, .F. ) ;
#10521 = AXIS2_PLACEMENT_3D ( 'NONE', #16337, #7381, #1100 ) ;
#10523 = CARTESIAN_POINT ( 'NONE',  ( 12.67417846324118358, 14.47720745114811436, 7.499999999999997335 ) ) ;
#10522 = CARTESIAN_POINT ( 'NONE',  ( -17.23503577783534624, 11.12556197759191967, -29.42916173689316039 ) ) ;
#10524 = EDGE_CURVE ( 'NONE', #19243, #31932, #7452, .T. ) ;
#10525 = CARTESIAN_POINT ( 'NONE',  ( -13.57128027507772039, 27.95460132400015496, 10.49999999999999822 ) ) ;
#10526 = CARTESIAN_POINT ( 'NONE',  ( 14.42086957103650668, -25.08249617576892732, -11.59459791273149065 ) ) ;
#10527 = EDGE_CURVE ( 'NONE', #16505, #24016, #4289, .T. ) ;
#10528 = DIRECTION ( 'NONE',  ( 0.000000000000000000, 0.000000000000000000, -1.000000000000000000 ) ) ;
#10529 = CARTESIAN_POINT ( 'NONE',  ( 13.18496159700378811, 22.28102628015067666, -16.43839240474340713 ) ) ;
#10530 = CARTESIAN_POINT ( 'NONE',  ( -3.091399026088746727, 22.35909668862748134, -19.80438750953544513 ) ) ;
#10531 = CARTESIAN_POINT ( 'NONE',  ( -24.49490654608537454, -11.70163678053536316, 23.00000000000000355 ) ) ;
#10532 = CARTESIAN_POINT ( 'NONE',  ( -27.61224229448858836, -24.44226837637327421, -7.577694500159308788 ) ) ;
#10533 = CIRCLE ( 'NONE', #11178, 0.5000000000000000000 ) ;
#10534 = CARTESIAN_POINT ( 'NONE',  ( 6.261531442577396689, -25.09448364857072633, -5.000000000000002665 ) ) ;
#10535 = CARTESIAN_POINT ( 'NONE',  ( 14.12972245875639032, 23.70285533380211263, -13.52451117403163217 ) ) ;
#10536 = B_SPLINE_CURVE_WITH_KNOTS ( 'NONE', 3,
 ( #16257, #34743, #22338, #15455, #6894, #15657 ),
 .UNSPECIFIED., .F., .F.,
 ( 4, 2, 4 ),
 ( 0.000000000000000000, 0.5000000000000000000, 1.000000000000000000 ),
 .UNSPECIFIED. ) ;
#10537 = CARTESIAN_POINT ( 'NONE',  ( 19.31783821962531533, 13.01333379127007817, -14.91341792948933787 ) ) ;
#10538 = DIRECTION ( 'NONE',  ( 1.000000000000000000, 0.000000000000000000, 0.000000000000000000 ) ) ;
#10539 = CARTESIAN_POINT ( 'NONE',  ( -24.51396478725073180, -11.15767879383071559, 20.99999999999999645 ) ) ;
#10540 = EDGE_LOOP ( 'NONE', ( #36271, #20656, #14297, #2080, #35946 ) ) ;
#10541 = CARTESIAN_POINT ( 'NONE',  ( -8.213440145680040771, 34.88663893459818155, -8.900416981694739604 ) ) ;
#10542 = ORIENTED_EDGE ( 'NONE', *, *, #25872, .T. ) ;
#10543 = CARTESIAN_POINT ( 'NONE',  ( -14.92561699251189999, -26.11061048198896017, -8.769174845341428437 ) ) ;
#10544 = CARTESIAN_POINT ( 'NONE',  ( 4.794796183863160977, 36.71301971979253409, 7.000000000000000000 ) ) ;
#10545 = ORIENTED_EDGE ( 'NONE', *, *, #28354, .F. ) ;
#10546 = CARTESIAN_POINT ( 'NONE',  ( 30.94149296799522020, -0.08026563842153495998, -5.473949085746474097 ) ) ;
#10547 = DIRECTION ( 'NONE',  ( -0.000000000000000000, -0.000000000000000000, -1.000000000000000000 ) ) ;
#10548 = EDGE_CURVE ( 'NONE', #27371, #15493, #1640, .T. ) ;
#10549 = VECTOR ( 'NONE', #15248, 1000.000000000000000 ) ;
#10550 = CARTESIAN_POINT ( 'NONE',  ( -24.20198940123769304, -6.620595927252166391, 20.94377226548377635 ) ) ;
#10551 = ADVANCED_FACE ( 'NONE', ( #35169 ), #35575, .F. ) ;
#10552 = ORIENTED_EDGE ( 'NONE', *, *, #4683, .T. ) ;
#10553 = CARTESIAN_POINT ( 'NONE',  ( -20.96089682640939600, 0.8916499400121695729, -26.23216352804135099 ) ) ;
#10554 = VERTEX_POINT ( 'NONE', #11397 ) ;
#10555 = CARTESIAN_POINT ( 'NONE',  ( 35.07953814774953827, -9.478878833152338146, -7.167510118368202399 ) ) ;
#10556 = CIRCLE ( 'NONE', #7317, 15.00000000000000000 ) ;
#10557 = VERTEX_POINT ( 'NONE', #33344 ) ;
#10558 =( LENGTH_UNIT ( ) NAMED_UNIT ( * ) SI_UNIT ( .MILLI., .METRE. ) );
#10559 = CARTESIAN_POINT ( 'NONE',  ( 5.746222359017451708, 39.55816310746059372, 11.55979286843935405 ) ) ;
#10560 = B_SPLINE_CURVE_WITH_KNOTS ( 'NONE', 3,
 ( #8721, #11967, #33910, #5662 ),
 .UNSPECIFIED., .F., .F.,
 ( 4, 4 ),
 ( 0.000000000000000000, 1.000000000000000000 ),
 .UNSPECIFIED. ) ;
#10561 = CARTESIAN_POINT ( 'NONE',  ( 6.462764152049919275, 17.91932574229959130, 20.99999999999999289 ) ) ;
#10562 = CARTESIAN_POINT ( 'NONE',  ( -12.62435565298219764, 16.36602540378455828, 10.50000000000000000 ) ) ;
#10563 = CARTESIAN_POINT ( 'NONE',  ( -8.307596863006601495, 33.43166269068522212, 18.42518152272108622 ) ) ;
#10564 = CARTESIAN_POINT ( 'NONE',  ( -11.48173768534023154, 32.16538668264431777, 10.49999999999999822 ) ) ;
#10565 = ORIENTED_EDGE ( 'NONE', *, *, #19717, .F. ) ;
#10566 = CARTESIAN_POINT ( 'NONE',  ( 3.118675362266300599, 7.827785988992891575, 7.000000000000000000 ) ) ;
#10567 = LINE ( 'NONE', #35354, #25399 ) ;
#10568 = CYLINDRICAL_SURFACE ( 'NONE', #9799, 0.5000000000000004441 ) ;
#10569 = EDGE_CURVE ( 'NONE', #39330, #9244, #35779, .T. ) ;
#10570 = CARTESIAN_POINT ( 'NONE',  ( 14.83043047287890559, 14.27182183044933694, -28.25080419411967725 ) ) ;
#10571 = AXIS2_PLACEMENT_3D ( 'NONE', #5174, #2132, #2335 ) ;
#10572 = CARTESIAN_POINT ( 'NONE',  ( 9.099779625626309709, 28.28310968578335505, -14.93302891365372886 ) ) ;
#10573 = ORIENTED_EDGE ( 'NONE', *, *, #36674, .F. ) ;
#10574 = FACE_OUTER_BOUND ( 'NONE', #35788, .T. ) ;
#10575 = CARTESIAN_POINT ( 'NONE',  ( -0.6308996938995719006, 37.50000000000000711, 10.49999999999999822 ) ) ;
#10576 = AXIS2_PLACEMENT_3D ( 'NONE', #37197, #21747, #19108 ) ;
#10577 = CARTESIAN_POINT ( 'NONE',  ( 15.87182004195441110, -26.02674557003009426, -9.657777150000830702 ) ) ;
#10578 = DIRECTION ( 'NONE',  ( -0.8660254037844362651, 0.5000000000000043299, 0.000000000000000000 ) ) ;
#10579 = DIRECTION ( 'NONE',  ( 0.6691306063588561281, -0.7431448254773961315, 0.000000000000000000 ) ) ;
#10580 = ORIENTED_EDGE ( 'NONE', *, *, #19102, .T. ) ;
#10581 = CARTESIAN_POINT ( 'NONE',  ( -12.93600697479300621, 21.64018247274085027, -17.43937243684336735 ) ) ;
#10582 = CIRCLE ( 'NONE', #37205, 6.000000000000010658 ) ;
#10583 = CARTESIAN_POINT ( 'NONE',  ( -35.28408311606106906, -16.24929212132110123, 15.72805884748946426 ) ) ;
#10584 = CARTESIAN_POINT ( 'NONE',  ( 9.344739644993655503, -18.38529687660023271, -28.08976026156862105 ) ) ;
#10585 = CARTESIAN_POINT ( 'NONE',  ( -0.01803903918367114056, 14.62372257652092422, 13.00000000000000178 ) ) ;
#10586 = EDGE_LOOP ( 'NONE', ( #24496, #30985, #22011, #37133 ) ) ;
#10587 = EDGE_LOOP ( 'NONE', ( #22604, #20788, #20401, #38216 ) ) ;
#10588 = CARTESIAN_POINT ( 'NONE',  ( -8.438355134513948030, 19.20186035763207855, -26.59191105792285015 ) ) ;
#10589 = CARTESIAN_POINT ( 'NONE',  ( -18.98517869367844924, -25.27528659947290990, -11.33194675744996971 ) ) ;
#10590 = VECTOR ( 'NONE', #16775, 1000.000000000000000 ) ;
#10591 = CARTESIAN_POINT ( 'NONE',  ( 14.01837422881150452, 21.26636931122159169, 6.000000000000000000 ) ) ;
#10592 = CARTESIAN_POINT ( 'NONE',  ( -19.91373213366430761, -4.906168661338282888, -29.99999999999999645 ) ) ;
#10593 = AXIS2_PLACEMENT_3D ( 'NONE', #34254, #15162, #15560 ) ;
#10594 = DIRECTION ( 'NONE',  ( -0.1470157664652027019, -0.6916548014802211819, -0.7071067811865510144 ) ) ;
#10595 = ORIENTED_EDGE ( 'NONE', *, *, #19818, .T. ) ;
#10596 = CARTESIAN_POINT ( 'NONE',  ( 20.95770388837388865, 0.9215809845027531644, -26.23473912195051838 ) ) ;
#10597 = CARTESIAN_POINT ( 'NONE',  ( 13.76592227337845209, 23.41050468301912346, -14.45573797668741634 ) ) ;
#10598 = CARTESIAN_POINT ( 'NONE',  ( 3.597409820281487480, 14.42008525284347087, 7.000000000000000000 ) ) ;
#10599 = ORIENTED_EDGE ( 'NONE', *, *, #2466, .T. ) ;
#10600 = CARTESIAN_POINT ( 'NONE',  ( -25.21984550008777148, 0.3633275739477161981, -17.43674445742407997 ) ) ;
#10601 = CARTESIAN_POINT ( 'NONE',  ( -20.51299636258527315, -31.28130022544801392, 10.99999999999999645 ) ) ;
#10603 = EDGE_CURVE ( 'NONE', #20519, #25405, #5094, .T. ) ;
#10602 = ORIENTED_EDGE ( 'NONE', *, *, #12309, .F. ) ;
#10604 = CARTESIAN_POINT ( 'NONE',  ( 33.84582931909603332, -4.187585590875373853, -5.904510056914596738 ) ) ;
#10605 = VECTOR ( 'NONE', #7445, 1000.000000000000000 ) ;
#10606 = CARTESIAN_POINT ( 'NONE',  ( 13.96856925441951880, 15.00887706487568352, -30.00000000000001066 ) ) ;
#10607 = CARTESIAN_POINT ( 'NONE',  ( 22.57839169151760217, -28.22498753043745978, 14.53008259253988577 ) ) ;
#10608 = ORIENTED_EDGE ( 'NONE', *, *, #25798, .T. ) ;
#10609 = CARTESIAN_POINT ( 'NONE',  ( -5.259215691052897768, 38.11244126491425277, 15.72805884748939853 ) ) ;
#10610 = CARTESIAN_POINT ( 'NONE',  ( -5.257622542056430426, -24.31502561551697283, 16.87380292611441845 ) ) ;
#10611 = FACE_OUTER_BOUND ( 'NONE', #9598, .T. ) ;
#10612 = CARTESIAN_POINT ( 'NONE',  ( -4.723668461522841053E-14, 28.28960257232502684, 20.99999999999998934 ) ) ;
#10613 = AXIS2_PLACEMENT_3D ( 'NONE', #12160, #23955, #30254 ) ;
#10614 = PLANE ( 'NONE',  #18107 ) ;
#10615 = DIRECTION ( 'NONE',  ( -0.000000000000000000, -0.000000000000000000, -1.000000000000000000 ) ) ;
#10616 = EDGE_CURVE ( 'NONE', #3736, #17087, #7932, .T. ) ;
#10617 = CARTESIAN_POINT ( 'NONE',  ( 4.348106467989403257, 35.16482219193073178, 6.000000000000000000 ) ) ;
#10618 = AXIS2_PLACEMENT_3D ( 'NONE', #17973, #6355, #18170 ) ;
#10619 = EDGE_CURVE ( 'NONE', #26362, #28707, #19819, .T. ) ;
#10620 = CARTESIAN_POINT ( 'NONE',  ( 16.81914744106122228, 21.75867863382669753, 16.30093088679352320 ) ) ;
#10621 = CARTESIAN_POINT ( 'NONE',  ( -19.47111235004281937, 7.144292970305836654, -26.58057671234093888 ) ) ;
#10622 = CARTESIAN_POINT ( 'NONE',  ( 19.81334941875573108, -24.54698869046120535, -12.19926732474853814 ) ) ;
#10623 = CARTESIAN_POINT ( 'NONE',  ( -32.54675706181794936, -20.70611888103728049, -4.999999999999999112 ) ) ;
#10624 = CARTESIAN_POINT ( 'NONE',  ( 11.34939637619692121, 18.55308824603512363, -23.83256028268874260 ) ) ;
#10625 = VECTOR ( 'NONE', #16219, 999.9999999999998863 ) ;
#10626 = ORIENTED_EDGE ( 'NONE', *, *, #22993, .F. ) ;
#10627 = CARTESIAN_POINT ( 'NONE',  ( -15.81425778636113755, 25.16710388755963024, -6.419180666290403181 ) ) ;
#10628 = EDGE_CURVE ( 'NONE', #10152, #21190, #5487, .T. ) ;
#10629 = CARTESIAN_POINT ( 'NONE',  ( -30.53792857583819398, -5.895195796384474107, 19.27171037444156809 ) ) ;
#10630 = CARTESIAN_POINT ( 'NONE',  ( -13.24038105676664578, 15.43301270189234309, 10.50000000000000000 ) ) ;
#10631 = CARTESIAN_POINT ( 'NONE',  ( 11.34936283256858225, 18.00731010319261927, -25.01985386284653146 ) ) ;
#10632 = ORIENTED_EDGE ( 'NONE', *, *, #17791, .T. ) ;
#10633 = CARTESIAN_POINT ( 'NONE',  ( 18.16597811475082835, -10.02368442138252114, -27.70584967217684280 ) ) ;
#10634 = FACE_OUTER_BOUND ( 'NONE', #30682, .T. ) ;
#10635 = VERTEX_POINT ( 'NONE', #4892 ) ;
#10637 = DIRECTION ( 'NONE',  ( -0.000000000000000000, -0.000000000000000000, -1.000000000000000000 ) ) ;
#10636 = CARTESIAN_POINT ( 'NONE',  ( -15.22095580511879120, 27.34682230800605751, -5.939933693853666874 ) ) ;
#10638 = CARTESIAN_POINT ( 'NONE',  ( -16.64260134343204101, -26.86770968575480012, -6.862158467649761562 ) ) ;
#10639 = CARTESIAN_POINT ( 'NONE',  ( 13.35472669706387272, 15.66947210016787118, 7.455686640544899824 ) ) ;
#10640 = VECTOR ( 'NONE', #25094, 1000.000000000000114 ) ;
#10641 = ORIENTED_EDGE ( 'NONE', *, *, #8926, .T. ) ;
#10642 = CARTESIAN_POINT ( 'NONE',  ( -35.33747858074038817, -13.37758297739395452, -5.862854311016519659 ) ) ;
#10643 = CARTESIAN_POINT ( 'NONE',  ( -14.73998792673631542, -26.43434547851132166, -6.889327648708172269 ) ) ;
#10644 = CARTESIAN_POINT ( 'NONE',  ( -12.37435565298220119, 15.93301270189233598, 7.499999999999993783 ) ) ;
#10645 = CARTESIAN_POINT ( 'NONE',  ( 15.31670499384548023, 17.89843587122107493, -17.77664689643157558 ) ) ;
#10646 = VERTEX_POINT ( 'NONE', #14033 ) ;
#10647 = CARTESIAN_POINT ( 'NONE',  ( 20.04042991074784652, 4.507464788493477315, -28.80730530478267681 ) ) ;
#10648 = DIRECTION ( 'NONE',  ( -0.3090169943749448977, 0.9510565162951543083, 0.000000000000000000 ) ) ;
#10649 = DIRECTION ( 'NONE',  ( 0.7032331762534119735, 0.07391278520356013571, -0.7071067811865404673 ) ) ;
#10650 = VERTEX_POINT ( 'NONE', #17302 ) ;
#10651 = ADVANCED_FACE ( 'NONE', ( #30079 ), #2252, .F. ) ;
#10652 = CARTESIAN_POINT ( 'NONE',  ( -25.35686378040836075, 0.1132805088522348264, -17.40355568153567134 ) ) ;
#10653 = ADVANCED_FACE ( 'NONE', ( #7736 ), #39413, .T. ) ;
#10654 = CARTESIAN_POINT ( 'NONE',  ( 20.83961557846457424, 0.5176935620071271282, -26.80626269608042023 ) ) ;
#10655 = VECTOR ( 'NONE', #11818, 1000.000000000000114 ) ;
#10656 = CARTESIAN_POINT ( 'NONE',  ( 22.56822310031678214, -21.59793901597642574, 19.99202127657133232 ) ) ;
#10657 = EDGE_LOOP ( 'NONE', ( #28277, #9112, #16189, #23388, #22742, #10061, #27003 ) ) ;
#10658 = CARTESIAN_POINT ( 'NONE',  ( -26.53302367738332279, 1.838442054519318525, -13.60518866641464442 ) ) ;
#10659 = CARTESIAN_POINT ( 'NONE',  ( -15.29245034862075769, 32.56469986091995850, -4.999999999999987566 ) ) ;
#10660 = VECTOR ( 'NONE', #29310, 1000.000000000000114 ) ;
#10661 = DIRECTION ( 'NONE',  ( -0.000000000000000000, -0.000000000000000000, -1.000000000000000000 ) ) ;
#10662 = CARTESIAN_POINT ( 'NONE',  ( -5.440908595777636414, 35.94977745735568675, 7.500000000000000888 ) ) ;
#10663 = ADVANCED_FACE ( 'NONE', ( #11193 ), #8345, .F. ) ;
#10664 = VECTOR ( 'NONE', #38995, 1000.000000000000000 ) ;
#10665 = CARTESIAN_POINT ( 'NONE',  ( -11.50946345163895934, 31.52577281809603704, 10.49999999999999822 ) ) ;
#10666 = CARTESIAN_POINT ( 'NONE',  ( 6.557822374958314882, 35.99981354310111215, 10.63089969389957368 ) ) ;
#10667 = ADVANCED_FACE ( 'NONE', ( #35980 ), #23704, .T. ) ;
#10668 = CARTESIAN_POINT ( 'NONE',  ( 9.165204679926031162, 20.33931832809677331, 12.00000000000000000 ) ) ;
#10669 = EDGE_LOOP ( 'NONE', ( #26340, #22035, #17526 ) ) ;
#10670 = DIRECTION ( 'NONE',  ( 0.8660254037844364872, -0.5000000000000038858, 0.000000000000000000 ) ) ;
#10671 = DIRECTION ( 'NONE',  ( 1.000000000000000000, 0.000000000000000000, 0.000000000000000000 ) ) ;
#10672 = CARTESIAN_POINT ( 'NONE',  ( 18.46250793368027487, -16.02721248873823612, -20.80436923686731632 ) ) ;
#10673 = CARTESIAN_POINT ( 'NONE',  ( 14.81197284684443360, 20.44044478137463727, 10.76099332938163577 ) ) ;
#10674 = PLANE ( 'NONE',  #12533 ) ;
#10675 = CARTESIAN_POINT ( 'NONE',  ( 12.32516380029041159, 21.52845440364069063, -18.38234602673094287 ) ) ;
#10676 = DIRECTION ( 'NONE',  ( 1.000000000000000000, 0.000000000000000000, 0.000000000000000000 ) ) ;
#10677 = ORIENTED_EDGE ( 'NONE', *, *, #33881, .T. ) ;
#10678 = CARTESIAN_POINT ( 'NONE',  ( -17.03554767930629410, 20.20091378400016424, -9.804406882113656962 ) ) ;
#10679 = CARTESIAN_POINT ( 'NONE',  ( -25.15015781185978483, -9.899056496887835621, 20.99999999999989697 ) ) ;
#10680 = CARTESIAN_POINT ( 'NONE',  ( 15.33814677726094189, -26.70409432335911859, -5.474165994462620866 ) ) ;
#10681 = CARTESIAN_POINT ( 'NONE',  ( -2.036571916123810055, 8.108948098542073879, 7.499999999999997335 ) ) ;
#10682 = CARTESIAN_POINT ( 'NONE',  ( 14.29780702217399657, 24.45410663696299736, -12.55099008032420471 ) ) ;
#10683 = ORIENTED_EDGE ( 'NONE', *, *, #18215, .F. ) ;
#10684 = CARTESIAN_POINT ( 'NONE',  ( 11.30219353822485395, 18.04414504934459984, -25.01352393563159282 ) ) ;
#10685 = ORIENTED_EDGE ( 'NONE', *, *, #37560, .T. ) ;
#10687 = CARTESIAN_POINT ( 'NONE',  ( 14.18553059334559308, 26.06413323176228047, 10.49999999999999822 ) ) ;
#10686 = CARTESIAN_POINT ( 'NONE',  ( -13.72666537043441615, 23.49252283158499921, -14.46614592794059284 ) ) ;
#10688 = CARTESIAN_POINT ( 'NONE',  ( -10.80461807628140392, -19.99823691242070467, -21.62132452699231422 ) ) ;
#10689 = CARTESIAN_POINT ( 'NONE',  ( -20.78373334066888845, -29.14101728923843027, 12.14047268033097460 ) ) ;
#10690 = CIRCLE ( 'NONE', #13932, 1.000000000000000888 ) ;
#10691 = CARTESIAN_POINT ( 'NONE',  ( -29.53691847232408918, -17.84505293552917493, -11.97318411411579575 ) ) ;
#10692 = CARTESIAN_POINT ( 'NONE',  ( -9.209455750247457217, -25.27647548880431216, -7.390589557538877585 ) ) ;
#10693 = CARTESIAN_POINT ( 'NONE',  ( 15.55043953303557380, 24.72954629399698590, -8.782262712390135562 ) ) ;
#10694 = ORIENTED_EDGE ( 'NONE', *, *, #20086, .F. ) ;
#10695 = CARTESIAN_POINT ( 'NONE',  ( 23.51665520216067051, 8.202378042728126317, -9.863491397679609918 ) ) ;
#10696 = CARTESIAN_POINT ( 'NONE',  ( 23.90699799611010334, -26.67493067552189601, -4.999999999999999112 ) ) ;
#10697 = LINE ( 'NONE', #10493, #5643 ) ;
#10698 = DIRECTION ( 'NONE',  ( -0.9781476007338042455, 0.2079116908177663370, 0.000000000000000000 ) ) ;
#10699 = CIRCLE ( 'NONE', #11999, 6.000000000000003553 ) ;
#10700 = ORIENTED_EDGE ( 'NONE', *, *, #7030, .F. ) ;
#10701 = CARTESIAN_POINT ( 'NONE',  ( -31.30770620205629129, -1.570573974800437700, -9.148545248552471421 ) ) ;
#10702 = CARTESIAN_POINT ( 'NONE',  ( -13.32438941869583005, 7.692839817671220715, 20.94377226548378346 ) ) ;
#10703 = ORIENTED_EDGE ( 'NONE', *, *, #16004, .T. ) ;
#10704 = FACE_OUTER_BOUND ( 'NONE', #25092, .T. ) ;
#10705 = DIRECTION ( 'NONE',  ( 0.000000000000000000, 0.000000000000000000, 1.000000000000000000 ) ) ;
#10706 = EDGE_CURVE ( 'NONE', #16758, #12080, #26424, .T. ) ;
#10707 = DIRECTION ( 'NONE',  ( 0.000000000000000000, 0.000000000000000000, 1.000000000000000000 ) ) ;
#10708 = CARTESIAN_POINT ( 'NONE',  ( 32.17432900182389943, -14.06792078237634414, -11.08295527558030180 ) ) ;
#10709 = CARTESIAN_POINT ( 'NONE',  ( 36.04785107591603577, -18.56329043283703584, 11.55979286843940557 ) ) ;
#10710 = ORIENTED_EDGE ( 'NONE', *, *, #30647, .T. ) ;
#10711 = DIRECTION ( 'NONE',  ( 0.8660254037844364872, -0.5000000000000038858, 0.000000000000000000 ) ) ;
#10712 = DIRECTION ( 'NONE',  ( 1.000000000000000000, 0.000000000000000000, -0.000000000000000000 ) ) ;
#10713 = AXIS2_PLACEMENT_3D ( 'NONE', #4634, #26164, #2198 ) ;
#10714 = DIRECTION ( 'NONE',  ( -0.6691306063588561281, 0.7431448254773961315, 0.000000000000000000 ) ) ;
#10715 = ORIENTED_EDGE ( 'NONE', *, *, #24933, .F. ) ;
#10716 = CARTESIAN_POINT ( 'NONE',  ( -0.7281348173785022748, 36.90684702921205940, -9.281235812587201650 ) ) ;
#10717 = DIRECTION ( 'NONE',  ( 0.000000000000000000, 0.000000000000000000, 1.000000000000000000 ) ) ;
#10718 = DIRECTION ( 'NONE',  ( -0.000000000000000000, -0.000000000000000000, 1.000000000000000000 ) ) ;
#10719 = CIRCLE ( 'NONE', #5520, 6.000000000000005329 ) ;
#10720 = DIRECTION ( 'NONE',  ( 0.000000000000000000, 0.000000000000000000, 1.000000000000000000 ) ) ;
#10721 = CYLINDRICAL_SURFACE ( 'NONE', #4172, 1.000000000000000888 ) ;
#10722 = CARTESIAN_POINT ( 'NONE',  ( -1.247473515615844075, 16.63111439559750693, 13.00000000000000178 ) ) ;
#10723 = CARTESIAN_POINT ( 'NONE',  ( 13.74729660097108663, 28.63478031050133410, -9.567228944388832090 ) ) ;
#10725 = AXIS2_PLACEMENT_3D ( 'NONE', #9523, #16410, #34696 ) ;
#10724 = CARTESIAN_POINT ( 'NONE',  ( 0.000000000000000000, 22.50000000000000355, 13.00000000000000178 ) ) ;
#10726 = ORIENTED_EDGE ( 'NONE', *, *, #8628, .T. ) ;
#10729 = DIRECTION ( 'NONE',  ( 0.8660254037844432595, 0.4999999999999921729, 0.000000000000000000 ) ) ;
#10728 = VECTOR ( 'NONE', #30080, 1000.000000000000000 ) ;
#10727 = CARTESIAN_POINT ( 'NONE',  ( -20.16920377049624591, 14.63653134085040541, -6.451392141180062545 ) ) ;
#10730 = DIRECTION ( 'NONE',  ( 0.000000000000000000, 0.000000000000000000, 1.000000000000000000 ) ) ;
#10731 = CARTESIAN_POINT ( 'NONE',  ( 15.49955545918230548, -26.71975771321320181, -5.945739302876239307 ) ) ;
#10732 = DIRECTION ( 'NONE',  ( 0.000000000000000000, 0.000000000000000000, 1.000000000000000000 ) ) ;
#10733 = CARTESIAN_POINT ( 'NONE',  ( 14.51660510353637257, 25.01588927535994955, -11.59567232272055470 ) ) ;
#10734 = CARTESIAN_POINT ( 'NONE',  ( -35.84808252048276955, -3.038699442442197807, -13.99876745781545218 ) ) ;
#10735 = FACE_OUTER_BOUND ( 'NONE', #92, .T. ) ;
#10736 = CARTESIAN_POINT ( 'NONE',  ( -17.00128974941928917, -15.01612503178150071, -23.10570941354218633 ) ) ;
#10737 = CARTESIAN_POINT ( 'NONE',  ( 7.126221445658505793, -19.51322017656814722, -27.01549118789370141 ) ) ;
#10738 = CARTESIAN_POINT ( 'NONE',  ( 14.95545557393707092, 25.26472974152139983, -10.18678968210642566 ) ) ;
#10739 = CARTESIAN_POINT ( 'NONE',  ( 17.11772138832456847, 11.31348593724026053, -28.86057714366049609 ) ) ;
#10740 = DIRECTION ( 'NONE',  ( 1.000000000000000000, 0.000000000000000000, 0.000000000000000000 ) ) ;
#10741 = LINE ( 'NONE', #21431, #4048 ) ;
#10742 = ORIENTED_EDGE ( 'NONE', *, *, #11766, .F. ) ;
#10743 = CARTESIAN_POINT ( 'NONE',  ( -6.386588552221052595, 37.17016244130430636, -5.438612508982328286 ) ) ;
#10744 = EDGE_LOOP ( 'NONE', ( #12159, #15730, #9806, #38573 ) ) ;
#10745 = CARTESIAN_POINT ( 'NONE',  ( -13.90807750521352304, -24.59146351958235144, -12.55541049602243575 ) ) ;
#10746 = CARTESIAN_POINT ( 'NONE',  ( -9.427394962683591118, 11.06314620782489833, 10.49999999999999822 ) ) ;
#10747 = EDGE_LOOP ( 'NONE', ( #51, #28130, #31233 ) ) ;
#10748 = CARTESIAN_POINT ( 'NONE',  ( 4.118671991557230072, 37.17221401100731981, 12.00000000000000000 ) ) ;
#10749 = ADVANCED_FACE ( 'NONE', ( #29473 ), #32539, .F. ) ;
#10750 = CARTESIAN_POINT ( 'NONE',  ( -14.48927117870122316, -30.61587158504648087, 3.000000000000000000 ) ) ;
#10751 = ORIENTED_EDGE ( 'NONE', *, *, #2717, .T. ) ;
#10752 = AXIS2_PLACEMENT_3D ( 'NONE', #7973, #17343, #39058 ) ;
#10753 = CARTESIAN_POINT ( 'NONE',  ( -30.79543237407852985, 0.06882123448303990865, -5.474165231917279328 ) ) ;
#10754 = ORIENTED_EDGE ( 'NONE', *, *, #32131, .F. ) ;
#10755 = CARTESIAN_POINT ( 'NONE',  ( 34.24879707383919936, -9.221469049884310820, -8.917830257142501438 ) ) ;
#10756 = VECTOR ( 'NONE', #35247, 1000.000000000000000 ) ;
#10757 = AXIS2_PLACEMENT_3D ( 'NONE', #34963, #4682, #16680 ) ;
#10758 = EDGE_CURVE ( 'NONE', #24136, #11294, #30285, .T. ) ;
#10759 = ORIENTED_EDGE ( 'NONE', *, *, #20330, .F. ) ;
#10760 = CARTESIAN_POINT ( 'NONE',  ( -17.28285333400955182, 27.30382183500235271, 12.14047268033097460 ) ) ;
#10761 = EDGE_CURVE ( 'NONE', #18018, #38835, #36042, .T. ) ;
#10762 = CARTESIAN_POINT ( 'NONE',  ( -6.651296319737220131, 27.81603774131167839, 9.000000000000001776 ) ) ;
#10763 = DIRECTION ( 'NONE',  ( -0.9945218953682745111, -0.1045284632676436454, 0.000000000000000000 ) ) ;
#10764 = CARTESIAN_POINT ( 'NONE',  ( -1.485997264023686038, 36.23016441347868977, 18.42518152272108622 ) ) ;
#10765 = CARTESIAN_POINT ( 'NONE',  ( -10.36702044712415116, 31.16169077310601665, 9.500000000000000000 ) ) ;
#10766 = ORIENTED_EDGE ( 'NONE', *, *, #18060, .F. ) ;
#10767 = DIRECTION ( 'NONE',  ( 0.000000000000000000, 0.000000000000000000, 1.000000000000000000 ) ) ;
#10768 = DIRECTION ( 'NONE',  ( 1.000000000000000000, 0.000000000000000000, 0.000000000000000000 ) ) ;
#10769 = CARTESIAN_POINT ( 'NONE',  ( -13.95683075005229767, 28.08631143191951196, 10.50000000000000533 ) ) ;
#10770 = DIRECTION ( 'NONE',  ( 1.000000000000000000, 0.000000000000000000, 0.000000000000000000 ) ) ;
#10771 = CARTESIAN_POINT ( 'NONE',  ( 18.84172639249922909, 16.68708957390086312, -8.877532344250958829 ) ) ;
#10772 = CARTESIAN_POINT ( 'NONE',  ( 6.542235822104545129, 20.26185204575804022, -25.79941729011566309 ) ) ;
#10773 = EDGE_LOOP ( 'NONE', ( #25581, #18890, #34965, #24286 ) ) ;
#10774 = CYLINDRICAL_SURFACE ( 'NONE', #28104, 0.5000000000000004441 ) ;
#10775 = CARTESIAN_POINT ( 'NONE',  ( 3.494936919103933448, 34.23777120880591696, 13.00000000000000178 ) ) ;
#10776 = EDGE_CURVE ( 'NONE', #27469, #27237, #26827, .T. ) ;
#10777 = EDGE_CURVE ( 'NONE', #38307, #34486, #1002, .T. ) ;
#10778 = CARTESIAN_POINT ( 'NONE',  ( 13.65807228238010573, -23.12680062072891118, -15.38534464500674659 ) ) ;
#10779 = CARTESIAN_POINT ( 'NONE',  ( 15.74227866053861824, -25.75916161678321004, 17.42190598798392998 ) ) ;
#10780 = CIRCLE ( 'NONE', #15327, 1.000000000000000000 ) ;
#10781 = LINE ( 'NONE', #4072, #32974 ) ;
#10782 = VERTEX_POINT ( 'NONE', #38617 ) ;
#10783 = AXIS2_PLACEMENT_3D ( 'NONE', #28603, #19256, #13157 ) ;
#10784 = CARTESIAN_POINT ( 'NONE',  ( -11.11991152073464484, 17.61650879674641246, -26.82993365721759460 ) ) ;
#10785 = VECTOR ( 'NONE', #6429, 1000.000000000000000 ) ;
#10786 = CARTESIAN_POINT ( 'NONE',  ( -33.34742602403127165, -19.25314539175551332, 16.30093088680190760 ) ) ;
#10787 = CARTESIAN_POINT ( 'NONE',  ( 15.03800791059918396, -26.62802654356141119, -5.474101061827365555 ) ) ;
#10788 = AXIS2_PLACEMENT_3D ( 'NONE', #26365, #1590, #38758 ) ;
#10789 = CARTESIAN_POINT ( 'NONE',  ( -9.819582157326459892, 24.63911342745442568, 10.50000000000000533 ) ) ;
#10790 = ORIENTED_EDGE ( 'NONE', *, *, #8628, .F. ) ;
#10791 = ORIENTED_EDGE ( 'NONE', *, *, #26108, .F. ) ;
#10792 = CARTESIAN_POINT ( 'NONE',  ( -10.94743835640653806, 25.45487626883825172, -16.07729632899789962 ) ) ;
#10793 = CARTESIAN_POINT ( 'NONE',  ( -5.440908595777636414, 35.94977745735568675, 7.500000000000000888 ) ) ;
#10794 = DIRECTION ( 'NONE',  ( 0.5877852522924792433, 0.8090169943749431214, 0.000000000000000000 ) ) ;
#10795 = CARTESIAN_POINT ( 'NONE',  ( -33.91433556152139062, -7.380049849088682556, -8.955366286169795131 ) ) ;
#10796 = CARTESIAN_POINT ( 'NONE',  ( 7.312035131040564906, 19.41226734497195849, 6.000000000000000000 ) ) ;
#10797 = VERTEX_POINT ( 'NONE', #36573 ) ;
#10798 = CARTESIAN_POINT ( 'NONE',  ( 20.51905432487639303, 1.011595284947182982, -28.71231566379986688 ) ) ;
#10799 = CARTESIAN_POINT ( 'NONE',  ( -14.51034691152591805, -19.54383025136282725, -20.13759940192544562 ) ) ;
#10800 = DIRECTION ( 'NONE',  ( -0.9781476007338072431, -0.2079116908177519041, 0.000000000000000000 ) ) ;
#10801 = LINE ( 'NONE', #26231, #480 ) ;
#10802 = UNCERTAINTY_MEASURE_WITH_UNIT (LENGTH_MEASURE( 1.000000000000000082E-05 ), #25494, 'distance_accuracy_value', 'NONE');
#10803 = ORIENTED_EDGE ( 'NONE', *, *, #31583, .F. ) ;
#10804 = CARTESIAN_POINT ( 'NONE',  ( -21.71245050099948415, 0.7107615646682705624, -23.85198221761060822 ) ) ;
#10805 = EDGE_CURVE ( 'NONE', #35366, #21446, #32146, .T. ) ;
#10806 = DIRECTION ( 'NONE',  ( 0.8660254037844363761, -0.5000000000000038858, 0.000000000000000000 ) ) ;
#10807 = VERTEX_POINT ( 'NONE', #28025 ) ;
#10808 = CARTESIAN_POINT ( 'NONE',  ( 32.87498921192744206, -3.141057219873002904, -7.719697989364024515 ) ) ;
#10809 = DIRECTION ( 'NONE',  ( -0.5000000000000038858, -0.8660254037844363761, 0.000000000000000000 ) ) ;
#10810 = CARTESIAN_POINT ( 'NONE',  ( 31.99827245170146739, -22.69195664478511887, 15.13084544680246246 ) ) ;
#10811 = ORIENTED_EDGE ( 'NONE', *, *, #4069, .T. ) ;
#10812 = CARTESIAN_POINT ( 'NONE',  ( -3.468257360957398561, 38.22173125672347282, 16.30093088680195379 ) ) ;
#10813 = CARTESIAN_POINT ( 'NONE',  ( 4.310286166645415044E-14, -23.76115801358234947, 17.42190598798392998 ) ) ;
#10814 = DIRECTION ( 'NONE',  ( 1.000000000000000000, 0.000000000000000000, 0.000000000000000000 ) ) ;
#10815 = CARTESIAN_POINT ( 'NONE',  ( 6.337050370968067448, 27.87972302178011930, 20.69868183039781329 ) ) ;
#10816 = AXIS2_PLACEMENT_3D ( 'NONE', #18585, #28115, #37066 ) ;
#10817 = CARTESIAN_POINT ( 'NONE',  ( -13.49038105676664223, 15.86602540378456361, 11.00000000000000000 ) ) ;
#10818 = VERTEX_POINT ( 'NONE', #18689 ) ;
#10819 = DIRECTION ( 'NONE',  ( -1.000000000000000000, 0.000000000000000000, 0.000000000000000000 ) ) ;
#10820 = CARTESIAN_POINT ( 'NONE',  ( 4.786734853113896904, 35.82772156925080509, -9.744462803125076178 ) ) ;
#10821 = DIRECTION ( 'NONE',  ( 0.000000000000000000, 0.000000000000000000, 1.000000000000000000 ) ) ;
#10822 = CARTESIAN_POINT ( 'NONE',  ( 13.31403195191067290, 20.45929608435098501, 19.27171037444031043 ) ) ;
#10823 = CARTESIAN_POINT ( 'NONE',  ( -19.17389268837527538, 8.645407496481396947, -24.39727980451651845 ) ) ;
#10824 = ADVANCED_FACE ( 'NONE', ( #27624 ), #8745, .F. ) ;
#10825 = CARTESIAN_POINT ( 'NONE',  ( 19.29636281975407641, -23.92107482882588698, -13.13705708359962898 ) ) ;
#10826 = DIRECTION ( 'NONE',  ( 1.000000000000000000, 0.000000000000000000, 0.000000000000000000 ) ) ;
#10827 = DIRECTION ( 'NONE',  ( 0.000000000000000000, 0.000000000000000000, 1.000000000000000000 ) ) ;
#10828 = ORIENTED_EDGE ( 'NONE', *, *, #8705, .T. ) ;
#10829 = CARTESIAN_POINT ( 'NONE',  ( 13.71091892849755389, 23.52758077876742604, -14.46248064163161118 ) ) ;
#10830 = ORIENTED_EDGE ( 'NONE', *, *, #1026, .F. ) ;
#10831 = CARTESIAN_POINT ( 'NONE',  ( -13.53743224670682110, 20.67868719046468939, -17.53536389037096299 ) ) ;
#10832 = CARTESIAN_POINT ( 'NONE',  ( -30.92601969764245595, -9.797982979854426233, 19.66345542862527651 ) ) ;
#10833 = CARTESIAN_POINT ( 'NONE',  ( -4.100643064501314328, 15.70406341247269211, 12.00000000000000000 ) ) ;
#10834 = CARTESIAN_POINT ( 'NONE',  ( 11.53052341169412287, 18.39746216749503205, -23.86097604571838815 ) ) ;
#10835 = ORIENTED_EDGE ( 'NONE', *, *, #18486, .F. ) ;
#10836 = CARTESIAN_POINT ( 'NONE',  ( 32.50613532488242896, -16.64577724727427466, -9.727483418184714736 ) ) ;
#10837 = EDGE_LOOP ( 'NONE', ( #557, #35903, #21776, #18731 ) ) ;
#10839 = DIRECTION ( 'NONE',  ( -1.000000000000000000, 0.000000000000000000, 0.000000000000000000 ) ) ;
#10838 = CARTESIAN_POINT ( 'NONE',  ( -11.45602697265520042, 19.13019776967873398, -22.69526440986508575 ) ) ;
#10840 = CARTESIAN_POINT ( 'NONE',  ( -16.07798611810649092, -26.06690065413934221, -9.647245371388256885 ) ) ;
#10841 = CARTESIAN_POINT ( 'NONE',  ( -14.31603901957233660, 19.98981538725089990, 7.000000000000000000 ) ) ;
#10842 = CIRCLE ( 'NONE', #13409, 0.5000000000000004441 ) ;
#10843 = CIRCLE ( 'NONE', #20568, 1.000000000000000888 ) ;
#10844 = ORIENTED_EDGE ( 'NONE', *, *, #11505, .T. ) ;
#10845 = CARTESIAN_POINT ( 'NONE',  ( -34.43511996550268606, -14.21315942988885084, -7.987749063897047641 ) ) ;
#10846 = CARTESIAN_POINT ( 'NONE',  ( -9.288332648570273520, -18.50011473801034612, -27.47095926884810169 ) ) ;
#10847 = CARTESIAN_POINT ( 'NONE',  ( 24.51396478725026640, -11.15767879383072447, 23.00000000000000000 ) ) ;
#10848 = CARTESIAN_POINT ( 'NONE',  ( 13.37783513257456036, 15.99063134506573824, -26.42944179521041903 ) ) ;
#10849 = VERTEX_POINT ( 'NONE', #30487 ) ;
#10850 = CARTESIAN_POINT ( 'NONE',  ( 28.12338329411292648, 2.888959741955042571, -6.424895456845277408 ) ) ;
#10851 = DIRECTION ( 'NONE',  ( 0.000000000000000000, 0.000000000000000000, 1.000000000000000000 ) ) ;
#10852 = LINE ( 'NONE', #23244, #27081 ) ;
#10853 = ORIENTED_EDGE ( 'NONE', *, *, #30990, .F. ) ;
#10854 = CARTESIAN_POINT ( 'NONE',  ( -30.80141499821036533, -0.2118792597572127512, -7.350865256546702753 ) ) ;
#10855 = EDGE_CURVE ( 'NONE', #26924, #22721, #30179, .T. ) ;
#10856 = CARTESIAN_POINT ( 'NONE',  ( 22.29505466895832555, 0.3560692172932813371, -22.69527732140045728 ) ) ;
#10857 = AXIS2_PLACEMENT_3D ( 'NONE', #16568, #16975, #19205 ) ;
#10858 = ADVANCED_FACE ( 'NONE', ( #8946 ), #14840, .F. ) ;
#10859 = CARTESIAN_POINT ( 'NONE',  ( 17.70478766477712185, -23.47393717365348209, 19.27171037444127677 ) ) ;
#10860 = ORIENTED_EDGE ( 'NONE', *, *, #37827, .F. ) ;
#10861 = EDGE_CURVE ( 'NONE', #32505, #32004, #17323, .T. ) ;
#10862 = CARTESIAN_POINT ( 'NONE',  ( -24.38535528688051102, 1.937739723335398567, -17.58705028769485423 ) ) ;
#10863 = CARTESIAN_POINT ( 'NONE',  ( -27.08779848459120743, 7.221796966026712283, -13.42901749168596481 ) ) ;
#10864 = CARTESIAN_POINT ( 'NONE',  ( 14.36830325120613239, 20.48707633493483371, 7.500000000000010658 ) ) ;
#10865 = EDGE_CURVE ( 'NONE', #32296, #22181, #27717, .T. ) ;
#10866 = CARTESIAN_POINT ( 'NONE',  ( 17.34253826607186255, 27.32041144404028543, -5.000000000000000000 ) ) ;
#10867 = AXIS2_PLACEMENT_3D ( 'NONE', #28128, #31378, #505 ) ;
#10868 = VECTOR ( 'NONE', #32890, 1000.000000000000000 ) ;
#10869 = DIRECTION ( 'NONE',  ( 0.000000000000000000, 0.000000000000000000, 1.000000000000000000 ) ) ;
#10870 = FACE_OUTER_BOUND ( 'NONE', #29739, .T. ) ;
#10871 = CARTESIAN_POINT ( 'NONE',  ( 12.92073081513896859, 15.61756285494237773, 10.99999999999999822 ) ) ;
#10872 = VERTEX_POINT ( 'NONE', #2648 ) ;
#10873 = CARTESIAN_POINT ( 'NONE',  ( -24.66395718121962233, 6.133371777919307100, -10.81519827307880277 ) ) ;
#10874 = DIRECTION ( 'NONE',  ( 1.000000000000000000, 0.000000000000000000, 0.000000000000000000 ) ) ;
#10875 = CARTESIAN_POINT ( 'NONE',  ( 7.267999511063016449, 35.13630417120400296, 7.000000000000000000 ) ) ;
#10876 = CARTESIAN_POINT ( 'NONE',  ( 26.18580253464329033, -24.21476188511185157, -9.337349200188750586 ) ) ;
#10877 = EDGE_CURVE ( 'NONE', #17593, #9209, #18887, .T. ) ;
#10878 = AXIS2_PLACEMENT_3D ( 'NONE', #15155, #15555, #3164 ) ;
#10879 = ADVANCED_FACE ( 'NONE', ( #9549 ), #6482, .F. ) ;
#10880 = CARTESIAN_POINT ( 'NONE',  ( -8.472151273871419974, 28.78272654129072095, 10.50000000000000000 ) ) ;
#10881 = LINE ( 'NONE', #1531, #28768 ) ;
#10882 = EDGE_CURVE ( 'NONE', #37740, #26271, #1772, .T. ) ;
#10883 = CARTESIAN_POINT ( 'NONE',  ( 14.40939021871823300, 25.31363344341408350, -11.57339647497523671 ) ) ;
#10884 = CIRCLE ( 'NONE', #35532, 1.000000000000000888 ) ;
#10885 = CARTESIAN_POINT ( 'NONE',  ( 3.914034194965611668, 30.06176806842419680, 7.000000000000000000 ) ) ;
#10886 = ORIENTED_EDGE ( 'NONE', *, *, #36374, .T. ) ;
#10887 = CARTESIAN_POINT ( 'NONE',  ( -17.31397306521514423, 20.64508075850899615, -7.389967135817093968 ) ) ;
#10888 = CARTESIAN_POINT ( 'NONE',  ( -25.16128423893358601, -12.39270898182848768, 20.99999999999999645 ) ) ;
#10889 = CARTESIAN_POINT ( 'NONE',  ( 13.98758249977653634, -24.60317294295146695, -12.55250303098777032 ) ) ;
#10890 = CARTESIAN_POINT ( 'NONE',  ( -11.11016527260153097, 31.83082137946489354, 11.00000000000000000 ) ) ;
#10891 = CARTESIAN_POINT ( 'NONE',  ( 15.40702647791744617, 26.72275646984359199, -5.946082907002145923 ) ) ;
#10892 = EDGE_LOOP ( 'NONE', ( #83, #30543, #39994, #38398 ) ) ;
#10893 = CARTESIAN_POINT ( 'NONE',  ( 14.84111742463147010, 25.60591702902530997, -10.18041830445567442 ) ) ;
#10894 = ORIENTED_EDGE ( 'NONE', *, *, #8626, .T. ) ;
#10896 = CARTESIAN_POINT ( 'NONE',  ( 3.607749162633204332, 7.931741834401772273, 10.63089969389957545 ) ) ;
#10895 = CARTESIAN_POINT ( 'NONE',  ( -13.17768508386178006, 22.29448265875752355, -16.43670467243796551 ) ) ;
#10897 = CARTESIAN_POINT ( 'NONE',  ( -10.50283404165479162, -19.58549042586600919, -22.73910474386799407 ) ) ;
#10898 = CARTESIAN_POINT ( 'NONE',  ( -24.65531199400790996, -28.60128534115777654, 11.55979286843934695 ) ) ;
#10899 = CARTESIAN_POINT ( 'NONE',  ( -32.47674537595472799, -19.61558511033160457, -7.544019131575042003 ) ) ;
#10900 = CARTESIAN_POINT ( 'NONE',  ( -4.880576112647466935, -20.34275454070125733, -25.40727637649297677 ) ) ;
#10901 = CARTESIAN_POINT ( 'NONE',  ( 11.81800289456031727, 17.11319857350586204, -26.89243828160074301 ) ) ;
#10902 = ORIENTED_EDGE ( 'NONE', *, *, #4052, .F. ) ;
#10903 = CARTESIAN_POINT ( 'NONE',  ( 18.88780196539459055, 8.001059241770983377, -29.42544452779240416 ) ) ;
#10904 = CARTESIAN_POINT ( 'NONE',  ( -4.331888841169210913, 42.14502281828541186, 11.00000000000000178 ) ) ;
#10905 = CARTESIAN_POINT ( 'NONE',  ( 0.000000000000000000, 22.50000000000000355, 13.00000000000000178 ) ) ;
#10906 = DIRECTION ( 'NONE',  ( 0.000000000000000000, 0.000000000000000000, 1.000000000000000000 ) ) ;
#10907 = VERTEX_POINT ( 'NONE', #5688 ) ;
#10908 = CARTESIAN_POINT ( 'NONE',  ( -32.83526622438716913, -2.536178072473608935, -6.372889071231118585 ) ) ;
#10909 = ADVANCED_FACE ( 'NONE', ( #31080 ), #18762, .T. ) ;
#10910 = VECTOR ( 'NONE', #206, 1000.000000000000000 ) ;
#10911 = VECTOR ( 'NONE', #5596, 1000.000000000000227 ) ;
#10912 = CARTESIAN_POINT ( 'NONE',  ( -18.38177052347168683, 3.916595739930567532, 20.50957957746028271 ) ) ;
#10913 = ORIENTED_EDGE ( 'NONE', *, *, #10706, .F. ) ;
#10914 = EDGE_CURVE ( 'NONE', #14680, #14045, #23084, .T. ) ;
#10915 = CARTESIAN_POINT ( 'NONE',  ( 23.31768133719840463, -16.68166585059941198, 20.94377226548368398 ) ) ;
#10916 = DIRECTION ( 'NONE',  ( -0.2079116908177663370, -0.9781476007338042455, 0.000000000000000000 ) ) ;
#10917 = AXIS2_PLACEMENT_3D ( 'NONE', #23453, #5558, #32809 ) ;
#10918 =( NAMED_UNIT ( * ) PLANE_ANGLE_UNIT ( ) SI_UNIT ( $, .RADIAN. ) );
#10919 = CARTESIAN_POINT ( 'NONE',  ( 18.51815053109030629, -8.815588134695454769, -30.00000000000002487 ) ) ;
#10921 = AXIS2_PLACEMENT_3D ( 'NONE', #17308, #29682, #1864 ) ;
#10920 = CARTESIAN_POINT ( 'NONE',  ( 22.73075399258389595, -29.06185307675081830, 11.55979286843892595 ) ) ;
#10922 = EDGE_LOOP ( 'NONE', ( #17116, #8357 ) ) ;
#10923 = DIRECTION ( 'NONE',  ( 0.000000000000000000, 0.000000000000000000, 1.000000000000000000 ) ) ;
#10924 = CARTESIAN_POINT ( 'NONE',  ( -14.98890121934610242, -28.67928442654176635, -5.000000000000000000 ) ) ;
#10925 = LINE ( 'NONE', #14364, #34416 ) ;
#10926 = ORIENTED_EDGE ( 'NONE', *, *, #20727, .F. ) ;
#10927 = CARTESIAN_POINT ( 'NONE',  ( 1.098729202488071710, 26.81952012603705526, -18.61434905906123305 ) ) ;
#10928 = CARTESIAN_POINT ( 'NONE',  ( -10.54147634889124063, 27.59512447410525127, 12.00000000000000000 ) ) ;
#10929 = FACE_OUTER_BOUND ( 'NONE', #16627, .T. ) ;
#10930 = CARTESIAN_POINT ( 'NONE',  ( 7.917734535019441466, 14.47043272369397116, 6.000000000000000000 ) ) ;
#10931 = DIRECTION ( 'NONE',  ( 1.000000000000000000, 0.000000000000000000, 0.000000000000000000 ) ) ;
#10932 = DIRECTION ( 'NONE',  ( 1.000000000000000000, 0.000000000000000000, 0.000000000000000000 ) ) ;
#10933 = AXIS2_PLACEMENT_3D ( 'NONE', #17667, #38981, #23544 ) ;
#10934 = CARTESIAN_POINT ( 'NONE',  ( 9.649540945264268643, 19.20465645623720974, -24.79630837131278298 ) ) ;
#10935 = DIRECTION ( 'NONE',  ( 0.000000000000000000, 0.000000000000000000, -1.000000000000000000 ) ) ;
#10936 = AXIS2_PLACEMENT_3D ( 'NONE', #8600, #8405, #20802 ) ;
#10937 = ORIENTED_EDGE ( 'NONE', *, *, #38336, .T. ) ;
#10939 = LINE ( 'NONE', #14173, #5792 ) ;
#10938 = CARTESIAN_POINT ( 'NONE',  ( -17.24968974221940599, 11.13640497999314150, -28.86202543690495759 ) ) ;
#10940 = CARTESIAN_POINT ( 'NONE',  ( 12.30764836806737961, -22.02250499063774214, -17.43528973058483800 ) ) ;
#10941 = DIRECTION ( 'NONE',  ( -0.000000000000000000, -0.000000000000000000, -1.000000000000000000 ) ) ;
#10942 = CARTESIAN_POINT ( 'NONE',  ( 15.39755691330850951, 26.84919286949167017, -4.999999999999998224 ) ) ;
#10943 = AXIS2_PLACEMENT_3D ( 'NONE', #29549, #26502, #20415 ) ;
#10944 = CARTESIAN_POINT ( 'NONE',  ( -17.81784622497958281, -13.85677843414106292, -30.00000000000001421 ) ) ;
#10945 = CARTESIAN_POINT ( 'NONE',  ( -22.38145423153888558, -15.36249082013412171, 23.00000000000000000 ) ) ;
#10946 = AXIS2_PLACEMENT_3D ( 'NONE', #37134, #15198, #27588 ) ;
#10947 = CARTESIAN_POINT ( 'NONE',  ( -20.57193854740110339, -18.21112165086101342, -17.70184765716385300 ) ) ;
#10948 = CARTESIAN_POINT ( 'NONE',  ( 2.809657567551183455, -20.57247227728830907, -26.60406814968515832 ) ) ;
#10949 = CARTESIAN_POINT ( 'NONE',  ( 15.28216090130213267, 25.92595189827088475, -8.300399430041283111 ) ) ;
#10950 = CARTESIAN_POINT ( 'NONE',  ( 16.70239018954916332, 11.94149278131882497, -28.85809821401793229 ) ) ;
#10951 = DIRECTION ( 'NONE',  ( -0.9781476007338043566, 0.2079116908177657264, 0.000000000000000000 ) ) ;
#10952 = ORIENTED_EDGE ( 'NONE', *, *, #11589, .F. ) ;
#10953 = CARTESIAN_POINT ( 'NONE',  ( -6.284372354627114632, 36.40390034292152421, -7.999116229162498648 ) ) ;
#10954 = EDGE_LOOP ( 'NONE', ( #17716, #16368 ) ) ;
#10955 = LINE ( 'NONE', #14397, #5323 ) ;
#10956 = ORIENTED_EDGE ( 'NONE', *, *, #14562, .T. ) ;
#10957 = DIRECTION ( 'NONE',  ( -1.000000000000000000, 0.000000000000000000, 0.000000000000000000 ) ) ;
#10958 = CARTESIAN_POINT ( 'NONE',  ( 8.954580980757247843, 11.02572744104254987, 11.00000000000000000 ) ) ;
#10959 = ORIENTED_EDGE ( 'NONE', *, *, #36602, .T. ) ;
#10960 = CARTESIAN_POINT ( 'NONE',  ( -30.32825103788703203, 0.1531031937912943341, -7.828961834450372415 ) ) ;
#10961 = ORIENTED_EDGE ( 'NONE', *, *, #7479, .F. ) ;
#10962 = CARTESIAN_POINT ( 'NONE',  ( 27.17184055267051335, -8.181037515565595442, -16.75553878453715839 ) ) ;
#10963 = AXIS2_PLACEMENT_3D ( 'NONE', #11512, #20663, #17214 ) ;
#10964 = AXIS2_PLACEMENT_3D ( 'NONE', #24250, #5760, #12055 ) ;
#10965 = EDGE_LOOP ( 'NONE', ( #28268, #19947, #12841, #37426, #9180, #23783, #7117, #27890 ) ) ;
#10966 = DIRECTION ( 'NONE',  ( -0.8660254037844425934, -0.4999999999999933942, -6.938893903907226800E-15 ) ) ;
#10967 = EDGE_LOOP ( 'NONE', ( #28242, #37480, #11060, #12628 ) ) ;
#10968 = CIRCLE ( 'NONE', #30435, 1.000000000000000888 ) ;
#10969 = CARTESIAN_POINT ( 'NONE',  ( -7.935776944912362296, 22.65328985282726393, 12.00000000000000000 ) ) ;
#10970 = CARTESIAN_POINT ( 'NONE',  ( 3.161220354320215975, 12.43736188311278212, 10.50000000000000000 ) ) ;
#10971 = CARTESIAN_POINT ( 'NONE',  ( 7.449887436097998084, 34.87105630051927108, 17.92354375535251521 ) ) ;
#10972 = CARTESIAN_POINT ( 'NONE',  ( -14.98890121934603314, -28.67928442654204346, 11.00000000000000000 ) ) ;
#10973 = VERTEX_POINT ( 'NONE', #32646 ) ;
#10974 = LINE ( 'NONE', #8112, #956 ) ;
#10975 = CYLINDRICAL_SURFACE ( 'NONE', #26691, 1.000000000000000000 ) ;
#10976 = DIRECTION ( 'NONE',  ( 1.000000000000000000, 0.000000000000000000, 0.000000000000000000 ) ) ;
#10977 = CARTESIAN_POINT ( 'NONE',  ( 15.67651070409536018, 15.51254429634443888, -21.03034014038798460 ) ) ;
#10978 = CARTESIAN_POINT ( 'NONE',  ( 6.469800813340902401, 20.02804225434012508, -26.45432154560951332 ) ) ;
#10979 = EDGE_LOOP ( 'NONE', ( #33742, #9786, #19776, #14110, #9005 ) ) ;
#10980 = CARTESIAN_POINT ( 'NONE',  ( -19.48557158514985588, -11.25000000000002309, 0.000000000000000000 ) ) ;
#10981 = CYLINDRICAL_SURFACE ( 'NONE', #30508, 18.00000000000002842 ) ;
#10982 = ADVANCED_FACE ( 'NONE', ( #20046 ), #14142, .F. ) ;
#10983 = CARTESIAN_POINT ( 'NONE',  ( 10.28494437836259401, -18.68278944082468840, -24.97709700113341214 ) ) ;
#10984 = CARTESIAN_POINT ( 'NONE',  ( 35.36940577612500647, -20.42053594592276866, -5.000000000000000000 ) ) ;
#10985 = CARTESIAN_POINT ( 'NONE',  ( -1.000003370709253492, 22.50000000000031264, 13.00000000000000178 ) ) ;
#10986 = AXIS2_PLACEMENT_3D ( 'NONE', #931, #35811, #32570 ) ;
#10987 = ORIENTED_EDGE ( 'NONE', *, *, #6611, .T. ) ;
#10989 = VECTOR ( 'NONE', #24310, 1000.000000000000000 ) ;
#10988 = CARTESIAN_POINT ( 'NONE',  ( -14.02656482509936353, 23.94253483213065437, -13.51260121954110183 ) ) ;
#10990 = CARTESIAN_POINT ( 'NONE',  ( -27.50471383176088480, -25.75100844545737644, 15.72805884748907879 ) ) ;
#10991 = CARTESIAN_POINT ( 'NONE',  ( 9.221110303372956452, -18.35701242422515378, -28.71846602907799451 ) ) ;
#10992 = ADVANCED_FACE ( 'NONE', ( #35278 ), #4192, .T. ) ;
#10993 = DIRECTION ( 'NONE',  ( -0.9945218953682745111, -0.1045284632676437703, 0.000000000000000000 ) ) ;
#10994 = EDGE_CURVE ( 'NONE', #25787, #32523, #16570, .T. ) ;
#10995 = ORIENTED_EDGE ( 'NONE', *, *, #7096, .F. ) ;
#10996 = VERTEX_POINT ( 'NONE', #10290 ) ;
#10997 = CIRCLE ( 'NONE', #7734, 0.4999999999999995559 ) ;
#10998 = CARTESIAN_POINT ( 'NONE',  ( -12.01180344372764530, 30.47904674458951035, -10.37449900079057485 ) ) ;
#10999 = DIRECTION ( 'NONE',  ( 0.000000000000000000, 0.000000000000000000, 1.000000000000000000 ) ) ;
#11000 = FACE_BOUND ( 'NONE', #5700, .T. ) ;
#11001 = CARTESIAN_POINT ( 'NONE',  ( -34.80117605982864148, -8.634413430420472935, -7.612578086861918614 ) ) ;
#11002 = PLANE ( 'NONE',  #1416 ) ;
#11003 = EDGE_LOOP ( 'NONE', ( #33057, #36990 ) ) ;
#11004 = CARTESIAN_POINT ( 'NONE',  ( 22.70770152948616882, 0.6873525397408100091, -21.62692844155446181 ) ) ;
#11005 = DIRECTION ( 'NONE',  ( 1.000000000000000000, 0.000000000000000000, 0.000000000000000000 ) ) ;
#11006 = CARTESIAN_POINT ( 'NONE',  ( -3.610593701936590350, 31.83882289796395426, 10.50000000000000533 ) ) ;
#11007 = CARTESIAN_POINT ( 'NONE',  ( -16.31185170147123387, -29.02059919786648479, 10.99999999999952038 ) ) ;
#11008 = VERTEX_POINT ( 'NONE', #32232 ) ;
#11009 = CARTESIAN_POINT ( 'NONE',  ( -30.80677756886225183, -0.04596665832818841446, -6.416728566985741011 ) ) ;
#11010 = CARTESIAN_POINT ( 'NONE',  ( 4.727507481117209309, 31.88885898370940453, 10.50000000000000000 ) ) ;
#11011 = ORIENTED_EDGE ( 'NONE', *, *, #7121, .T. ) ;
#11012 = CARTESIAN_POINT ( 'NONE',  ( 26.90501378883225314, -1.666325082333041552, -16.21919210836066227 ) ) ;
#11013 = CARTESIAN_POINT ( 'NONE',  ( 15.20016916874550539, -27.86040092368493504, 14.53008259254011136 ) ) ;
#11014 = EDGE_CURVE ( 'NONE', #7168, #22045, #10697, .T. ) ;
#11015 = ORIENTED_EDGE ( 'NONE', *, *, #24715, .F. ) ;
#11016 = CARTESIAN_POINT ( 'NONE',  ( -1.415557151730355161E-13, 39.95159812444026670, 13.92931973827808712 ) ) ;
#11017 = EDGE_CURVE ( 'NONE', #30187, #32040, #3699, .T. ) ;
#11018 = CARTESIAN_POINT ( 'NONE',  ( -15.60391421429489434, -26.29546805948952581, 16.87380292611441490 ) ) ;
#11019 = CARTESIAN_POINT ( 'NONE',  ( 11.14716901145161643, 12.46304090461738667, 13.00000000000000178 ) ) ;
#11020 = CARTESIAN_POINT ( 'NONE',  ( -5.702281711626214999, 27.34093017838354456, 20.82122704794079127 ) ) ;
#11021 = VECTOR ( 'NONE', #37889, 1000.000000000000114 ) ;
#11022 = B_SPLINE_CURVE_WITH_KNOTS ( 'NONE', 3,
 ( #19763, #10214, #32159, #7158, #4319, #10623, #1482, #32772, #1893, #7770 ),
 .UNSPECIFIED., .F., .F.,
 ( 4, 2, 2, 2, 4 ),
 ( 0.1234515740337736034, 0.2679468505892486085, 0.4124421271447235582, 0.5569374037001986188, 0.7014326802556738460 ),
 .UNSPECIFIED. ) ;
#11023 = DIRECTION ( 'NONE',  ( 0.8660254037844377084, -0.5000000000000015543, -3.469446951953621683E-15 ) ) ;
#11024 = EDGE_LOOP ( 'NONE', ( #15050, #25980, #31375, #10641 ) ) ;
#11025 = CARTESIAN_POINT ( 'NONE',  ( -8.015823967414606344, 9.821249526829326726, 7.339470489435493405 ) ) ;
#11026 = CIRCLE ( 'NONE', #23346, 0.5000000000000001110 ) ;
#11027 = CARTESIAN_POINT ( 'NONE',  ( 6.092423932518094887, 37.33975570695338320, -4.999999999999998224 ) ) ;
#11028 = LINE ( 'NONE', #35805, #28160 ) ;
#11029 = CARTESIAN_POINT ( 'NONE',  ( 14.97058623676333866, 26.66112013783126500, 16.87380292611441845 ) ) ;
#11030 = CARTESIAN_POINT ( 'NONE',  ( 19.66234726371370201, -27.08195440243529006, -6.812183372440195228 ) ) ;
#11031 = DIRECTION ( 'NONE',  ( 1.000000000000000000, 0.000000000000000000, 0.000000000000000000 ) ) ;
#11032 = CARTESIAN_POINT ( 'NONE',  ( -12.49038105676665644, 14.13397459621567798, 11.00000000000000000 ) ) ;
#11033 = DIRECTION ( 'NONE',  ( 1.000000000000000000, 0.000000000000000000, 0.000000000000000000 ) ) ;
#11034 = ADVANCED_FACE ( 'NONE', ( #17001 ), #15838, .F. ) ;
#11035 = ORIENTED_EDGE ( 'NONE', *, *, #10007, .T. ) ;
#11036 = CARTESIAN_POINT ( 'NONE',  ( 10.96848842646544853, 17.47186599299789123, -28.07314336957281142 ) ) ;
#11037 = ORIENTED_EDGE ( 'NONE', *, *, #18989, .F. ) ;
#11038 = CARTESIAN_POINT ( 'NONE',  ( -15.58277398399269131, 26.10415450534656046, -5.946235503377694798 ) ) ;
#11039 = CARTESIAN_POINT ( 'NONE',  ( -25.71034552362591796, -20.07240169439133481, 19.99202127657103389 ) ) ;
#11040 = DIRECTION ( 'NONE',  ( 0.000000000000000000, 0.000000000000000000, 1.000000000000000000 ) ) ;
#11041 = CARTESIAN_POINT ( 'NONE',  ( 11.73655712706644572, 18.86307847280393091, -22.74338934216403629 ) ) ;
#11042 = EDGE_CURVE ( 'NONE', #31785, #33916, #5419, .T. ) ;
#11043 = ORIENTED_EDGE ( 'NONE', *, *, #21293, .T. ) ;
#11044 = CARTESIAN_POINT ( 'NONE',  ( 23.11556285573274394, -13.67656654032385966, -18.60984667135146253 ) ) ;
#11045 = ORIENTED_EDGE ( 'NONE', *, *, #35695, .T. ) ;
#11047 = DIRECTION ( 'NONE',  ( 1.000000000000000000, 0.000000000000000000, 0.000000000000000000 ) ) ;
#11046 = CARTESIAN_POINT ( 'NONE',  ( -11.80048683308201518, 20.30964621748999122, -20.47546970256553678 ) ) ;
#11048 = CARTESIAN_POINT ( 'NONE',  ( -13.64307358185168439, -21.94662204693058172, -17.28659994694505997 ) ) ;
#11049 = CARTESIAN_POINT ( 'NONE',  ( 8.118377661053324701, 10.47536095541698486, 9.000000000000001776 ) ) ;
#11050 = VERTEX_POINT ( 'NONE', #1556 ) ;
#11051 = CARTESIAN_POINT ( 'NONE',  ( -30.37997259716803100, -13.60122796121996203, -12.90426562829724055 ) ) ;
#11052 = CARTESIAN_POINT ( 'NONE',  ( -14.59935253407961930, -26.03713580996503296, -8.772365449628392042 ) ) ;
#11053 = CARTESIAN_POINT ( 'NONE',  ( 5.473344025737210572, 14.11593743010426394, 10.49999999999999822 ) ) ;
#11054 = CARTESIAN_POINT ( 'NONE',  ( 16.58472503010262145, 19.97504727872816943, -11.75017852518634776 ) ) ;
#11055 = EDGE_LOOP ( 'NONE', ( #12796, #22524, #17992, #6716, #27587 ) ) ;
#11056 = CARTESIAN_POINT ( 'NONE',  ( 20.18678365231757255, 3.805571786065587769, -28.79240286594302489 ) ) ;
#11057 = DIRECTION ( 'NONE',  ( 1.000000000000000000, 0.000000000000000000, 0.000000000000000000 ) ) ;
#11058 = FACE_OUTER_BOUND ( 'NONE', #26880, .T. ) ;
#11059 = AXIS2_PLACEMENT_3D ( 'NONE', #1573, #30003, #33269 ) ;
#11060 = ORIENTED_EDGE ( 'NONE', *, *, #3147, .F. ) ;
#11061 = CARTESIAN_POINT ( 'NONE',  ( -24.01208527996724840, 0.3188823248074318939, -19.47337513750245819 ) ) ;
#11062 = CARTESIAN_POINT ( 'NONE',  ( 20.63344826760219775, 0.3739914392306604163, -28.05361808214927066 ) ) ;
#11063 = CARTESIAN_POINT ( 'NONE',  ( 31.47522604700277071, -16.54376571344620217, 18.87996532025784546 ) ) ;
#11064 = EDGE_CURVE ( 'NONE', #39958, #20580, #38729, .T. ) ;
#11065 = ORIENTED_EDGE ( 'NONE', *, *, #27652, .T. ) ;
#11066 = CARTESIAN_POINT ( 'NONE',  ( -28.96942539544459549, 1.744189647663177523, -7.367551979210757551 ) ) ;
#11067 = EDGE_CURVE ( 'NONE', #35978, #21042, #8901, .T. ) ;
#11068 = CARTESIAN_POINT ( 'NONE',  ( -30.41237130417910706, 3.314011747244096195, -5.000000000000000000 ) ) ;
#11069 = FACE_OUTER_BOUND ( 'NONE', #9305, .T. ) ;
#11070 = TOROIDAL_SURFACE ( 'NONE', #25341, 16.00000000000000000, 1.000000000000000000 ) ;
#11071 = CARTESIAN_POINT ( 'NONE',  ( -13.46929972531958697, 26.35070966310183138, 7.499999999999994671 ) ) ;
#11072 = DIRECTION ( 'NONE',  ( 1.000000000000000000, 0.000000000000000000, 0.000000000000000000 ) ) ;
#11073 = DIRECTION ( 'NONE',  ( 0.000000000000000000, 0.000000000000000000, -1.000000000000000000 ) ) ;
#11074 = CARTESIAN_POINT ( 'NONE',  ( -9.151574469205524309, 1.945227203041487218, 7.000000000000000000 ) ) ;
#11075 = EDGE_LOOP ( 'NONE', ( #25737, #16681 ) ) ;
#11076 = CARTESIAN_POINT ( 'NONE',  ( -25.54365046647732029, 5.272554438015793821, -9.817126893295599288 ) ) ;
#11077 = DIRECTION ( 'NONE',  ( -1.000000000000000000, 0.000000000000000000, 0.000000000000000000 ) ) ;
#11078 = CYLINDRICAL_SURFACE ( 'NONE', #21395, 1.000000000000000000 ) ;
#11079 = CARTESIAN_POINT ( 'NONE',  ( 26.88891980231563394, -23.41974722532487974, -9.768121312577717319 ) ) ;
#11080 = AXIS2_PLACEMENT_3D ( 'NONE', #34956, #14013, #13407 ) ;
#11081 = CARTESIAN_POINT ( 'NONE',  ( 9.917734535019443243, 14.47043272369397116, 6.000000000000000000 ) ) ;
#11082 = LINE ( 'NONE', #33430, #15149 ) ;
#11083 = EDGE_CURVE ( 'NONE', #37992, #21042, #17982, .T. ) ;
#11084 = CARTESIAN_POINT ( 'NONE',  ( 14.57748215141210757, 25.86296597815312737, -10.62311630137386587 ) ) ;
#11085 = ORIENTED_EDGE ( 'NONE', *, *, #20515, .T. ) ;
#11086 = CARTESIAN_POINT ( 'NONE',  ( -13.90277657046047288, 15.06583648262319031, -30.00000000000000711 ) ) ;
#11087 = CARTESIAN_POINT ( 'NONE',  ( -20.52988490949636713, -16.97904854937761243, 20.99999999999995026 ) ) ;
#11088 = CARTESIAN_POINT ( 'NONE',  ( 13.95448054433643392, -24.59828557378244085, -12.55371339440786116 ) ) ;
#11089 = DIRECTION ( 'NONE',  ( 0.000000000000000000, 0.000000000000000000, 1.000000000000000000 ) ) ;
#11090 = CARTESIAN_POINT ( 'NONE',  ( 13.49780444981478844, 22.80326206385345245, -15.45136375860262845 ) ) ;
#11091 = ORIENTED_EDGE ( 'NONE', *, *, #25743, .T. ) ;
#11092 = CARTESIAN_POINT ( 'NONE',  ( -14.89501059309200137, 21.76138985984223595, 10.49999999999999822 ) ) ;
#11093 = VERTEX_POINT ( 'NONE', #18203 ) ;
#11095 = CARTESIAN_POINT ( 'NONE',  ( 8.238488885696289898, 24.65111619403943877, 9.000000000000001776 ) ) ;
#11094 = CARTESIAN_POINT ( 'NONE',  ( -15.20842241300166009, 26.48812948757255015, -7.825058628721806464 ) ) ;
#11096 = CARTESIAN_POINT ( 'NONE',  ( -15.40614666684921552, -26.59809411392278733, -6.887480037654896137 ) ) ;
#11097 = CARTESIAN_POINT ( 'NONE',  ( -35.99085602461024536, -18.53811353976085030, 12.14047268033095150 ) ) ;
#11098 = CARTESIAN_POINT ( 'NONE',  ( -16.89362134160771944, -11.62925611732713804, -30.00000000000001421 ) ) ;
#11099 = CARTESIAN_POINT ( 'NONE',  ( -5.350130231482848941, -21.35397508028911773, -21.04018493678614377 ) ) ;
#11100 = CARTESIAN_POINT ( 'NONE',  ( 14.54495187225327868, 22.76206543785304248, -13.57072665076263185 ) ) ;
#11101 = ORIENTED_EDGE ( 'NONE', *, *, #33904, .T. ) ;
#11102 = CARTESIAN_POINT ( 'NONE',  ( 23.31974132639167863, 9.208228383191446653, -6.934278112824287632 ) ) ;
#11103 = CIRCLE ( 'NONE', #22102, 1.000000000000000000 ) ;
#11104 = CARTESIAN_POINT ( 'NONE',  ( 13.63581098909226519, 27.45627467658428600, 7.000000000000000000 ) ) ;
#11105 = CARTESIAN_POINT ( 'NONE',  ( 3.863783140547853712E-14, -86.77689918168233874, 3.000000000000000000 ) ) ;
#11106 = DIRECTION ( 'NONE',  ( -0.9135454576426005335, 0.4067366430758009299, 0.000000000000000000 ) ) ;
#11107 = ORIENTED_EDGE ( 'NONE', *, *, #30341, .F. ) ;
#11108 = CARTESIAN_POINT ( 'NONE',  ( -21.08730904962191133, -1.198901753354387534, -26.04825129587869270 ) ) ;
#11109 = CARTESIAN_POINT ( 'NONE',  ( -24.20198940123769304, -6.620595927252167279, 20.94377226548378346 ) ) ;
#11110 = CARTESIAN_POINT ( 'NONE',  ( 24.05659981020950866, -7.641904207658117620, 21.00000000000024514 ) ) ;
#11111 = CARTESIAN_POINT ( 'NONE',  ( 20.38753357181586878, -16.19769905861743808, 20.99999999999998934 ) ) ;
#11112 = VECTOR ( 'NONE', #36358, 1000.000000000000000 ) ;
#11113 = CARTESIAN_POINT ( 'NONE',  ( 33.88951946378950453, -17.36670660975930147, -7.118497633377743661 ) ) ;
#11114 = EDGE_CURVE ( 'NONE', #39423, #25190, #8300, .T. ) ;
#11115 = FACE_OUTER_BOUND ( 'NONE', #5079, .T. ) ;
#11116 = ORIENTED_EDGE ( 'NONE', *, *, #38589, .T. ) ;
#11117 = CARTESIAN_POINT ( 'NONE',  ( 5.348106467989403257, 35.16482219193073178, 6.000000000000000000 ) ) ;
#11118 = CIRCLE ( 'NONE', #28652, 1.000000000000000000 ) ;
#11119 = CARTESIAN_POINT ( 'NONE',  ( 6.557822374958623968, 35.99981354310097004, 10.59344459855570619 ) ) ;
#11120 = CYLINDRICAL_SURFACE ( 'NONE', #19030, 6.000000000000005329 ) ;
#11121 = CARTESIAN_POINT ( 'NONE',  ( 1.552613142282920355, 37.67816372275503767, -7.972283367467844606 ) ) ;
#11122 = FACE_OUTER_BOUND ( 'NONE', #39072, .T. ) ;
#11123 = CARTESIAN_POINT ( 'NONE',  ( -13.24038105676664046, 15.43301270189234486, 10.63089969389957545 ) ) ;
#11124 = CARTESIAN_POINT ( 'NONE',  ( 14.36830325120613239, 20.48707633493483371, 7.000000000000000000 ) ) ;
#11125 = CARTESIAN_POINT ( 'NONE',  ( 7.953805871968279817, 30.22298757065274444, 6.000000000000000000 ) ) ;
#11126 = EDGE_CURVE ( 'NONE', #35341, #6246, #30942, .T. ) ;
#11127 = CARTESIAN_POINT ( 'NONE',  ( 9.165204679926031162, 20.33931832809677331, 6.000000000000000000 ) ) ;
#11128 = CARTESIAN_POINT ( 'NONE',  ( 11.14360014059721848, 20.13980330270795349, -21.48012828381845196 ) ) ;
#11129 = FACE_OUTER_BOUND ( 'NONE', #30436, .T. ) ;
#11130 = EDGE_LOOP ( 'NONE', ( #7367, #20396 ) ) ;
#11132 = DIRECTION ( 'NONE',  ( -0.000000000000000000, -0.000000000000000000, 1.000000000000000000 ) ) ;
#11131 = CARTESIAN_POINT ( 'NONE',  ( -18.12326418384769866, 12.88339258814709964, -19.04514329360673486 ) ) ;
#11133 = CARTESIAN_POINT ( 'NONE',  ( 2.229431105722923245, 20.49260818092372460, 12.00000000000000000 ) ) ;
#11134 = ADVANCED_FACE ( 'NONE', ( #20854 ), #8455, .F. ) ;
#11135 = AXIS2_PLACEMENT_3D ( 'NONE', #34528, #22722, #18889 ) ;
#11136 = CARTESIAN_POINT ( 'NONE',  ( 9.550008964001319711, -18.19057619834521233, -28.70580708904410372 ) ) ;
#11137 = CARTESIAN_POINT ( 'NONE',  ( -14.06009009443818591, 27.59413131461144530, 10.76099332938163400 ) ) ;
#11138 = CARTESIAN_POINT ( 'NONE',  ( 14.82211149595034350, 25.66540809471278806, -10.17682616307655330 ) ) ;
#11139 = CARTESIAN_POINT ( 'NONE',  ( -14.97283170755581061, 21.46414480565966798, 10.49999999999999822 ) ) ;
#11140 = DIRECTION ( 'NONE',  ( -0.4067366430757888285, 0.9135454576426059736, 0.000000000000000000 ) ) ;
#11141 = EDGE_CURVE ( 'NONE', #13470, #5684, #20653, .T. ) ;
#11142 = CARTESIAN_POINT ( 'NONE',  ( -27.75902213711245636, -24.56286694941507420, -7.146441665128197229 ) ) ;
#11143 = CARTESIAN_POINT ( 'NONE',  ( 3.937535457903849068, -24.55738665131292819, -8.888856001756707315 ) ) ;
#11144 = CARTESIAN_POINT ( 'NONE',  ( 13.92524374386434971, 23.06449320611515574, -14.49605255741758114 ) ) ;
#11145 = CARTESIAN_POINT ( 'NONE',  ( 17.26157349013544007, 11.42543953884226759, -26.61627152139759289 ) ) ;
#11146 = EDGE_LOOP ( 'NONE', ( #4276, #8949, #39370, #33080, #35088, #39282, #34136 ) ) ;
#11147 = CARTESIAN_POINT ( 'NONE',  ( -6.310829074464455068, 36.59364124554614506, -7.568975181432845645 ) ) ;
#11148 = ORIENTED_EDGE ( 'NONE', *, *, #31759, .F. ) ;
#11149 = AXIS2_PLACEMENT_3D ( 'NONE', #38749, #10718, #32667 ) ;
#11150 = CARTESIAN_POINT ( 'NONE',  ( 14.52509594610761745, 21.97885917798724265, 10.49999999999999822 ) ) ;
#11151 = EDGE_LOOP ( 'NONE', ( #38782, #22273, #19195 ) ) ;
#11152 = DIRECTION ( 'NONE',  ( -0.4067366430757884399, 0.9135454576426061957, 1.734723475976807410E-14 ) ) ;
#11153 = CARTESIAN_POINT ( 'NONE',  ( 9.126688212160850355, 10.78884215935634749, 10.87262190629280667 ) ) ;
#11154 = ORIENTED_EDGE ( 'NONE', *, *, #668, .T. ) ;
#11155 = CARTESIAN_POINT ( 'NONE',  ( -21.67682104884834970, 0.8966140999393611422, -23.87369810390991631 ) ) ;
#11156 = EDGE_CURVE ( 'NONE', #333, #10298, #23801, .T. ) ;
#11157 = VERTEX_POINT ( 'NONE', #5402 ) ;
#11158 = CARTESIAN_POINT ( 'NONE',  ( 20.35255112268399458, -5.483977284129752050, -26.39574775961089514 ) ) ;
#11159 = ADVANCED_FACE ( 'NONE', ( #26939 ), #1968, .T. ) ;
#11160 = ORIENTED_EDGE ( 'NONE', *, *, #18532, .F. ) ;
#11161 = VECTOR ( 'NONE', #18605, 1000.000000000000000 ) ;
#11162 = CYLINDRICAL_SURFACE ( 'NONE', #19335, 1.000000000000000000 ) ;
#11163 = VERTEX_POINT ( 'NONE', #30596 ) ;
#11164 = LINE ( 'NONE', #14410, #33957 ) ;
#11165 = DIRECTION ( 'NONE',  ( 0.000000000000000000, 0.000000000000000000, 1.000000000000000000 ) ) ;
#11166 = CARTESIAN_POINT ( 'NONE',  ( 4.383143208095032328, 35.51174355874288580, 18.42518152272108978 ) ) ;
#11167 = CARTESIAN_POINT ( 'NONE',  ( 0.000000000000000000, 22.50000000000000355, 7.000000000000000000 ) ) ;
#11168 = ORIENTED_EDGE ( 'NONE', *, *, #29443, .F. ) ;
#11169 = SURFACE_STYLE_USAGE ( .BOTH. , #36153 ) ;
#11170 = LINE ( 'NONE', #4670, #15859 ) ;
#11171 = CARTESIAN_POINT ( 'NONE',  ( -1.000000000000000000, 37.00000000000000711, 10.49999999999999822 ) ) ;
#11172 = CARTESIAN_POINT ( 'NONE',  ( 1.078807199784882265, 27.41272755941693617, 23.00000000000000355 ) ) ;
#11173 = EDGE_CURVE ( 'NONE', #32427, #40197, #10842, .T. ) ;
#11174 = CARTESIAN_POINT ( 'NONE',  ( 15.82467753361613205, 14.38668779758848082, -23.23502576981553602 ) ) ;
#11175 = CARTESIAN_POINT ( 'NONE',  ( 8.609117341516606459, 22.13848295504110197, -21.12116105944807032 ) ) ;
#11176 = VERTEX_POINT ( 'NONE', #17614 ) ;
#11177 = DIRECTION ( 'NONE',  ( 1.000000000000000000, 0.000000000000000000, 0.000000000000000000 ) ) ;
#11178 = AXIS2_PLACEMENT_3D ( 'NONE', #17335, #29710, #32975 ) ;
#11179 = CARTESIAN_POINT ( 'NONE',  ( -10.33795143809923367, 20.40792924032147226, 10.50000000000000000 ) ) ;
#11180 = EDGE_CURVE ( 'NONE', #34496, #20580, #8225, .T. ) ;
#11181 = CARTESIAN_POINT ( 'NONE',  ( 13.82053027212990592, -23.66662816038719441, -14.43394760191610615 ) ) ;
#11182 = CARTESIAN_POINT ( 'NONE',  ( 14.98890121934609532, -28.67928442654221044, -5.000000000000000000 ) ) ;
#11183 = LINE ( 'NONE', #23165, #26457 ) ;
#11184 = CARTESIAN_POINT ( 'NONE',  ( -15.29018876279933536, 26.53061139393243550, -7.357746246747966623 ) ) ;
#11185 = CARTESIAN_POINT ( 'NONE',  ( -34.11404923485120122, -2.099951938866391199, 14.53008259253964951 ) ) ;
#11186 = CARTESIAN_POINT ( 'NONE',  ( 9.552484026374298054, -19.39438616658035031, -23.93357300817531552 ) ) ;
#11187 = AXIS2_PLACEMENT_3D ( 'NONE', #28679, #7546, #38230 ) ;
#11188 = CARTESIAN_POINT ( 'NONE',  ( -15.00000000000000000, 22.50000000000000355, 7.000000000000000000 ) ) ;
#11189 = ORIENTED_EDGE ( 'NONE', *, *, #19932, .F. ) ;
#11190 = B_SPLINE_CURVE_WITH_KNOTS ( 'NONE', 3,
 ( #6462, #31652, #6656, #13360, #22496, #35102 ),
 .UNSPECIFIED., .F., .F.,
 ( 4, 2, 4 ),
 ( 0.000000000000000000, 0.4999999999999988898, 1.000000000000000000 ),
 .UNSPECIFIED. ) ;
#11191 = ORIENTED_EDGE ( 'NONE', *, *, #14228, .T. ) ;
#11192 = CARTESIAN_POINT ( 'NONE',  ( -11.39446229461578852, 31.55080954265326199, -9.887314613259318818 ) ) ;
#11193 = FACE_OUTER_BOUND ( 'NONE', #14604, .T. ) ;
#11194 = FACE_BOUND ( 'NONE', #38576, .T. ) ;
#11195 = VECTOR ( 'NONE', #6381, 1000.000000000000114 ) ;
#11196 = CARTESIAN_POINT ( 'NONE',  ( -34.33172124301603390, -5.488825450266375583, -6.338420623816570121 ) ) ;
#11197 = DIRECTION ( 'NONE',  ( 1.000000000000000000, 0.000000000000000000, 0.000000000000000000 ) ) ;
#11198 = ORIENTED_EDGE ( 'NONE', *, *, #39945, .F. ) ;
#11199 = CARTESIAN_POINT ( 'NONE',  ( 21.69624659619600138, 0.7958053819504173898, -23.86200436752996623 ) ) ;
#11200 = CARTESIAN_POINT ( 'NONE',  ( 11.30412111481574655, 32.00546000420950321, 10.94611345180491035 ) ) ;
#11201 = CARTESIAN_POINT ( 'NONE',  ( 9.892954722048896699, 20.95745441963929423, 10.50000000000000533 ) ) ;
#11202 = CARTESIAN_POINT ( 'NONE',  ( -2.623829155769458410, 7.750987179268020277, 10.68306085400110739 ) ) ;
#11203 = ORIENTED_EDGE ( 'NONE', *, *, #14245, .F. ) ;
#11204 = CARTESIAN_POINT ( 'NONE',  ( -29.57198801820384659, 0.07677956331076821184, -10.18105163486785436 ) ) ;
#11205 = B_SPLINE_CURVE_WITH_KNOTS ( 'NONE', 3,
 ( #14940, #15331, #23880, #17998, #5790, #2551 ),
 .UNSPECIFIED., .F., .F.,
 ( 4, 2, 4 ),
 ( 0.000000000000000000, 0.5000000000000000000, 1.000000000000000000 ),
 .UNSPECIFIED. ) ;
#11206 = FACE_OUTER_BOUND ( 'NONE', #22661, .T. ) ;
#11207 = ORIENTED_EDGE ( 'NONE', *, *, #7603, .T. ) ;
#11208 = CARTESIAN_POINT ( 'NONE',  ( 33.62952761534187118, -5.089175442527881899, -8.119193510173552397 ) ) ;
#11209 = CARTESIAN_POINT ( 'NONE',  ( 33.53425769460820050, -2.462485423393242279, 15.72805884748974847 ) ) ;
#11210 = ORIENTED_EDGE ( 'NONE', *, *, #1106, .T. ) ;
#11211 = CARTESIAN_POINT ( 'NONE',  ( -16.52773037515743226, 27.09393310379821074, 14.53008259254011136 ) ) ;
#11212 = ADVANCED_FACE ( 'NONE', ( #2162 ), #39725, .T. ) ;
#11213 = CARTESIAN_POINT ( 'NONE',  ( 4.272934335498898793E-14, -24.78318996519343997, 16.30093088680190760 ) ) ;
#11214 = CARTESIAN_POINT ( 'NONE',  ( 15.41558956984165363, 26.78481017248027740, -5.000000000000000000 ) ) ;
#11215 = CARTESIAN_POINT ( 'NONE',  ( 6.839309919355001988, 27.13928353713056651, 20.69868183039781684 ) ) ;
#11216 = CIRCLE ( 'NONE', #37163, 16.00000000000000000 ) ;
#11217 = LINE ( 'NONE', #33563, #10315 ) ;
#11218 = ORIENTED_EDGE ( 'NONE', *, *, #36845, .F. ) ;
#11219 = DIRECTION ( 'NONE',  ( 0.5254827454987502922, -0.4731467892558335331, -0.7071067811865415775 ) ) ;
#11220 = AXIS2_PLACEMENT_3D ( 'NONE', #12990, #611, #6886 ) ;
#11221 = CARTESIAN_POINT ( 'NONE',  ( -7.852079885517520452, 9.718707764022953555, 7.203056206335834766 ) ) ;
#11222 = CARTESIAN_POINT ( 'NONE',  ( 2.056640691923211417, 20.39672081104026802, -30.00000000000001066 ) ) ;
#11223 = DIRECTION ( 'NONE',  ( 0.000000000000000000, 0.000000000000000000, -1.000000000000000000 ) ) ;
#11224 = CARTESIAN_POINT ( 'NONE',  ( 7.205739717458053306, 18.19477196579531153, 20.99999999999999645 ) ) ;
#11225 = CARTESIAN_POINT ( 'NONE',  ( 14.71739798221114626, -19.47888500857317240, -20.11316221547454219 ) ) ;
#11226 = DIRECTION ( 'NONE',  ( 0.000000000000000000, 0.000000000000000000, 1.000000000000000000 ) ) ;
#11227 = CARTESIAN_POINT ( 'NONE',  ( -13.24038105676666710, 15.43301270189238394, 10.59344438985530878 ) ) ;
#11228 = CARTESIAN_POINT ( 'NONE',  ( -9.356056665764024061, 26.06569820189715259, 10.49999999999999112 ) ) ;
#11229 = VERTEX_POINT ( 'NONE', #39122 ) ;
#11230 = CIRCLE ( 'NONE', #843, 1.000000000000000000 ) ;
#11231 = CARTESIAN_POINT ( 'NONE',  ( 11.09749326504985056, 17.81885627187519816, -26.21546615232898958 ) ) ;
#11232 = ORIENTED_EDGE ( 'NONE', *, *, #38535, .F. ) ;
#11233 = CARTESIAN_POINT ( 'NONE',  ( -15.21277803108789328, 25.35827226598801687, -9.246070508268418919 ) ) ;
#11234 = CARTESIAN_POINT ( 'NONE',  ( -32.58967084635843037, -11.00843821516755483, 18.87996532025856666 ) ) ;
#11235 = EDGE_CURVE ( 'NONE', #5911, #4096, #5001, .T. ) ;
#11236 = LINE ( 'NONE', #8181, #19858 ) ;
#11237 = CARTESIAN_POINT ( 'NONE',  ( 14.96898239447578760, 25.69415526101390057, -9.710597112631324634 ) ) ;
#11238 = ORIENTED_EDGE ( 'NONE', *, *, #19203, .T. ) ;
#11239 = CARTESIAN_POINT ( 'NONE',  ( 17.86600798541212143, -10.56832063488048945, -27.70419187582904641 ) ) ;
#11240 = ORIENTED_EDGE ( 'NONE', *, *, #27021, .T. ) ;
#11242 = DIRECTION ( 'NONE',  ( 1.000000000000000000, 0.000000000000000000, 0.000000000000000000 ) ) ;
#11241 = CARTESIAN_POINT ( 'NONE',  ( -10.58469681223512637, 17.55611623359288131, -29.33974004713073214 ) ) ;
#11243 = CARTESIAN_POINT ( 'NONE',  ( -10.63103180431346395, -17.81178731582381403, -27.37356996827503863 ) ) ;
#11244 = CARTESIAN_POINT ( 'NONE',  ( 9.293999462566146619, 11.53598992149257008, 13.00000000000000178 ) ) ;
#11245 = CIRCLE ( 'NONE', #22236, 0.5000000000000004441 ) ;
#11246 = ORIENTED_EDGE ( 'NONE', *, *, #32881, .F. ) ;
#11247 = CARTESIAN_POINT ( 'NONE',  ( -28.92757974739110693, -10.91245307248345853, -14.78116652952236443 ) ) ;
#11248 = CARTESIAN_POINT ( 'NONE',  ( -14.83165383358532452, -26.38547499157037990, -7.359629187061518252 ) ) ;
#11249 = CARTESIAN_POINT ( 'NONE',  ( 12.14716901145161643, 12.46304090461738667, 6.000000000000000000 ) ) ;
#11250 = VERTEX_POINT ( 'NONE', #39328 ) ;
#11251 = CARTESIAN_POINT ( 'NONE',  ( 27.31176527514317343, 2.051244179470905760, -11.67027739895878646 ) ) ;
#11252 = CARTESIAN_POINT ( 'NONE',  ( -7.713869163866016621, 10.18146832927085121, 10.49999999999999822 ) ) ;
#11253 = AXIS2_PLACEMENT_3D ( 'NONE', #9038, #21422, #5977 ) ;
#11254 = CARTESIAN_POINT ( 'NONE',  ( -39.51968005974920572, -13.07391886567259576, 22.99999999999999289 ) ) ;
#11255 = ORIENTED_EDGE ( 'NONE', *, *, #19815, .T. ) ;
#11256 = CARTESIAN_POINT ( 'NONE',  ( -30.71039170661696716, -0.1163676949505514646, -7.354338998695498120 ) ) ;
#11257 = CARTESIAN_POINT ( 'NONE',  ( 31.58308575085905190, -0.9855460381432907813, -6.862365370586210211 ) ) ;
#11258 = AXIS2_PLACEMENT_3D ( 'NONE', #6893, #16050, #24996 ) ;
#11259 = CARTESIAN_POINT ( 'NONE',  ( 31.21198460772024674, -5.568619476414755631, 18.87996532025785967 ) ) ;
#11260 = EDGE_CURVE ( 'NONE', #5091, #23135, #17412, .T. ) ;
#11261 = ORIENTED_EDGE ( 'NONE', *, *, #575, .T. ) ;
#11262 = CARTESIAN_POINT ( 'NONE',  ( -29.11873305926894417, 1.737964268060802953, -6.420677056849690700 ) ) ;
#11263 = CARTESIAN_POINT ( 'NONE',  ( 17.34253826539385201, 27.32041144647958575, -5.000000000000000000 ) ) ;
#11264 = AXIS2_PLACEMENT_3D ( 'NONE', #11478, #20426, #14320 ) ;
#11265 = FACE_OUTER_BOUND ( 'NONE', #5379, .T. ) ;
#11266 = CLOSED_SHELL ( 'NONE', ( #32511, #27404, #33361, #39597, #3196, #28429, #286, #2573, #10245, #13818, #39785, #24293, #12740, #20490, #13362, #36345, #14309, #24138, #10824, #30987, #24396, #33386, #22885, #9298, #36994, #37308, #10367, #35893, #23208, #9613, #25246, #16383, #16718, #17622, #32763, #37083, #1609, #6655, #38946, #319, #3655, #15061, #10395, #3957, #11159, #13101, #13671, #26772, #3360 ) ) ;
#11267 = DIRECTION ( 'NONE',  ( 0.000000000000000000, 0.000000000000000000, 1.000000000000000000 ) ) ;
#11268 = ADVANCED_FACE ( 'NONE', ( #8652 ), #23688, .F. ) ;
#11269 = EDGE_CURVE ( 'NONE', #39078, #34288, #32895, .T. ) ;
#11270 = ADVANCED_FACE ( 'NONE', ( #33454 ), #5598, .T. ) ;
#11271 = AXIS2_PLACEMENT_3D ( 'NONE', #20073, #13761, #1992 ) ;
#11272 = DIRECTION ( 'NONE',  ( -0.7032331762534076436, 0.07391278520357413839, -0.7071067811865433539 ) ) ;
#11273 = CARTESIAN_POINT ( 'NONE',  ( -10.49474413300070097, 21.89971208337388120, 10.00000000000000000 ) ) ;
#11274 = DIRECTION ( 'NONE',  ( 0.5773502691896257311, -0.5773502691896217343, 0.5773502691896298389 ) ) ;
#11275 = ORIENTED_EDGE ( 'NONE', *, *, #4816, .F. ) ;
#11276 = CARTESIAN_POINT ( 'NONE',  ( -20.12887129416308696, 5.733943412042154186, -25.39721956534479119 ) ) ;
#11277 = DIRECTION ( 'NONE',  ( 0.000000000000000000, 0.000000000000000000, 1.000000000000000000 ) ) ;
#11278 = DIRECTION ( 'NONE',  ( 1.000000000000000000, 0.000000000000000000, 0.000000000000000000 ) ) ;
#11279 = CARTESIAN_POINT ( 'NONE',  ( 15.24725239375168329, -14.05410354436919285, -27.77140347803001319 ) ) ;
#11280 = FACE_OUTER_BOUND ( 'NONE', #5385, .T. ) ;
#11281 = DIRECTION ( 'NONE',  ( 1.000000000000000000, 0.000000000000000000, 0.000000000000000000 ) ) ;
#11282 = B_SPLINE_CURVE_WITH_KNOTS ( 'NONE', 3,
 ( #35360, #1432, #17691, #7920, #23765, #8120 ),
 .UNSPECIFIED., .F., .F.,
 ( 4, 2, 4 ),
 ( 0.000000000000000000, 0.5000000000000000000, 1.000000000000000000 ),
 .UNSPECIFIED. ) ;
#11283 = CARTESIAN_POINT ( 'NONE',  ( 14.98650480333069979, 26.50796964270606537, -8.751387093918793880 ) ) ;
#11284 = DIRECTION ( 'NONE',  ( -0.000000000000000000, -0.000000000000000000, -1.000000000000000000 ) ) ;
#11285 = EDGE_LOOP ( 'NONE', ( #14139, #39230, #3374 ) ) ;
#11286 = VECTOR ( 'NONE', #34098, 1000.000000000000000 ) ;
#11287 = CARTESIAN_POINT ( 'NONE',  ( -14.96418064126415715, 20.04621382461933976, -15.64591645429735678 ) ) ;
#11288 = ADVANCED_FACE ( 'NONE', ( #31573 ), #27930, .T. ) ;
#11289 = CARTESIAN_POINT ( 'NONE',  ( -24.05659981020947669, -7.641904207658729575, 20.99999999999999645 ) ) ;
#11290 = ADVANCED_FACE ( 'NONE', ( #3739 ), #6778, .T. ) ;
#11291 = EDGE_CURVE ( 'NONE', #25337, #11380, #12148, .T. ) ;
#11292 = CARTESIAN_POINT ( 'NONE',  ( -7.064571727552472424, 31.45661825943146894, 6.000000000000000000 ) ) ;
#11293 = CARTESIAN_POINT ( 'NONE',  ( 11.49255140715953338, 18.43021842612911598, -23.85520735916814772 ) ) ;
#11294 = VERTEX_POINT ( 'NONE', #25469 ) ;
#11295 = LINE ( 'NONE', #20437, #26106 ) ;
#11296 = ORIENTED_EDGE ( 'NONE', *, *, #24342, .F. ) ;
#11298 = CARTESIAN_POINT ( 'NONE',  ( 11.44134295108989186, 15.31698729810772797, 10.00000000000000000 ) ) ;
#11297 = CARTESIAN_POINT ( 'NONE',  ( -14.97507841241774784, 26.10841250006580339, -9.231366820537651563 ) ) ;
#11299 = CARTESIAN_POINT ( 'NONE',  ( -14.99851249572590106, -25.99467288956163813, -9.237413589426980209 ) ) ;
#11300 = CARTESIAN_POINT ( 'NONE',  ( -28.24711154207077257, -27.09388640670392689, 11.55979286843935050 ) ) ;
#11301 = CARTESIAN_POINT ( 'NONE',  ( -33.71484418225002599, -17.65950029506896612, -7.118567158664396821 ) ) ;
#11302 = VECTOR ( 'NONE', #20775, 1000.000000000000000 ) ;
#11303 = CARTESIAN_POINT ( 'NONE',  ( -6.123308122133267695, -19.62006737319780569, -29.40205820084093702 ) ) ;
#11304 = CARTESIAN_POINT ( 'NONE',  ( 14.78937771930062262, 23.24318486792957117, -12.59837077348300660 ) ) ;
#11305 = ORIENTED_EDGE ( 'NONE', *, *, #16868, .T. ) ;
#11306 = CARTESIAN_POINT ( 'NONE',  ( 24.38209929399536335, 7.347059586047067548, -8.383116823341570267 ) ) ;
#11307 = DIRECTION ( 'NONE',  ( -0.2079116908177664480, -0.9781476007338042455, 0.000000000000000000 ) ) ;
#11308 = DIRECTION ( 'NONE',  ( 0.000000000000000000, 0.000000000000000000, -1.000000000000000000 ) ) ;
#11309 = CARTESIAN_POINT ( 'NONE',  ( -14.84160187385925589, 20.32586711127000711, 7.500000000000004441 ) ) ;
#11310 = ORIENTED_EDGE ( 'NONE', *, *, #7647, .T. ) ;
#11311 = CARTESIAN_POINT ( 'NONE',  ( -32.95954470968036532, -2.553576478305152886, -5.000000000000000000 ) ) ;
#11312 = CARTESIAN_POINT ( 'NONE',  ( 28.35484778630695502, 0.1198746217886747789, -12.54935875910663157 ) ) ;
#11313 = FACE_OUTER_BOUND ( 'NONE', #36772, .T. ) ;
#11314 = CARTESIAN_POINT ( 'NONE',  ( 17.62780868050626637, -18.45076755199313112, 20.82122704794080192 ) ) ;
#11315 = DIRECTION ( 'NONE',  ( 1.000000000000000000, 0.000000000000000000, 0.000000000000000000 ) ) ;
#11316 = EDGE_CURVE ( 'NONE', #33425, #1690, #11480, .T. ) ;
#11317 = DIRECTION ( 'NONE',  ( -0.8090169943749504489, -0.5877852522924689183, 0.000000000000000000 ) ) ;
#11318 = CARTESIAN_POINT ( 'NONE',  ( 32.33143948541780333, 1.358872982501766025, 11.00000000000000000 ) ) ;
#11319 = AXIS2_PLACEMENT_3D ( 'NONE', #29595, #28993, #35090 ) ;
#11320 = VERTEX_POINT ( 'NONE', #3151 ) ;
#11321 = CARTESIAN_POINT ( 'NONE',  ( -1.853172919594719970, 21.57294901687549427, 12.00000000000000000 ) ) ;
#11322 = CARTESIAN_POINT ( 'NONE',  ( 6.546529844545025512, 35.97445010452246805, 10.68306085400100791 ) ) ;
#11323 = DIRECTION ( 'NONE',  ( 0.8660254037844431485, 0.4999999999999921174, 0.000000000000000000 ) ) ;
#11324 = AXIS2_PLACEMENT_3D ( 'NONE', #382, #9920, #25155 ) ;
#11325 = CARTESIAN_POINT ( 'NONE',  ( 0.8578242162873520593, 21.13533821733210871, -26.25769815819063524 ) ) ;
#11326 = CARTESIAN_POINT ( 'NONE',  ( -18.00000000000003197, 22.50000000000001066, 3.000000000000000000 ) ) ;
#11327 = FACE_OUTER_BOUND ( 'NONE', #35999, .T. ) ;
#11328 = DIRECTION ( 'NONE',  ( 1.000000000000000000, 0.000000000000000000, 0.000000000000000000 ) ) ;
#11329 = CARTESIAN_POINT ( 'NONE',  ( 10.06946225350410984, 32.23940090176269990, 7.499999999999996447 ) ) ;
#11330 = CARTESIAN_POINT ( 'NONE',  ( -14.48927117870122316, -30.61587158504648087, 11.00000000000000000 ) ) ;
#11331 = AXIS2_PLACEMENT_3D ( 'NONE', #2441, #21716, #24572 ) ;
#11332 = CARTESIAN_POINT ( 'NONE',  ( 14.30190381450494286, 27.90070721307182566, -9.148110432232169131 ) ) ;
#11333 = CARTESIAN_POINT ( 'NONE',  ( -12.99377146717201192, 26.19620116591435277, 10.50000000000000000 ) ) ;
#11334 = ORIENTED_EDGE ( 'NONE', *, *, #16593, .T. ) ;
#11336 = CARTESIAN_POINT ( 'NONE',  ( -3.784955426773653375, 9.502919080911414795, 9.500000000000000000 ) ) ;
#11335 = CARTESIAN_POINT ( 'NONE',  ( -18.85571089263951450, 16.25964530329961022, -9.864473642832360056 ) ) ;
#11337 = CARTESIAN_POINT ( 'NONE',  ( -1.000000000000000444, 37.04625217320466390, 10.49999999999999822 ) ) ;
#11338 = CARTESIAN_POINT ( 'NONE',  ( 15.10121951614408253, -26.15095910722338601, -8.766956026588630380 ) ) ;
#11339 = EDGE_CURVE ( 'NONE', #24976, #13129, #6339, .T. ) ;
#11340 = DIRECTION ( 'NONE',  ( 1.000000000000000000, 0.000000000000000000, 0.000000000000000000 ) ) ;
#11341 = CARTESIAN_POINT ( 'NONE',  ( 15.00671440964051939, 26.00632701074570008, -9.236423267190737363 ) ) ;
#11342 = CARTESIAN_POINT ( 'NONE',  ( 12.05832241004688399, 18.99596958976722760, -30.00000000000000000 ) ) ;
#11343 = CARTESIAN_POINT ( 'NONE',  ( -0.5000000000000004441, 32.50000000000000000, 10.50000000000000000 ) ) ;
#11344 = EDGE_CURVE ( 'NONE', #31717, #2452, #18988, .T. ) ;
#11345 = AXIS2_PLACEMENT_3D ( 'NONE', #38080, #10055, #7399 ) ;
#11346 = CARTESIAN_POINT ( 'NONE',  ( -24.87365189169005575, -23.40965842456435908, -11.14002769881621724 ) ) ;
#11347 = CARTESIAN_POINT ( 'NONE',  ( 2.790632566740769871, -20.50748363971857913, -27.16196803510360169 ) ) ;
#11348 = CARTESIAN_POINT ( 'NONE',  ( 14.67493102267895466, 24.58460314029640159, -11.61047959535504148 ) ) ;
#11349 = CARTESIAN_POINT ( 'NONE',  ( 19.59303125460614226, 10.94001574543910138, -18.02074012208363385 ) ) ;
#11350 = CYLINDRICAL_SURFACE ( 'NONE', #21879, 0.4999999999999998890 ) ;
#11351 = ORIENTED_EDGE ( 'NONE', *, *, #7561, .T. ) ;
#11352 = CARTESIAN_POINT ( 'NONE',  ( -4.809622099922509442, 20.53902726650351340, -26.36567314579518850 ) ) ;
#11353 = ORIENTED_EDGE ( 'NONE', *, *, #22386, .F. ) ;
#11354 = CARTESIAN_POINT ( 'NONE',  ( 5.023113021171168313, 36.63452954033265030, 7.203056206335840095 ) ) ;
#11355 = ORIENTED_EDGE ( 'NONE', *, *, #33008, .T. ) ;
#11356 = LINE ( 'NONE', #30040, #7035 ) ;
#11357 = CARTESIAN_POINT ( 'NONE',  ( 1.278175571583998194, 14.08178954835375940, 9.000000000000001776 ) ) ;
#11358 = ORIENTED_EDGE ( 'NONE', *, *, #31257, .F. ) ;
#11359 = CARTESIAN_POINT ( 'NONE',  ( -23.26829119944321178, 0.6879608890881370176, -20.55845448473494486 ) ) ;
#11360 = EDGE_CURVE ( 'NONE', #25659, #25600, #30099, .T. ) ;
#11361 = ORIENTED_EDGE ( 'NONE', *, *, #17569, .T. ) ;
#11362 = CARTESIAN_POINT ( 'NONE',  ( 31.86584383545969246, -10.62267807593470259, -12.03292509902580854 ) ) ;
#11363 = AXIS2_PLACEMENT_3D ( 'NONE', #1593, #7875, #17244 ) ;
#11364 = EDGE_CURVE ( 'NONE', #20973, #16864, #106, .T. ) ;
#11365 = EDGE_LOOP ( 'NONE', ( #30741, #30918, #2060, #29849 ) ) ;
#11366 = CARTESIAN_POINT ( 'NONE',  ( 10.62305557349671403, 33.09035064698313278, 7.455686640544900712 ) ) ;
#11367 = ORIENTED_EDGE ( 'NONE', *, *, #21444, .F. ) ;
#11368 = DIRECTION ( 'NONE',  ( 0.000000000000000000, 0.000000000000000000, 1.000000000000000000 ) ) ;
#11369 = DIRECTION ( 'NONE',  ( 0.000000000000000000, 0.000000000000000000, -1.000000000000000000 ) ) ;
#11370 = AXIS2_PLACEMENT_3D ( 'NONE', #9071, #8267, #6011 ) ;
#11371 = ADVANCED_FACE ( 'NONE', ( #19180 ), #16141, .T. ) ;
#11372 = DIRECTION ( 'NONE',  ( 0.000000000000000000, 0.000000000000000000, 1.000000000000000000 ) ) ;
#11373 = ORIENTED_EDGE ( 'NONE', *, *, #21338, .T. ) ;
#11374 = SURFACE_STYLE_FILL_AREA ( #5070 ) ;
#11375 = CARTESIAN_POINT ( 'NONE',  ( -23.05386822411323422, -7.747535282638357224, 20.99999999999999645 ) ) ;
#11376 = CYLINDRICAL_SURFACE ( 'NONE', #15027, 20.00000000000002487 ) ;
#11377 = CARTESIAN_POINT ( 'NONE',  ( 10.16122020288883299, 33.53402030034401804, 7.000000000000000000 ) ) ;
#11378 = CARTESIAN_POINT ( 'NONE',  ( 18.58187274253394605, 17.94739436884781369, -5.960075704151572396 ) ) ;
#11379 = CARTESIAN_POINT ( 'NONE',  ( 7.608710298680324335, 19.37355573834689437, -27.20130433680634141 ) ) ;
#11380 = VERTEX_POINT ( 'NONE', #5991 ) ;
#11381 = DIRECTION ( 'NONE',  ( -0.8090169943749503378, -0.5877852522924691403, 0.000000000000000000 ) ) ;
#11382 = FACE_OUTER_BOUND ( 'NONE', #19042, .T. ) ;
#11383 = CARTESIAN_POINT ( 'NONE',  ( 12.48110824329010171, -22.01890908291360205, -17.41505214487477105 ) ) ;
#11384 = DIRECTION ( 'NONE',  ( 0.000000000000000000, 0.000000000000000000, 1.000000000000000000 ) ) ;
#11385 = EDGE_CURVE ( 'NONE', #17600, #35419, #18398, .T. ) ;
#11386 = EDGE_CURVE ( 'NONE', #33800, #14056, #27054, .T. ) ;
#11387 = DIRECTION ( 'NONE',  ( 0.000000000000000000, 0.000000000000000000, 1.000000000000000000 ) ) ;
#11388 = ADVANCED_FACE ( 'NONE', ( #21831 ), #12489, .T. ) ;
#11389 = CARTESIAN_POINT ( 'NONE',  ( -14.53044073688932869, 24.97606202870426628, -11.59869272441059174 ) ) ;
#11390 = CARTESIAN_POINT ( 'NONE',  ( -31.99827245169854706, -22.69195664478721142, 15.13084544680206811 ) ) ;
#11391 = CARTESIAN_POINT ( 'NONE',  ( 9.824869631482991750, -19.77893024222395368, -22.81952676811747693 ) ) ;
#11392 = DIRECTION ( 'NONE',  ( 0.000000000000000000, 0.000000000000000000, 1.000000000000000000 ) ) ;
#11393 = ORIENTED_EDGE ( 'NONE', *, *, #7509, .F. ) ;
#11394 = VERTEX_POINT ( 'NONE', #22032 ) ;
#11395 = CARTESIAN_POINT ( 'NONE',  ( -11.90375846996125020, 33.19065507634929446, -5.000000000000001776 ) ) ;
#11396 = VECTOR ( 'NONE', #38912, 1000.000000000000000 ) ;
#11397 = CARTESIAN_POINT ( 'NONE',  ( 13.03640989728592459, 29.14264673470096767, 12.00000000000000000 ) ) ;
#11398 = DIRECTION ( 'NONE',  ( 0.000000000000000000, 0.000000000000000000, 1.000000000000000000 ) ) ;
#11399 = CIRCLE ( 'NONE', #23045, 1.000000000000000888 ) ;
#11400 = CARTESIAN_POINT ( 'NONE',  ( 0.5000000000000002220, 36.00000000000000711, 10.50000000000000000 ) ) ;
#11401 = VERTEX_POINT ( 'NONE', #34235 ) ;
#11402 = CARTESIAN_POINT ( 'NONE',  ( 20.81180504415543808, 0.8748342307719589872, -26.83400273307002237 ) ) ;
#11403 = LINE ( 'NONE', #30085, #20667 ) ;
#11404 = LINE ( 'NONE', #35585, #3809 ) ;
#11405 = CARTESIAN_POINT ( 'NONE',  ( -36.71098721002695697, -16.64818343423248237, 11.00000000000018829 ) ) ;
#11406 = VERTEX_POINT ( 'NONE', #6386 ) ;
#11407 = CARTESIAN_POINT ( 'NONE',  ( -27.72708288707136148, 0.2041362863144290662, -13.51430501883785595 ) ) ;
#11408 = CARTESIAN_POINT ( 'NONE',  ( -5.459721035624959029, 35.99203088905950665, 10.99999999999999289 ) ) ;
#11409 = ADVANCED_FACE ( 'NONE', ( #31181 ), #23157, .T. ) ;
#11410 = VERTEX_POINT ( 'NONE', #15739 ) ;
#11411 = CARTESIAN_POINT ( 'NONE',  ( 20.84830255071761584, -2.293361874497828357, -26.59171325517713669 ) ) ;
#11412 = CARTESIAN_POINT ( 'NONE',  ( 35.63595018118459734, -14.50160624002288579, 15.72805884748939853 ) ) ;
#11413 = EDGE_CURVE ( 'NONE', #33916, #37897, #15941, .T. ) ;
#11414 = ORIENTED_EDGE ( 'NONE', *, *, #3666, .F. ) ;
#11415 = CARTESIAN_POINT ( 'NONE',  ( 9.055806345856177941, 37.53717483670233435, 13.92931973827812620 ) ) ;
#11416 = CARTESIAN_POINT ( 'NONE',  ( -5.594491472541998967, -20.30912387778604966, 19.66345542862528717 ) ) ;
#11417 = CARTESIAN_POINT ( 'NONE',  ( -26.35691893567060617, -28.22903657647675857, -5.000000000000004441 ) ) ;
#11418 = CARTESIAN_POINT ( 'NONE',  ( -6.337046384719310588, 27.87972889837504553, 20.69868183039780263 ) ) ;
#11419 = DIRECTION ( 'NONE',  ( 1.000000000000000000, 0.000000000000000000, 0.000000000000000000 ) ) ;
#11420 = ORIENTED_EDGE ( 'NONE', *, *, #12085, .F. ) ;
#11421 = DIRECTION ( 'NONE',  ( 1.000000000000000000, 0.000000000000000000, 0.000000000000000000 ) ) ;
#11422 = B_SPLINE_CURVE_WITH_KNOTS ( 'NONE', 3,
 ( #34456, #11430, #33376, #26456, #2285, #29708, #27260, #1891, #30114, #36215, #20970, #14675, #17334, #27064, #14269, #5325, #11630, #17933 ),
 .UNSPECIFIED., .F., .F.,
 ( 4, 2, 2, 2, 2, 2, 2, 2, 4 ),
 ( 0.000000000000000000, 0.1250000000000001388, 0.2500000000000001665, 0.3750000000000001665, 0.5000000000000002220, 0.6250000000000002220, 0.7500000000000001110, 0.8750000000000001110, 1.000000000000000000 ),
 .UNSPECIFIED. ) ;
#11423 = AXIS2_PLACEMENT_3D ( 'NONE', #10833, #1900, #20180 ) ;
#11424 = VECTOR ( 'NONE', #36261, 1000.000000000000000 ) ;
#11425 = CARTESIAN_POINT ( 'NONE',  ( 4.004005824709742534, 20.71913140499757588, -26.33338948413068792 ) ) ;
#11426 = CARTESIAN_POINT ( 'NONE',  ( 32.33143948541783885, 1.358872982501748927, -5.000000000000000000 ) ) ;
#11427 = CARTESIAN_POINT ( 'NONE',  ( 20.38546294303163720, 5.309590202429361305, 19.66345542862513796 ) ) ;
#11428 = AXIS2_PLACEMENT_3D ( 'NONE', #13367, #19663, #32057 ) ;
#11429 = CARTESIAN_POINT ( 'NONE',  ( 12.74496003955331602, -18.08351565856460041, -23.53601421872712862 ) ) ;
#11430 = CARTESIAN_POINT ( 'NONE',  ( -16.82090372984274396, 29.19711159930251299, 10.99999999999914913 ) ) ;
#11431 = CARTESIAN_POINT ( 'NONE',  ( -11.81630298851966288, 31.79381426990562787, 11.00000000000000000 ) ) ;
#11432 = CARTESIAN_POINT ( 'NONE',  ( 2.525645716490519277, 8.212903943950919938, 11.00000000000000355 ) ) ;
#11433 = ORIENTED_EDGE ( 'NONE', *, *, #28134, .T. ) ;
#11434 = CARTESIAN_POINT ( 'NONE',  ( 12.32426020000443678, 20.57966432427881287, -19.48222999790586130 ) ) ;
#11435 = ORIENTED_EDGE ( 'NONE', *, *, #30665, .T. ) ;
#11436 = CARTESIAN_POINT ( 'NONE',  ( -13.56937750933248843, 21.60099091529283655, -16.49869329321488465 ) ) ;
#11437 = CARTESIAN_POINT ( 'NONE',  ( -30.06493440560439012, -18.98646248983845553, 18.87996532025748664 ) ) ;
#11438 = CARTESIAN_POINT ( 'NONE',  ( -14.18553059334566591, 26.06413323176255759, 10.49999999999999822 ) ) ;
#11439 = CARTESIAN_POINT ( 'NONE',  ( 11.95881310940501052, 19.31147990981001428, -21.62860280665383428 ) ) ;
#11440 = VERTEX_POINT ( 'NONE', #7185 ) ;
#11441 = CARTESIAN_POINT ( 'NONE',  ( 18.61388091722034943, -11.78005302609667737, -24.22059683775887606 ) ) ;
#11442 = VERTEX_POINT ( 'NONE', #3941 ) ;
#11444 = CARTESIAN_POINT ( 'NONE',  ( 17.34253826607184479, 27.32041144404033162, 11.00000000000000000 ) ) ;
#11443 = CARTESIAN_POINT ( 'NONE',  ( -14.70800301661877363, 26.47766101481222378, -9.672390817437571897 ) ) ;
#11445 = CARTESIAN_POINT ( 'NONE',  ( -11.32445066732773142, -18.74575232930073554, -23.71343054792953708 ) ) ;
#11446 = CYLINDRICAL_SURFACE ( 'NONE', #2382, 0.4999999999999986122 ) ;
#11447 = EDGE_LOOP ( 'NONE', ( #10351, #8443, #25730, #9847 ) ) ;
#11448 = CARTESIAN_POINT ( 'NONE',  ( -26.01876133091875687, -8.953118292131030387, -17.69243264847248653 ) ) ;
#11449 = CARTESIAN_POINT ( 'NONE',  ( -11.44614701672549728, -21.52147791799877652, -18.49673592605288874 ) ) ;
#11450 = DIRECTION ( 'NONE',  ( -0.2079116908177663092, -0.9781476007338041345, 0.000000000000000000 ) ) ;
#11451 = ORIENTED_EDGE ( 'NONE', *, *, #33431, .T. ) ;
#11452 = CARTESIAN_POINT ( 'NONE',  ( 28.22673339625941935, 2.021307961998640490, -9.272653165744820569 ) ) ;
#11453 = CARTESIAN_POINT ( 'NONE',  ( -5.100643064501314328, 15.70406341247269211, 6.000000000000000000 ) ) ;
#11454 = LINE ( 'NONE', #27090, #12170 ) ;
#11455 = VECTOR ( 'NONE', #5482, 1000.000000000000000 ) ;
#11456 = ORIENTED_EDGE ( 'NONE', *, *, #12061, .T. ) ;
#11457 = CARTESIAN_POINT ( 'NONE',  ( -25.24992131713657884, 0.3092178984780983853, -17.42948113351768669 ) ) ;
#11458 = CARTESIAN_POINT ( 'NONE',  ( 32.12080372859628596, -1.419867088699604984, -5.000000000000000888 ) ) ;
#11459 = CIRCLE ( 'NONE', #19212, 1.000000000000000000 ) ;
#11460 = CARTESIAN_POINT ( 'NONE',  ( 20.42855823444378771, -24.24606183460743480, 18.87996532025784546 ) ) ;
#11461 = VECTOR ( 'NONE', #33834, 1000.000000000000000 ) ;
#11462 = ORIENTED_EDGE ( 'NONE', *, *, #14579, .F. ) ;
#11463 = CARTESIAN_POINT ( 'NONE',  ( -21.41754555983938602, 3.564190076994790068, -23.03422754373932335 ) ) ;
#11464 = DIRECTION ( 'NONE',  ( 1.000000000000000000, 0.000000000000000000, 0.000000000000000000 ) ) ;
#11465 = DIRECTION ( 'NONE',  ( 0.7071067811865451302, 8.659560562354889717E-17, 0.7071067811865500152 ) ) ;
#11466 = DIRECTION ( 'NONE',  ( -1.000000000000000000, 0.000000000000000000, 0.000000000000000000 ) ) ;
#11467 =( BOUNDED_CURVE ( )  B_SPLINE_CURVE ( 2, ( #13201, #12613, #37995 ),
 .UNSPECIFIED., .F., .F. ) 
 B_SPLINE_CURVE_WITH_KNOTS ( ( 3, 3 ),
 ( 0.000000000000000000, 1.000000000000000000 ),
 .UNSPECIFIED. ) 
 CURVE ( )  GEOMETRIC_REPRESENTATION_ITEM ( )  RATIONAL_B_SPLINE_CURVE ( ( 1.000000000000000000, 0.7071067811865474617, 1.000000000000000000 ) ) 
 REPRESENTATION_ITEM ( '' )  );
#11468 = DIRECTION ( 'NONE',  ( -0.000000000000000000, -0.000000000000000000, -1.000000000000000000 ) ) ;
#11469 = DIRECTION ( 'NONE',  ( 0.000000000000000000, 0.000000000000000000, 1.000000000000000000 ) ) ;
#11470 = B_SPLINE_CURVE_WITH_KNOTS ( 'NONE', 3,
 ( #3659, #31495, #22143, #34543, #9958, #6694 ),
 .UNSPECIFIED., .F., .F.,
 ( 4, 2, 4 ),
 ( 0.000000000000000000, 0.5000000000000000000, 1.000000000000000000 ),
 .UNSPECIFIED. ) ;
#11471 = LINE ( 'NONE', #24257, #29547 ) ;
#11472 = VERTEX_POINT ( 'NONE', #19380 ) ;
#11473 = CARTESIAN_POINT ( 'NONE',  ( -25.65838226093921648, 5.279357062076430296, -9.330829415115919900 ) ) ;
#11474 = CARTESIAN_POINT ( 'NONE',  ( -10.47804177580193041, 33.28010392086039815, 10.49999999999999822 ) ) ;
#11475 = CARTESIAN_POINT ( 'NONE',  ( -15.00309677617817883, 1.567672476163677109, 20.99999999999998934 ) ) ;
#11476 = CARTESIAN_POINT ( 'NONE',  ( 23.26876723194845908, -24.22783250195383076, -11.17799550874850567 ) ) ;
#11477 = CARTESIAN_POINT ( 'NONE',  ( 6.577540944421576441, 33.15743037285414374, 6.000000000000000000 ) ) ;
#11478 = CARTESIAN_POINT ( 'NONE',  ( -12.16658951415318768, 37.80625835076882879, 10.00000000000000000 ) ) ;
#11479 = CARTESIAN_POINT ( 'NONE',  ( 12.43688989749638907, 21.37114209746378179, -18.40534107864847968 ) ) ;
#11480 = CIRCLE ( 'NONE', #34189, 16.00000000000000000 ) ;
#11481 = CARTESIAN_POINT ( 'NONE',  ( 14.98890121934584663, -28.67928442654197951, 11.55979286843934872 ) ) ;
#11482 = VERTEX_POINT ( 'NONE', #16545 ) ;
#11484 = AXIS2_PLACEMENT_3D ( 'NONE', #37663, #10637, #7579 ) ;
#11483 = CARTESIAN_POINT ( 'NONE',  ( -13.41783481295519564, 15.62964107709064976, -28.19920321125439244 ) ) ;
#11485 = CARTESIAN_POINT ( 'NONE',  ( -18.03924190088572743, -16.85603499720482645, 20.99999999999999645 ) ) ;
#11486 = EDGE_CURVE ( 'NONE', #2306, #13272, #1506, .T. ) ;
#11487 = CARTESIAN_POINT ( 'NONE',  ( -7.659620408498105881, 26.92228390473685096, 9.000000000000001776 ) ) ;
#11488 = CARTESIAN_POINT ( 'NONE',  ( 11.50098969431590668, 18.42294700796338702, -23.85649179623154481 ) ) ;
#11489 = EDGE_LOOP ( 'NONE', ( #9232, #19628, #4016, #39870 ) ) ;
#11490 = CARTESIAN_POINT ( 'NONE',  ( 12.93090914344497122, 21.64873284080849203, -17.43820100889084657 ) ) ;
#11491 = EDGE_LOOP ( 'NONE', ( #27926, #8904, #39932, #33752, #32648, #17052, #19773 ) ) ;
#11493 = DIRECTION ( 'NONE',  ( -0.000000000000000000, -0.000000000000000000, -1.000000000000000000 ) ) ;
#11492 = CARTESIAN_POINT ( 'NONE',  ( -11.22930476693127311, 18.10080634600636529, -25.00346310164814767 ) ) ;
#11494 = CARTESIAN_POINT ( 'NONE',  ( -9.533178660976551200, -18.19926881236112592, -28.70647124653801896 ) ) ;
#11495 = CARTESIAN_POINT ( 'NONE',  ( 3.914034194965609892, 30.06176806842420035, 9.000000000000001776 ) ) ;
#11496 = CARTESIAN_POINT ( 'NONE',  ( -32.33767308879468771, -16.92829965255246449, -9.727596525381697390 ) ) ;
#11497 = CARTESIAN_POINT ( 'NONE',  ( -9.023319067658404080, -24.92662452266139184, -9.321921292790742442 ) ) ;
#11498 = DIRECTION ( 'NONE',  ( 1.000000000000000000, 0.000000000000000000, 0.000000000000000000 ) ) ;
#11499 = CARTESIAN_POINT ( 'NONE',  ( 12.21661684832558237, 18.39671740363510466, -22.81900652314237732 ) ) ;
#11500 = EDGE_CURVE ( 'NONE', #11836, #14093, #25673, .T. ) ;
#11501 = ORIENTED_EDGE ( 'NONE', *, *, #37687, .F. ) ;
#11502 = CARTESIAN_POINT ( 'NONE',  ( 20.02700736633234868, 6.692680301631161122, -24.33429107806700742 ) ) ;
#11503 = LINE ( 'NONE', #27336, #3093 ) ;
#11504 = CARTESIAN_POINT ( 'NONE',  ( 14.26584437371809777, 27.13525491562438319, 6.000000000000000000 ) ) ;
#11505 = EDGE_CURVE ( 'NONE', #38413, #8399, #10445, .T. ) ;
#11506 = DIRECTION ( 'NONE',  ( 1.000000000000000000, 0.000000000000000000, 0.000000000000000000 ) ) ;
#11507 = VERTEX_POINT ( 'NONE', #38070 ) ;
#11508 = CARTESIAN_POINT ( 'NONE',  ( -20.50243331965346627, -0.1390943044478715751, -29.32999314426240289 ) ) ;
#11509 = CARTESIAN_POINT ( 'NONE',  ( 20.48330953517068664, 0.8273339926270942835, -29.34778729633271510 ) ) ;
#11510 = DIRECTION ( 'NONE',  ( 1.000000000000000000, 0.000000000000000000, 0.000000000000000000 ) ) ;
#11511 = CARTESIAN_POINT ( 'NONE',  ( 22.30415078909558346, -16.34589999308455432, 20.99999999999995026 ) ) ;
#11512 = CARTESIAN_POINT ( 'NONE',  ( 3.863783140547853712E-14, -86.77689918168233874, -0.000000000000000000 ) ) ;
#11513 = DIRECTION ( 'NONE',  ( 0.000000000000000000, 0.000000000000000000, 1.000000000000000000 ) ) ;
#11514 = CARTESIAN_POINT ( 'NONE',  ( 37.58754968649115824, -10.91577297561518556, 10.99999999999992006 ) ) ;
#11515 = ADVANCED_FACE ( 'NONE', ( #26284 ), #22829, .F. ) ;
#11516 = ORIENTED_EDGE ( 'NONE', *, *, #37483, .T. ) ;
#11517 = EDGE_CURVE ( 'NONE', #7227, #13219, #10852, .T. ) ;
#11518 = FACE_OUTER_BOUND ( 'NONE', #29434, .T. ) ;
#11519 = AXIS2_PLACEMENT_3D ( 'NONE', #25885, #1315, #23043 ) ;
#11520 = AXIS2_PLACEMENT_3D ( 'NONE', #39549, #8475, #11725 ) ;
#11521 = CARTESIAN_POINT ( 'NONE',  ( -8.559512017365658920, 19.71884705062586107, 13.00000000000000178 ) ) ;
#11522 = CARTESIAN_POINT ( 'NONE',  ( -13.63581098909220479, 27.45627467658446008, 11.00000000000000000 ) ) ;
#11523 = CARTESIAN_POINT ( 'NONE',  ( 1.575354112968664566, 38.41398891768359647, -5.855932988374854098 ) ) ;
#11524 = LINE ( 'NONE', #11326, #8108 ) ;
#11525 = DIRECTION ( 'NONE',  ( -0.9510565162951507556, 0.3090169943749560000, 0.000000000000000000 ) ) ;
#11526 = CARTESIAN_POINT ( 'NONE',  ( 10.73859285986296541, 31.49625607628530588, 9.500000000000000000 ) ) ;
#11527 = DIRECTION ( 'NONE',  ( 0.000000000000000000, 0.000000000000000000, 1.000000000000000000 ) ) ;
#11528 = DIRECTION ( 'NONE',  ( 1.000000000000000000, 0.000000000000000000, 0.000000000000000000 ) ) ;
#11529 = CARTESIAN_POINT ( 'NONE',  ( -6.143904198944369455, -13.77689918168226235, 23.00000000000000000 ) ) ;
#11530 = CARTESIAN_POINT ( 'NONE',  ( 14.52179210396188758, 28.39636537094187574, -7.765798819039245515 ) ) ;
#11531 = DIRECTION ( 'NONE',  ( 1.000000000000000000, 0.000000000000000000, 0.000000000000000000 ) ) ;
#11532 = VERTEX_POINT ( 'NONE', #35226 ) ;
#11534 = CARTESIAN_POINT ( 'NONE',  ( -8.118377661053488126, 10.47536095541708967, 7.000000000000000000 ) ) ;
#11533 = CARTESIAN_POINT ( 'NONE',  ( -16.43970055640401640, 12.42160327418225663, -27.72196673367218622 ) ) ;
#11535 = CARTESIAN_POINT ( 'NONE',  ( -13.63581098909220479, 27.45627467658446008, 10.99999999999999289 ) ) ;
#11536 = CARTESIAN_POINT ( 'NONE',  ( 10.85850211433846013, -19.98559300887557555, -21.61446395924937036 ) ) ;
#11537 = CARTESIAN_POINT ( 'NONE',  ( 15.41558956916362000, 26.78481017491965233, -5.000000000000000000 ) ) ;
#11538 = CARTESIAN_POINT ( 'NONE',  ( 12.38021073363059799, 20.50496940924477229, -19.49405221216574091 ) ) ;
#11539 = CARTESIAN_POINT ( 'NONE',  ( 12.30736835487432757, 14.81698729810772441, 7.000000000000000000 ) ) ;
#11540 = EDGE_CURVE ( 'NONE', #12049, #28113, #17377, .T. ) ;
#11541 = DIRECTION ( 'NONE',  ( 0.2079116908177656708, 0.9781476007338043566, -0.000000000000000000 ) ) ;
#11542 = AXIS2_PLACEMENT_3D ( 'NONE', #3450, #21932, #15646 ) ;
#11543 = CIRCLE ( 'NONE', #39429, 0.5000000000000004441 ) ;
#11544 = CARTESIAN_POINT ( 'NONE',  ( -27.52659592799652444, -22.96876690456295123, -9.758689385506642111 ) ) ;
#11545 = CARTESIAN_POINT ( 'NONE',  ( 4.025418116673052715, -24.86707171575129038, -5.000000000000002665 ) ) ;
#11546 = CARTESIAN_POINT ( 'NONE',  ( 14.65085127499396478, 24.64916743084969042, -11.60854621773958684 ) ) ;
#11547 = CARTESIAN_POINT ( 'NONE',  ( 20.78558868895880707, 12.80151593431163093, -9.395610594804281845 ) ) ;
#11548 = DIRECTION ( 'NONE',  ( 0.000000000000000000, 0.000000000000000000, 1.000000000000000000 ) ) ;
#11549 = ORIENTED_EDGE ( 'NONE', *, *, #11787, .F. ) ;
#11550 = CARTESIAN_POINT ( 'NONE',  ( -4.067729689095753720, 20.10162097886301780, -29.99999999999998934 ) ) ;
#11551 = AXIS2_PLACEMENT_3D ( 'NONE', #28840, #1018, #36542 ) ;
#11552 = ORIENTED_EDGE ( 'NONE', *, *, #33839, .F. ) ;
#11553 = VECTOR ( 'NONE', #2954, 1000.000000000000114 ) ;
#11554 = CARTESIAN_POINT ( 'NONE',  ( -16.24129362380739749, 27.01431713447837524, 15.13084544680213739 ) ) ;
#11555 = VERTEX_POINT ( 'NONE', #7386 ) ;
#11556 = DIRECTION ( 'NONE',  ( 0.000000000000000000, 0.000000000000000000, 1.000000000000000000 ) ) ;
#11557 = CARTESIAN_POINT ( 'NONE',  ( 9.415016184005738253, 11.18446770392332468, 10.49999999999999822 ) ) ;
#11558 = EDGE_LOOP ( 'NONE', ( #16770, #4256, #11688, #12078 ) ) ;
#11559 = CARTESIAN_POINT ( 'NONE',  ( -30.40797137996420929, 0.1992154573447958432, -7.358886591698631463 ) ) ;
#11560 = CARTESIAN_POINT ( 'NONE',  ( 20.01479607499403812, -5.392035505496489023, -27.79632597738025623 ) ) ;
#11561 = EDGE_LOOP ( 'NONE', ( #1103, #28853, #7859, #13257 ) ) ;
#11562 = CONTEXT_DEPENDENT_SHAPE_REPRESENTATION ( #34517, #3513 ) ;
#11563 = CARTESIAN_POINT ( 'NONE',  ( -13.46929972531958875, 26.35070966310182783, 9.500000000000000000 ) ) ;
#11564 = VERTEX_POINT ( 'NONE', #7796 ) ;
#11565 = EDGE_CURVE ( 'NONE', #29202, #35666, #5667, .T. ) ;
#11566 = CARTESIAN_POINT ( 'NONE',  ( 2.036571916123614656, 8.108948098542045457, 9.500000000000000000 ) ) ;
#11567 = DIRECTION ( 'NONE',  ( 0.000000000000000000, 0.000000000000000000, 1.000000000000000000 ) ) ;
#11568 = CIRCLE ( 'NONE', #27800, 0.4999999999999995559 ) ;
#11569 = AXIS2_PLACEMENT_3D ( 'NONE', #28280, #37027, #18155 ) ;
#11570 = PLANE ( 'NONE',  #8442 ) ;
#11571 = ORIENTED_EDGE ( 'NONE', *, *, #7684, .F. ) ;
#11572 = CARTESIAN_POINT ( 'NONE',  ( 15.21690391738993320, 27.44427296666788862, 12.00000000000000000 ) ) ;
#11573 = CARTESIAN_POINT ( 'NONE',  ( -1.838889047819898037, 31.15129278236396360, 9.000000000000001776 ) ) ;
#11574 = CARTESIAN_POINT ( 'NONE',  ( -2.587667106213709101, 35.31811204475769728, 13.00000000000000178 ) ) ;
#11575 = CARTESIAN_POINT ( 'NONE',  ( 16.14253851327366363, 13.55324706950144886, -24.35198715851059248 ) ) ;
#11576 = CIRCLE ( 'NONE', #32347, 0.4999999999999999445 ) ;
#11577 = CARTESIAN_POINT ( 'NONE',  ( 10.13695427535512117, 26.23223918441782843, -16.00337151103656552 ) ) ;
#11578 = ORIENTED_EDGE ( 'NONE', *, *, #4408, .T. ) ;
#11579 = CARTESIAN_POINT ( 'NONE',  ( -21.66453300257672154, 11.69411660682930787, -7.917832817197552053 ) ) ;
#11580 = DIRECTION ( 'NONE',  ( 0.000000000000000000, 0.000000000000000000, 1.000000000000000000 ) ) ;
#11581 = CARTESIAN_POINT ( 'NONE',  ( 3.476901250629512941, 26.36149378532653031, 6.000000000000000000 ) ) ;
#11582 = CARTESIAN_POINT ( 'NONE',  ( 15.98679081489500575, -26.83810770539577106, -5.940741301600179547 ) ) ;
#11583 = CARTESIAN_POINT ( 'NONE',  ( 6.576253646258392926, 14.29921418520925869, 10.50000000000000000 ) ) ;
#11584 = CARTESIAN_POINT ( 'NONE',  ( 9.665073660139013256, 25.11464168560187460, 10.00000000000000000 ) ) ;
#11585 = EDGE_CURVE ( 'NONE', #22756, #26036, #27704, .T. ) ;
#11586 = CARTESIAN_POINT ( 'NONE',  ( -11.11125591800278478, 17.62252618941018056, -26.82911783566601116 ) ) ;
#11587 = CARTESIAN_POINT ( 'NONE',  ( -15.42415429988070841, -17.33959852952462910, -22.15376138321191490 ) ) ;
#11588 = CARTESIAN_POINT ( 'NONE',  ( 14.27123303369756790, -26.41390335293325009, -5.946466403055868710 ) ) ;
#11589 = EDGE_CURVE ( 'NONE', #13116, #6755, #31779, .T. ) ;
#11590 = ADVANCED_FACE ( 'NONE', ( #10042 ), #37443, .T. ) ;
#11591 = DIRECTION ( 'NONE',  ( 1.000000000000000000, 0.000000000000000000, 0.000000000000000000 ) ) ;
#11592 = VERTEX_POINT ( 'NONE', #20605 ) ;
#11593 = ORIENTED_EDGE ( 'NONE', *, *, #4387, .T. ) ;
#11594 = B_SPLINE_CURVE_WITH_KNOTS ( 'NONE', 3,
 ( #34480, #18841, #6627, #19035, #31427, #3594 ),
 .UNSPECIFIED., .F., .F.,
 ( 4, 2, 4 ),
 ( 0.000000000000000000, 0.5000000000000000000, 1.000000000000000000 ),
 .UNSPECIFIED. ) ;
#11595 = CARTESIAN_POINT ( 'NONE',  ( -10.66039439689632395, 26.89947780815539247, -15.04199405158239600 ) ) ;
#11596 = CARTESIAN_POINT ( 'NONE',  ( 12.19971670159632637, 4.637739668175409058, 7.000000000000000000 ) ) ;
#11597 = CARTESIAN_POINT ( 'NONE',  ( -12.48446084878477436, 14.34248059624584926, 10.49999999999999822 ) ) ;
#11598 = AXIS2_PLACEMENT_3D ( 'NONE', #4608, #36300, #35693 ) ;
#11599 = AXIS2_PLACEMENT_3D ( 'NONE', #13973, #38151, #13767 ) ;
#11600 = ADVANCED_FACE ( 'NONE', ( #23642 ), #33003, .F. ) ;
#11601 = CARTESIAN_POINT ( 'NONE',  ( -11.80736835487443592, 13.95096189432345213, 7.000000000000000000 ) ) ;
#11602 = ORIENTED_EDGE ( 'NONE', *, *, #15225, .T. ) ;
#11603 = CARTESIAN_POINT ( 'NONE',  ( 29.72646830413813390, 0.1273344848627241122, -9.710811668020681964 ) ) ;
#11604 = DIRECTION ( 'NONE',  ( 1.000000000000000000, 0.000000000000000000, 0.000000000000000000 ) ) ;
#11605 = CARTESIAN_POINT ( 'NONE',  ( -2.606860170653613640, 7.830819977571337631, 10.82238861112329609 ) ) ;
#11606 = AXIS2_PLACEMENT_3D ( 'NONE', #8616, #36448, #31341 ) ;
#11607 = ORIENTED_EDGE ( 'NONE', *, *, #32408, .F. ) ;
#11608 = CARTESIAN_POINT ( 'NONE',  ( -30.87691200222618804, -0.01437998035276856316, -5.474195421119384619 ) ) ;
#11609 = CARTESIAN_POINT ( 'NONE',  ( -14.07088901726633345, 27.73527618063616984, 10.49999999999999645 ) ) ;
#11610 = ORIENTED_EDGE ( 'NONE', *, *, #12965, .T. ) ;
#11611 = CARTESIAN_POINT ( 'NONE',  ( 32.29142382855410176, -3.921780356570798709, -9.954602144452415757 ) ) ;
#11612 = CARTESIAN_POINT ( 'NONE',  ( 34.78305373678702495, -20.08200543817097738, 13.32518128616608877 ) ) ;
#11613 = VERTEX_POINT ( 'NONE', #38882 ) ;
#11614 = CARTESIAN_POINT ( 'NONE',  ( -9.055806345858652406, 37.53717483670035193, 13.92931973827746717 ) ) ;
#11615 = CARTESIAN_POINT ( 'NONE',  ( 7.766013557953383106, 28.81973365084986938, 10.50000000000000178 ) ) ;
#11616 = ADVANCED_FACE ( 'NONE', ( #11058 ), #33598, .F. ) ;
#11617 = DIRECTION ( 'NONE',  ( -0.000000000000000000, -0.000000000000000000, -1.000000000000000000 ) ) ;
#11618 = EDGE_CURVE ( 'NONE', #19095, #20361, #2313, .T. ) ;
#11619 = CARTESIAN_POINT ( 'NONE',  ( -7.486246565637331948E-14, 31.60047892813804538, 20.50957957746028626 ) ) ;
#11620 = CARTESIAN_POINT ( 'NONE',  ( -11.14717575287011542, 32.53695909538323860, 13.00000000000000178 ) ) ;
#11621 = EDGE_LOOP ( 'NONE', ( #26582, #25860, #7537, #31168 ) ) ;
#11622 = FACE_OUTER_BOUND ( 'NONE', #31609, .T. ) ;
#11623 = CARTESIAN_POINT ( 'NONE',  ( 2.256323172317815207, 14.28970123917151192, 7.000000000000000000 ) ) ;
#11624 = AXIS2_PLACEMENT_3D ( 'NONE', #31805, #25310, #7771 ) ;
#11626 = CIRCLE ( 'NONE', #18127, 0.5000000000000004441 ) ;
#11625 = CARTESIAN_POINT ( 'NONE',  ( 4.474472994054608854, 23.12859998392846705, -21.95241731158036202 ) ) ;
#11627 = DIRECTION ( 'NONE',  ( -0.2079116908177664480, -0.9781476007338042455, 0.000000000000000000 ) ) ;
#11628 = CARTESIAN_POINT ( 'NONE',  ( 8.755436920352806851, 18.76929632773553180, 20.82122704794083390 ) ) ;
#11629 = CARTESIAN_POINT ( 'NONE',  ( 13.15139800428180727, -18.60661763037684224, -22.40227382322720118 ) ) ;
#11630 = CARTESIAN_POINT ( 'NONE',  ( 16.82090372984190907, 29.19711159930552924, 10.99999999999877787 ) ) ;
#11631 = TOROIDAL_SURFACE ( 'NONE', #19389, 1.000000000000000000, 0.5000000000000000000 ) ;
#11632 = LINE ( 'NONE', #17738, #15717 ) ;
#11633 = LINE ( 'NONE', #2090, #9680 ) ;
#11634 = ORIENTED_EDGE ( 'NONE', *, *, #28957, .F. ) ;
#11635 = ADVANCED_FACE ( 'NONE', ( #26887 ), #39675, .T. ) ;
#11636 = CARTESIAN_POINT ( 'NONE',  ( 13.72215835960534314, 23.50258046650561283, -14.46509339062811250 ) ) ;
#11637 = ORIENTED_EDGE ( 'NONE', *, *, #11385, .T. ) ;
#11638 = CARTESIAN_POINT ( 'NONE',  ( -15.42052737914556637, 25.77605439453884273, -7.831307328786774491 ) ) ;
#11639 = CARTESIAN_POINT ( 'NONE',  ( -29.67744882842988829, -20.56940131916892867, 18.42518152272108622 ) ) ;
#11640 = EDGE_CURVE ( 'NONE', #13994, #490, #11454, .T. ) ;
#11641 = DIRECTION ( 'NONE',  ( 0.000000000000000000, 0.000000000000000000, 1.000000000000000000 ) ) ;
#11642 = CARTESIAN_POINT ( 'NONE',  ( 15.34434150811012465, 26.34414864991459737, -7.358482492565846300 ) ) ;
#11643 = EDGE_LOOP ( 'NONE', ( #38325, #24303, #20934, #32421 ) ) ;
#11644 = CARTESIAN_POINT ( 'NONE',  ( 32.27861313376966734, -19.10088880322608418, -8.403838041204926057 ) ) ;
#11645 = ORIENTED_EDGE ( 'NONE', *, *, #10761, .F. ) ;
#11647 = CARTESIAN_POINT ( 'NONE',  ( -11.11016527260153630, 31.83082137946488643, 7.000000000000000000 ) ) ;
#11646 = CARTESIAN_POINT ( 'NONE',  ( -12.92543041999867803, 22.74201982050020376, -16.38141219968167306 ) ) ;
#11648 = CARTESIAN_POINT ( 'NONE',  ( -16.98077657287944220, -25.38500131946631200, -11.42923376808981928 ) ) ;
#11649 = CARTESIAN_POINT ( 'NONE',  ( -4.524139159579195102, 31.43208625488816566, 10.50000000000000888 ) ) ;
#11650 = ORIENTED_EDGE ( 'NONE', *, *, #36068, .T. ) ;
#11651 = ADVANCED_FACE ( 'NONE', ( #36246 ), #27290, .F. ) ;
#11652 = CARTESIAN_POINT ( 'NONE',  ( -26.89345970280778175, -10.16057822180111536, -16.68776630141959316 ) ) ;
#11653 = CARTESIAN_POINT ( 'NONE',  ( -15.26455680675359972, -26.65982646153380031, -5.946113180645928864 ) ) ;
#11654 = CARTESIAN_POINT ( 'NONE',  ( 23.09341953181399987, -31.04079623446942193, 22.99999999999999289 ) ) ;
#11655 = EDGE_LOOP ( 'NONE', ( #36318, #33748 ) ) ;
#11656 = CARTESIAN_POINT ( 'NONE',  ( 21.79450343673522639, 2.315575432259290523, -22.92150830105099146 ) ) ;
#11657 = DIRECTION ( 'NONE',  ( 1.000000000000000000, 0.000000000000000000, 0.000000000000000000 ) ) ;
#11658 = CARTESIAN_POINT ( 'NONE',  ( -2.229437847141422679, 24.50739181907689712, 12.00000000000000000 ) ) ;
#11659 = EDGE_LOOP ( 'NONE', ( #16653, #3522 ) ) ;
#11660 = CARTESIAN_POINT ( 'NONE',  ( -21.28869832545893814, 0.6870496981110076895, -25.00484597054681757 ) ) ;
#11661 = VERTEX_POINT ( 'NONE', #39480 ) ;
#11662 = CARTESIAN_POINT ( 'NONE',  ( 32.00254677347309951, -1.406971461693646397, -6.390648070956889804 ) ) ;
#11663 = VECTOR ( 'NONE', #31399, 1000.000000000000000 ) ;
#11664 = CARTESIAN_POINT ( 'NONE',  ( 30.53792857583748699, -5.895195796383389641, 19.27171037444157875 ) ) ;
#11665 = ORIENTED_EDGE ( 'NONE', *, *, #35362, .T. ) ;
#11666 = CARTESIAN_POINT ( 'NONE',  ( -27.39893270769881184, 2.645307716681419397, -10.24383054656171765 ) ) ;
#11667 = DIRECTION ( 'NONE',  ( -1.000000000000000000, -1.224646799147351235E-16, 0.000000000000000000 ) ) ;
#11668 = EDGE_CURVE ( 'NONE', #488, #30103, #31626, .T. ) ;
#11669 = CARTESIAN_POINT ( 'NONE',  ( 6.935770203493858865, 22.34671014717335780, 13.00000000000000178 ) ) ;
#11670 = CARTESIAN_POINT ( 'NONE',  ( 3.211395437248501850, 12.61633075744433796, 12.00000000000000000 ) ) ;
#11671 = FACE_BOUND ( 'NONE', #34035, .T. ) ;
#11672 = CARTESIAN_POINT ( 'NONE',  ( 10.29511041547406691, 24.79362192464177639, 11.00000000000000000 ) ) ;
#11673 = VERTEX_POINT ( 'NONE', #5547 ) ;
#11674 = CARTESIAN_POINT ( 'NONE',  ( -22.74773350093838431, 5.112260648264027374, -17.82922536596295160 ) ) ;
#11675 = CARTESIAN_POINT ( 'NONE',  ( 14.09933648065468503, 26.02968990214155198, 10.50000000000000533 ) ) ;
#11676 = LINE ( 'NONE', #33027, #7757 ) ;
#11677 = CARTESIAN_POINT ( 'NONE',  ( 17.90862233137103132, -16.51690928828630689, -20.84349936702684047 ) ) ;
#11678 = DIRECTION ( 'NONE',  ( 0.000000000000000000, 0.000000000000000000, 1.000000000000000000 ) ) ;
#11679 = CARTESIAN_POINT ( 'NONE',  ( 11.43364758157541949, 19.15105928248557987, -22.69143459194921064 ) ) ;
#11680 = CARTESIAN_POINT ( 'NONE',  ( -14.98890121934605268, -28.67928442654203636, 11.00000000000000000 ) ) ;
#11681 = CIRCLE ( 'NONE', #39574, 1.000000000000000000 ) ;
#11682 = EDGE_LOOP ( 'NONE', ( #33193, #23823, #28220, #18056 ) ) ;
#11683 = CARTESIAN_POINT ( 'NONE',  ( -14.25469411907181261, 18.74119916489544124, -18.70450738159251713 ) ) ;
#11684 = CARTESIAN_POINT ( 'NONE',  ( -27.31307357281963277, -8.451814904569179276, 20.69868183039799447 ) ) ;
#11685 = EDGE_CURVE ( 'NONE', #29068, #4691, #32919, .T. ) ;
#11686 = CARTESIAN_POINT ( 'NONE',  ( -8.910254037844424602, 17.93301270189230578, 10.50000000000000178 ) ) ;
#11687 = CARTESIAN_POINT ( 'NONE',  ( 15.41486640184582235, 26.69476953482462989, -5.946086842317699350 ) ) ;
#11688 = ORIENTED_EDGE ( 'NONE', *, *, #13748, .F. ) ;
#11689 = DIRECTION ( 'NONE',  ( -1.000000000000000000, 0.000000000000000000, 0.000000000000000000 ) ) ;
#11690 = VECTOR ( 'NONE', #20469, 999.9999999999998863 ) ;
#11691 = EDGE_LOOP ( 'NONE', ( #35881, #28676, #14436 ) ) ;
#11693 = CARTESIAN_POINT ( 'NONE',  ( 14.97277451176449325, 21.48159783397873923, 10.49999999999999822 ) ) ;
#11692 = CARTESIAN_POINT ( 'NONE',  ( -15.35726121420015211, 26.89840538448078888, -5.944526096835159201 ) ) ;
#11694 = CARTESIAN_POINT ( 'NONE',  ( -14.77304657029772805, -25.65973629052345828, -10.17934284075853490 ) ) ;
#11695 = DIRECTION ( 'NONE',  ( 0.000000000000000000, 0.000000000000000000, 1.000000000000000000 ) ) ;
#11696 = CARTESIAN_POINT ( 'NONE',  ( -32.89633676153053443, -18.52163263618783162, -7.970821576684871346 ) ) ;
#11697 = CARTESIAN_POINT ( 'NONE',  ( -12.68866578116655397, -24.42420696973755767, -12.60002993717948172 ) ) ;
#11698 = DIRECTION ( 'NONE',  ( 0.000000000000000000, 0.000000000000000000, 1.000000000000000000 ) ) ;
#11699 = CARTESIAN_POINT ( 'NONE',  ( 12.23345151996672264, 16.79682170085633430, -26.92720819876614158 ) ) ;
#11700 = ORIENTED_EDGE ( 'NONE', *, *, #2346, .F. ) ;
#11701 = CARTESIAN_POINT ( 'NONE',  ( 24.72357752798934882, 6.416377239431996671, -9.837715644156144634 ) ) ;
#11702 = CARTESIAN_POINT ( 'NONE',  ( -9.788946493797832105, 21.72623886970244911, 6.000000000000000000 ) ) ;
#11703 = DIRECTION ( 'NONE',  ( 0.000000000000000000, 0.000000000000000000, 1.000000000000000000 ) ) ;
#11704 = CARTESIAN_POINT ( 'NONE',  ( 0.000000000000000000, 22.50000000000000355, 0.000000000000000000 ) ) ;
#11705 = ORIENTED_EDGE ( 'NONE', *, *, #30256, .F. ) ;
#11706 = CARTESIAN_POINT ( 'NONE',  ( -26.47597712984326890, -0.7517266478712665290, -16.31359411516780966 ) ) ;
#11707 = CARTESIAN_POINT ( 'NONE',  ( 28.39060983474474753, 0.07700895002038117554, -12.54401228622873354 ) ) ;
#11708 = VECTOR ( 'NONE', #11369, 1000.000000000000000 ) ;
#11709 = CARTESIAN_POINT ( 'NONE',  ( -9.734896950324548826, 32.61097331450152836, 10.50000000000000000 ) ) ;
#11710 = CARTESIAN_POINT ( 'NONE',  ( 19.25012218476983605, -17.89323886701251354, 20.94377226548378346 ) ) ;
#11711 = DIRECTION ( 'NONE',  ( -0.000000000000000000, -0.000000000000000000, -1.000000000000000000 ) ) ;
#11712 = CARTESIAN_POINT ( 'NONE',  ( -7.111215932167764819, 17.81698729810783988, 9.000000000000001776 ) ) ;
#11713 = ADVANCED_FACE ( 'NONE', ( #6728 ), #1119, .T. ) ;
#11714 = VERTEX_POINT ( 'NONE', #12244 ) ;
#11715 = EDGE_CURVE ( 'NONE', #32514, #15350, #21389, .T. ) ;
#11716 = CIRCLE ( 'NONE', #32455, 1.000000000000000000 ) ;
#11717 = CARTESIAN_POINT ( 'NONE',  ( 14.97435279638159322, 21.61966441463743749, 7.485646746502383486 ) ) ;
#11718 = CARTESIAN_POINT ( 'NONE',  ( 6.856875760695868571, 35.58019112794455907, 10.49999999999999822 ) ) ;
#11719 = FACE_OUTER_BOUND ( 'NONE', #7259, .T. ) ;
#11720 = CARTESIAN_POINT ( 'NONE',  ( 0.4051383682548583276, 37.70807721162720583, -7.971661926679036725 ) ) ;
#11721 = FACE_OUTER_BOUND ( 'NONE', #16930, .T. ) ;
#11722 = CARTESIAN_POINT ( 'NONE',  ( 14.43694901005322961, 26.51279404187409483, 17.42190598798392998 ) ) ;
#11723 = EDGE_CURVE ( 'NONE', #22206, #10321, #29690, .T. ) ;
#11724 = LINE ( 'NONE', #40141, #34967 ) ;
#11725 = DIRECTION ( 'NONE',  ( 1.000000000000000000, 0.000000000000000000, 0.000000000000000000 ) ) ;
#11726 = CARTESIAN_POINT ( 'NONE',  ( -7.577547685840081648, 11.84256962714647798, 12.00000000000000000 ) ) ;
#11727 = CARTESIAN_POINT ( 'NONE',  ( -5.440908595777636414, 35.94977745735568675, 11.00000000000000000 ) ) ;
#11728 = CARTESIAN_POINT ( 'NONE',  ( 10.21381146793931549, 18.84016815455725080, -24.86718924084146565 ) ) ;
#11729 = CARTESIAN_POINT ( 'NONE',  ( -10.39021566973305788, 20.90519018800561213, 10.00000000000000000 ) ) ;
#11730 = ORIENTED_EDGE ( 'NONE', *, *, #6012, .T. ) ;
#11731 = AXIS2_PLACEMENT_3D ( 'NONE', #31343, #31940, #21796 ) ;
#11733 = CARTESIAN_POINT ( 'NONE',  ( -9.806982162272253944, 13.84996144622306247, 13.00000000000000178 ) ) ;
#11732 = CARTESIAN_POINT ( 'NONE',  ( -19.14596416633794718, 16.58431542591694097, -6.930462030153276665 ) ) ;
#11734 = CARTESIAN_POINT ( 'NONE',  ( -13.86243997625759583, 27.52991089825177795, 10.94387467463492136 ) ) ;
#11735 = VECTOR ( 'NONE', #17022, 1000.000000000000000 ) ;
#11736 = CARTESIAN_POINT ( 'NONE',  ( 15.36829843292950848, -26.58855099483750806, -6.887934304372063110 ) ) ;
#11737 = CARTESIAN_POINT ( 'NONE',  ( -3.503793317224518145, 8.420815634768723967, 7.000000000000000000 ) ) ;
#11738 = CARTESIAN_POINT ( 'NONE',  ( 15.35679505265130373, 26.72643039084889338, -6.416339992001557135 ) ) ;
#11739 = ORIENTED_EDGE ( 'NONE', *, *, #6521, .F. ) ;
#11740 = CARTESIAN_POINT ( 'NONE',  ( 12.05832241004688399, 18.99596958976722760, -21.04195414767209726 ) ) ;
#11741 = CARTESIAN_POINT ( 'NONE',  ( -11.77091082532341204, 29.60251629318183575, 12.00000000000000000 ) ) ;
#11742 = CARTESIAN_POINT ( 'NONE',  ( -16.64620719159282913, -13.00137674719640835, -26.29768302675261182 ) ) ;
#11743 = CARTESIAN_POINT ( 'NONE',  ( 4.003204069988485436, -24.78938737036088824, -6.934010167115818746 ) ) ;
#11744 = CARTESIAN_POINT ( 'NONE',  ( 12.64121829060639968, 20.16165939183971290, -19.53956656712336581 ) ) ;
#11745 = CARTESIAN_POINT ( 'NONE',  ( 18.17819536212576281, 10.17765543567462494, -25.51248847685047849 ) ) ;
#11746 = DIRECTION ( 'NONE',  ( 1.000000000000000000, 0.000000000000000000, 0.000000000000000000 ) ) ;
#11747 = EDGE_CURVE ( 'NONE', #16315, #22657, #34384, .T. ) ;
#11748 = AXIS2_PLACEMENT_3D ( 'NONE', #32311, #7717, #35759 ) ;
#11749 = CARTESIAN_POINT ( 'NONE',  ( -4.163637899402453435, 37.39365738118117832, -7.553763481216830833 ) ) ;
#11750 = ORIENTED_EDGE ( 'NONE', *, *, #8221, .T. ) ;
#11751 = CARTESIAN_POINT ( 'NONE',  ( -17.34253826607279692, 27.32041144403692101, 11.55979286843934872 ) ) ;
#11752 = ORIENTED_EDGE ( 'NONE', *, *, #21935, .T. ) ;
#11753 = CARTESIAN_POINT ( 'NONE',  ( -12.80736835487442349, 15.68301270189233954, 7.000000000000000000 ) ) ;
#11754 = DIRECTION ( 'NONE',  ( 0.000000000000000000, 0.000000000000000000, 1.000000000000000000 ) ) ;
#11755 = CARTESIAN_POINT ( 'NONE',  ( -20.68510868473422804, 0.9644064859642085263, -27.45587699270683402 ) ) ;
#11756 = CARTESIAN_POINT ( 'NONE',  ( 35.33511270614809519, -11.84873732983155925, -6.293930992841885619 ) ) ;
#11757 = EDGE_CURVE ( 'NONE', #19499, #20763, #29017, .T. ) ;
#11758 = VERTEX_POINT ( 'NONE', #37630 ) ;
#11759 = CONTEXT_DEPENDENT_SHAPE_REPRESENTATION ( #35290, #22660 ) ;
#11760 = CARTESIAN_POINT ( 'NONE',  ( 10.33787318040696057, 33.36945112946456504, 7.203056206335834766 ) ) ;
#11761 = EDGE_LOOP ( 'NONE', ( #39866, #37156, #6134, #34582 ) ) ;
#11762 = DIRECTION ( 'NONE',  ( -0.8090169943749423442, 0.5877852522924800205, 0.000000000000000000 ) ) ;
#11763 = DIRECTION ( 'NONE',  ( -0.7071067811865526798, 0.000000000000000000, -0.7071067811865424657 ) ) ;
#11764 = LINE ( 'NONE', #2623, #37584 ) ;
#11765 = ORIENTED_EDGE ( 'NONE', *, *, #33709, .F. ) ;
#11766 = EDGE_CURVE ( 'NONE', #6428, #19542, #18746, .T. ) ;
#11767 =( LENGTH_UNIT ( ) NAMED_UNIT ( * ) SI_UNIT ( .MILLI., .METRE. ) );
#11768 = CARTESIAN_POINT ( 'NONE',  ( -4.835137251120299240, 29.44922644035488446, 13.00000000000000178 ) ) ;
#11769 = FACE_OUTER_BOUND ( 'NONE', #21696, .T. ) ;
#11770 = EDGE_CURVE ( 'NONE', #7975, #2021, #31530, .T. ) ;
#11771 = CARTESIAN_POINT ( 'NONE',  ( 1.000000000000000000, 37.00000000000000711, 7.500000000000000888 ) ) ;
#11772 = CARTESIAN_POINT ( 'NONE',  ( 26.24913643253236373, -20.23034912788282469, -12.91558456940952837 ) ) ;
#11773 = CARTESIAN_POINT ( 'NONE',  ( 17.45454598098198673, 15.08987660865141933, -16.91469807549161075 ) ) ;
#11774 = CARTESIAN_POINT ( 'NONE',  ( 7.745869706829908274, 19.75473637109295311, -25.89095885954563769 ) ) ;
#11775 = ORIENTED_EDGE ( 'NONE', *, *, #20332, .F. ) ;
#11776 = CARTESIAN_POINT ( 'NONE',  ( -21.71367720907299770, 11.71909836743509636, -7.427745397021046969 ) ) ;
#11777 = FACE_OUTER_BOUND ( 'NONE', #1465, .T. ) ;
#11778 = CARTESIAN_POINT ( 'NONE',  ( -14.72984284853662729, 19.66343513167324630, 7.102637441331452806 ) ) ;
#11779 = CARTESIAN_POINT ( 'NONE',  ( 14.99950937118286021, -25.70747749863527076, -10.16616245189924506 ) ) ;
#11780 = CARTESIAN_POINT ( 'NONE',  ( -8.294006203984645609, 33.46401007850805343, 6.000000000000000000 ) ) ;
#11781 = CYLINDRICAL_SURFACE ( 'NONE', #29576, 18.00000000000003553 ) ;
#11782 = CARTESIAN_POINT ( 'NONE',  ( -15.38932783545047478, 26.78602940361181339, -5.945706122906532443 ) ) ;
#11783 = AXIS2_PLACEMENT_3D ( 'NONE', #5663, #14621, #30663 ) ;
#11784 = CARTESIAN_POINT ( 'NONE',  ( -24.93964139829124704, -26.28816300898122194, -5.879745673036421927 ) ) ;
#11785 = CARTESIAN_POINT ( 'NONE',  ( 13.51079035047422749, -25.25079545357177935, -10.67726867737688323 ) ) ;
#11786 = AXIS2_PLACEMENT_3D ( 'NONE', #30461, #36751, #15009 ) ;
#11787 = EDGE_CURVE ( 'NONE', #36348, #36134, #34882, .T. ) ;
#11788 = DIRECTION ( 'NONE',  ( -0.3090169943749450643, 0.9510565162951543083, 0.000000000000000000 ) ) ;
#11789 = EDGE_CURVE ( 'NONE', #29252, #9948, #22178, .T. ) ;
#11790 = ORIENTED_EDGE ( 'NONE', *, *, #7907, .T. ) ;
#11791 = VERTEX_POINT ( 'NONE', #15292 ) ;
#11792 = CARTESIAN_POINT ( 'NONE',  ( -12.54669116579298027, 32.01363879718496719, -7.228269468828303346 ) ) ;
#11793 = DIRECTION ( 'NONE',  ( -0.8660254037844432595, -0.4999999999999920064, 0.000000000000000000 ) ) ;
#11794 = DIRECTION ( 'NONE',  ( -0.9510565162951503115, 0.3090169943749573322, 0.000000000000000000 ) ) ;
#11795 = CARTESIAN_POINT ( 'NONE',  ( -9.417813166173889527, 10.93662330136618444, 10.49999999999999822 ) ) ;
#11796 = ORIENTED_EDGE ( 'NONE', *, *, #4163, .T. ) ;
#11797 = CARTESIAN_POINT ( 'NONE',  ( 30.86596729670053563, -0.003225903683491798332, -5.474191125761192822 ) ) ;
#11798 = DIRECTION ( 'NONE',  ( 1.000000000000000000, 3.469446951953568829E-15, 0.000000000000000000 ) ) ;
#11799 = VECTOR ( 'NONE', #39416, 1000.000000000000000 ) ;
#11800 = CARTESIAN_POINT ( 'NONE',  ( -3.813962023474481544, 32.29559562678526419, 10.50000000000000000 ) ) ;
#11801 = VERTEX_POINT ( 'NONE', #27484 ) ;
#11802 = CARTESIAN_POINT ( 'NONE',  ( -23.93377115618524442, 0.5022394957162249485, -19.49836098978260068 ) ) ;
#11803 = CARTESIAN_POINT ( 'NONE',  ( -9.427394962683591118, 11.06314620782489833, 10.49999999999999822 ) ) ;
#11804 = ORIENTED_EDGE ( 'NONE', *, *, #16513, .F. ) ;
#11805 = CARTESIAN_POINT ( 'NONE',  ( 34.09142973781642638, -5.184893016320399006, -6.786029529690497775 ) ) ;
#11806 = CARTESIAN_POINT ( 'NONE',  ( 33.02831943717437468, -0.5583946152424188458, 14.53008259254167811 ) ) ;
#11807 = ORIENTED_EDGE ( 'NONE', *, *, #39545, .T. ) ;
#11808 = CARTESIAN_POINT ( 'NONE',  ( -3.652674690108859146, 39.05729514278205272, 15.13084544680221200 ) ) ;
#11809 = CARTESIAN_POINT ( 'NONE',  ( -5.730292628140351674, -18.69445663741131014, 20.25080042701566541 ) ) ;
#11810 = CARTESIAN_POINT ( 'NONE',  ( 13.36830325120611995, 20.48707633493483371, 7.000000000000000000 ) ) ;
#11811 = EDGE_CURVE ( 'NONE', #32024, #30975, #15496, .T. ) ;
#11812 = CARTESIAN_POINT ( 'NONE',  ( -6.978236406932369462, 28.42397902804928833, 20.50957957746028271 ) ) ;
#11813 = DIRECTION ( 'NONE',  ( 0.000000000000000000, 0.000000000000000000, 1.000000000000000000 ) ) ;
#11814 = ORIENTED_EDGE ( 'NONE', *, *, #15504, .F. ) ;
#11815 = DIRECTION ( 'NONE',  ( 0.000000000000000000, 0.000000000000000000, 1.000000000000000000 ) ) ;
#11816 = DIRECTION ( 'NONE',  ( 0.000000000000000000, 0.000000000000000000, 1.000000000000000000 ) ) ;
#11817 = CARTESIAN_POINT ( 'NONE',  ( 7.586125664261425428, 33.43449133166674869, -11.13268412101803939 ) ) ;
#11818 = DIRECTION ( 'NONE',  ( -0.2185080122244276168, -0.6724985119639504960, 0.7071067811865486830 ) ) ;
#11819 = CARTESIAN_POINT ( 'NONE',  ( 8.768078002820624661, 24.93711404286646527, 20.50957957746029336 ) ) ;
#11820 = VECTOR ( 'NONE', #26742, 1000.000000000000000 ) ;
#11821 = CARTESIAN_POINT ( 'NONE',  ( 18.83296736436365393, -24.71623834213119153, -12.24355243440530749 ) ) ;
#11822 = SURFACE_SIDE_STYLE ('',( #37405 ) ) ;
#11823 = CARTESIAN_POINT ( 'NONE',  ( -12.84742388243067168, 15.65988663227498456, 11.00000000000000000 ) ) ;
#11824 = CARTESIAN_POINT ( 'NONE',  ( -19.48557158514988785, -11.24999999999987743, 10.00000000000000000 ) ) ;
#11825 = ORIENTED_EDGE ( 'NONE', *, *, #36882, .T. ) ;
#11826 = CARTESIAN_POINT ( 'NONE',  ( 15.30964094714013690, 26.71768783952137483, -6.885809892569045410 ) ) ;
#11827 = ORIENTED_EDGE ( 'NONE', *, *, #8152, .T. ) ;
#11828 = CARTESIAN_POINT ( 'NONE',  ( -14.94032676572743767, 24.81194212842451563, -10.66625999421779269 ) ) ;
#11829 = CIRCLE ( 'NONE', #13765, 6.000000000000003553 ) ;
#11830 = CARTESIAN_POINT ( 'NONE',  ( -20.37435360786956551, -23.49902402743817120, 19.27171037444156809 ) ) ;
#11831 = CARTESIAN_POINT ( 'NONE',  ( 12.96194030760161375, -23.08917773356923675, -15.45381493534388717 ) ) ;
#11832 = CARTESIAN_POINT ( 'NONE',  ( 11.16520467992603294, 20.33931832809677331, 6.000000000000000000 ) ) ;
#11833 = CARTESIAN_POINT ( 'NONE',  ( 14.78413089825309434, 25.26060220695678993, -10.65622333237480923 ) ) ;
#11834 = EDGE_LOOP ( 'NONE', ( #2498, #11420, #30736, #38681 ) ) ;
#11835 = CARTESIAN_POINT ( 'NONE',  ( 31.39467639332050553, -19.90237361881552403, -8.844072599137296820 ) ) ;
#11836 = VERTEX_POINT ( 'NONE', #30936 ) ;
#11838 = CARTESIAN_POINT ( 'NONE',  ( 2.247466774197339756, 28.36888560440311480, 13.00000000000000178 ) ) ;
#11837 = CARTESIAN_POINT ( 'NONE',  ( -14.85775003842022102, 28.53279358564904555, -5.466018984421181948 ) ) ;
#11839 = CARTESIAN_POINT ( 'NONE',  ( -17.29263770120802945, -27.09866115540251030, -5.466300565429026648 ) ) ;
#11840 = CARTESIAN_POINT ( 'NONE',  ( 2.605696033269626177, 17.55816537872232530, 6.000000000000000000 ) ) ;
#11841 = ADVANCED_FACE ( 'NONE', ( #24436 ), #17352, .T. ) ;
#11842 = EDGE_LOOP ( 'NONE', ( #9186, #27641, #5574, #35284, #12978 ) ) ;
#11843 = CARTESIAN_POINT ( 'NONE',  ( -33.72599793200199514, -11.57189992363034570, -9.767970167873338383 ) ) ;
#11844 = CARTESIAN_POINT ( 'NONE',  ( -15.28548941152575225, -26.69066991962944257, -5.474153390693990318 ) ) ;
#11845 = CIRCLE ( 'NONE', #35890, 1.000000000000000888 ) ;
#11846 = CARTESIAN_POINT ( 'NONE',  ( 0.000000000000000000, 22.50000000000000355, 7.000000000000000000 ) ) ;
#11847 = ORIENTED_EDGE ( 'NONE', *, *, #34431, .F. ) ;
#11848 = CARTESIAN_POINT ( 'NONE',  ( 28.97648499451679527, 1.995013090243813236, -4.999999999999998224 ) ) ;
#11849 = CYLINDRICAL_SURFACE ( 'NONE', #8320, 1.000000000000000000 ) ;
#11850 = CARTESIAN_POINT ( 'NONE',  ( -39.59914439355220850, -10.88071517532349475, 11.00000000000000000 ) ) ;
#11851 = ORIENTED_EDGE ( 'NONE', *, *, #31236, .T. ) ;
#11852 = CARTESIAN_POINT ( 'NONE',  ( -28.41653591125160006, 0.04529035542138026837, -12.54075237691299094 ) ) ;
#11853 = EDGE_LOOP ( 'NONE', ( #28716, #17661 ) ) ;
#11854 = CARTESIAN_POINT ( 'NONE',  ( 31.92511577782137522, -1.398606727016608042, -6.852345169075132247 ) ) ;
#11855 = CARTESIAN_POINT ( 'NONE',  ( 31.19395790416513847, -3.926110744752351778, 18.42518152272147702 ) ) ;
#11856 = ORIENTED_EDGE ( 'NONE', *, *, #3347, .T. ) ;
#11857 = AXIS2_PLACEMENT_3D ( 'NONE', #20759, #35790, #13843 ) ;
#11858 = CARTESIAN_POINT ( 'NONE',  ( -23.56736984768613041, 3.521302623928285858, -17.71584685096988565 ) ) ;
#11859 = DIRECTION ( 'NONE',  ( 0.05233595624294447302, 0.9986295347545738332, 0.000000000000000000 ) ) ;
#11860 = EDGE_CURVE ( 'NONE', #36229, #39423, #19764, .T. ) ;
#11861 = DIRECTION ( 'NONE',  ( -0.8660254037844433705, -0.4999999999999918399, -0.000000000000000000 ) ) ;
#11862 = VECTOR ( 'NONE', #11450, 1000.000000000000114 ) ;
#11863 = CARTESIAN_POINT ( 'NONE',  ( -37.48531001978128074, -11.24999991186452775, 11.00000000000002309 ) ) ;
#11864 = EDGE_CURVE ( 'NONE', #10191, #8118, #3715, .T. ) ;
#11865 = CYLINDRICAL_SURFACE ( 'NONE', #35069, 0.5000000000000015543 ) ;
#11866 = EDGE_CURVE ( 'NONE', #6906, #31457, #37231, .T. ) ;
#11867 = CARTESIAN_POINT ( 'NONE',  ( -11.68377382812826681, 31.90739031292463679, 7.426391444473273928 ) ) ;
#11868 = CARTESIAN_POINT ( 'NONE',  ( -7.330077540933487512, 17.71145523154927659, 13.00000000000000178 ) ) ;
#11869 = ORIENTED_EDGE ( 'NONE', *, *, #1944, .F. ) ;
#11870 = CARTESIAN_POINT ( 'NONE',  ( -22.91382620985103102, 6.848442421757915177, -14.83700933217039797 ) ) ;
#11871 = DIRECTION ( 'NONE',  ( 0.2079116908177533751, -0.9781476007338067991, 0.000000000000000000 ) ) ;
#11872 = DIRECTION ( 'NONE',  ( 1.000000000000000000, 0.000000000000000000, -0.000000000000000000 ) ) ;
#11873 = CARTESIAN_POINT ( 'NONE',  ( 14.64330500336448004, -14.34584279044560162, -29.99999999999999289 ) ) ;
#11874 = PLANE ( 'NONE',  #7948 ) ;
#11875 = CARTESIAN_POINT ( 'NONE',  ( 10.80899027733819295, 17.41890095272876593, -29.34456996907283610 ) ) ;
#11876 = CARTESIAN_POINT ( 'NONE',  ( -5.096756537559850031, -26.22849730612247754, 13.92931973827808712 ) ) ;
#11877 = ORIENTED_EDGE ( 'NONE', *, *, #37483, .F. ) ;
#11878 = CARTESIAN_POINT ( 'NONE',  ( -16.97879685541396455, 21.84934419274153683, -5.951441372114004480 ) ) ;
#11879 = CARTESIAN_POINT ( 'NONE',  ( -26.17801803039915498, -8.007547698858626717, 20.82122704794079837 ) ) ;
#11880 = AXIS2_PLACEMENT_3D ( 'NONE', #28446, #622, #13003 ) ;
#11881 = CARTESIAN_POINT ( 'NONE',  ( 4.724371395536106633, 32.23037938972932892, 13.00000000000000178 ) ) ;
#11882 = CARTESIAN_POINT ( 'NONE',  ( 15.38118955599525428, 26.63999108931288617, -6.417037871327162968 ) ) ;
#11883 = EDGE_LOOP ( 'NONE', ( #3306, #18465 ) ) ;
#11884 = DIRECTION ( 'NONE',  ( -1.000000000000000000, 0.000000000000000000, 0.000000000000000000 ) ) ;
#11885 = VERTEX_POINT ( 'NONE', #5945 ) ;
#11887 = CARTESIAN_POINT ( 'NONE',  ( -3.476907992048017260, 18.63850621467409496, 13.00000000000000178 ) ) ;
#11886 = CARTESIAN_POINT ( 'NONE',  ( -15.37369053509020667, 26.93276585663874556, -5.000000000000001776 ) ) ;
#11888 = EDGE_CURVE ( 'NONE', #34284, #19377, #30333, .T. ) ;
#11889 = CARTESIAN_POINT ( 'NONE',  ( -14.12857205807981842, -24.62559611294807382, -12.54400053039158713 ) ) ;
#11890 = CARTESIAN_POINT ( 'NONE',  ( 8.927394655428267711, 11.06314620770944757, 11.00000000000000000 ) ) ;
#11891 = EDGE_CURVE ( 'NONE', #11229, #17253, #12803, .T. ) ;
#11892 = VECTOR ( 'NONE', #31691, 1000.000000000000114 ) ;
#11893 = CARTESIAN_POINT ( 'NONE',  ( -27.74053922457303401, -14.52380522957474795, -14.73393910564032616 ) ) ;
#11894 = CARTESIAN_POINT ( 'NONE',  ( -10.35672055835056860, -23.76937265673268840, -13.66394602354463572 ) ) ;
#11895 = DIRECTION ( 'NONE',  ( -0.000000000000000000, -0.000000000000000000, -1.000000000000000000 ) ) ;
#11896 = CARTESIAN_POINT ( 'NONE',  ( 14.86260783703185417, 22.06351504111470874, -13.60475557901546750 ) ) ;
#11897 = ORIENTED_EDGE ( 'NONE', *, *, #4163, .F. ) ;
#11898 = CARTESIAN_POINT ( 'NONE',  ( 22.11552067476606354, 6.995634713880600764, -16.89582745047114543 ) ) ;
#11899 = FACE_OUTER_BOUND ( 'NONE', #31193, .T. ) ;
#11900 = DIRECTION ( 'NONE',  ( 1.000000000000000000, 0.000000000000000000, 0.000000000000000000 ) ) ;
#11901 = DIRECTION ( 'NONE',  ( 0.000000000000000000, 0.000000000000000000, 1.000000000000000000 ) ) ;
#11902 = EDGE_LOOP ( 'NONE', ( #3787, #3404, #32805, #24027 ) ) ;
#11903 = CARTESIAN_POINT ( 'NONE',  ( -31.05298752102547155, -0.7743630725552020921, -8.259985541401292153 ) ) ;
#11904 = CIRCLE ( 'NONE', #20312, 1.000000000000000000 ) ;
#11905 = CARTESIAN_POINT ( 'NONE',  ( 25.29308743037763918, 0.2312469298496797332, -17.41904786010038109 ) ) ;
#11906 = CARTESIAN_POINT ( 'NONE',  ( -5.034171952701847808, 35.03623199971306690, 7.000000000000000000 ) ) ;
#11907 = CARTESIAN_POINT ( 'NONE',  ( 25.92581632124332458, -14.96827703203057958, 20.82122704794079837 ) ) ;
#11908 = CARTESIAN_POINT ( 'NONE',  ( -10.79456899466765840, 1.678572790138225468, 10.00000000000000000 ) ) ;
#11909 = EDGE_CURVE ( 'NONE', #24813, #21291, #25762, .T. ) ;
#11910 = AXIS2_PLACEMENT_3D ( 'NONE', #36559, #23968, #36163 ) ;
#11911 = CARTESIAN_POINT ( 'NONE',  ( 9.911438049897887126, 11.24107483890952075, 7.000000000000000000 ) ) ;
#11912 = EDGE_CURVE ( 'NONE', #1084, #2141, #37425, .T. ) ;
#11913 =( GEOMETRIC_REPRESENTATION_CONTEXT ( 3 ) GLOBAL_UNCERTAINTY_ASSIGNED_CONTEXT ( ( #16904 ) ) GLOBAL_UNIT_ASSIGNED_CONTEXT ( ( #13606, #19500, #32516 ) ) REPRESENTATION_CONTEXT ( 'NONE', 'WORKASPACE' ) );
#11914 = ORIENTED_EDGE ( 'NONE', *, *, #33173, .T. ) ;
#11915 = CARTESIAN_POINT ( 'NONE',  ( -10.54147634889124063, 27.59512447410525127, 6.000000000000000000 ) ) ;
#11916 = DIRECTION ( 'NONE',  ( -0.000000000000000000, -0.000000000000000000, -1.000000000000000000 ) ) ;
#11917 = LINE ( 'NONE', #21259, #18405 ) ;
#11918 = CARTESIAN_POINT ( 'NONE',  ( 3.596573278996550993, 34.97522925885748180, -11.08051460049237491 ) ) ;
#11919 = CARTESIAN_POINT ( 'NONE',  ( 8.910254037844364206, 17.93301270189218499, 10.50000000000000000 ) ) ;
#11920 = CARTESIAN_POINT ( 'NONE',  ( 2.568190708544436429, 12.82247983807081226, 10.50000000000000000 ) ) ;
#11921 = B_SPLINE_CURVE_WITH_KNOTS ( 'NONE', 3,
 ( #31199, #22439, #6214, #6796 ),
 .UNSPECIFIED., .F., .F.,
 ( 4, 4 ),
 ( 0.000000000000000000, 1.000000000000000000 ),
 .UNSPECIFIED. ) ;
#11922 = CARTESIAN_POINT ( 'NONE',  ( -10.72918489117944674, 32.98258515686310943, 7.500000000000004441 ) ) ;
#11923 = DIRECTION ( 'NONE',  ( 1.000000000000000000, 0.000000000000000000, 0.000000000000000000 ) ) ;
#11924 = DIRECTION ( 'NONE',  ( -1.000000000000000000, 0.000000000000000000, 0.000000000000000000 ) ) ;
#11925 = DIRECTION ( 'NONE',  ( 0.000000000000000000, 0.000000000000000000, 1.000000000000000000 ) ) ;
#11926 = CARTESIAN_POINT ( 'NONE',  ( 14.69098151597639834, 28.78426858804810351, -5.926310556595937307 ) ) ;
#11927 = CARTESIAN_POINT ( 'NONE',  ( 9.911438049897887126, 11.24107483890952075, 7.000000000000000000 ) ) ;
#11928 = EDGE_LOOP ( 'NONE', ( #31123, #8584, #25941 ) ) ;
#11930 = CARTESIAN_POINT ( 'NONE',  ( -5.187504188494229673, 36.60991850771488032, 10.49999999999999822 ) ) ;
#11929 = CARTESIAN_POINT ( 'NONE',  ( -16.52500823362143834, 12.50774690784832543, -26.60145339744036264 ) ) ;
#11931 = AXIS2_PLACEMENT_3D ( 'NONE', #28542, #919, #4360 ) ;
#11932 = CARTESIAN_POINT ( 'NONE',  ( -13.95827473762437165, 27.56104949980369412, 10.87262190629278535 ) ) ;
#11933 = CARTESIAN_POINT ( 'NONE',  ( 9.631034963941338845, -18.33589862961692774, -27.44708460917885517 ) ) ;
#11934 = CARTESIAN_POINT ( 'NONE',  ( -18.50896748101629541, -23.35909915790261948, -14.08898525485408904 ) ) ;
#11935 = CARTESIAN_POINT ( 'NONE',  ( 12.39413036303996307, 20.48625930257312433, -19.49701620399656932 ) ) ;
#11936 = CARTESIAN_POINT ( 'NONE',  ( 11.87498658133518248, 19.40059169592226240, -21.61373574364315076 ) ) ;
#11937 = ORIENTED_EDGE ( 'NONE', *, *, #16154, .T. ) ;
#11938 = CARTESIAN_POINT ( 'NONE',  ( 11.31392148919589680, 36.91540483778863546, -14.26382729546508088 ) ) ;
#11939 = CARTESIAN_POINT ( 'NONE',  ( -5.330077540933487512, 17.71145523154927659, 13.00000000000000178 ) ) ;
#11940 = COLOUR_RGB ( '', 0.66274510, 0.83137255, 0.94901961) ;
#11941 = CARTESIAN_POINT ( 'NONE',  ( -28.00154710540513392, -23.35202446123746256, -8.873473656866229575 ) ) ;
#11942 = CARTESIAN_POINT ( 'NONE',  ( -0.2676006149246174526, -20.58428938002466779, -27.73625193941130007 ) ) ;
#11943 = CARTESIAN_POINT ( 'NONE',  ( 15.58410715161808824, 26.18909738223269557, -5.000000000000000888 ) ) ;
#11944 = CARTESIAN_POINT ( 'NONE',  ( 19.35653844823029246, 10.81242967103833763, -19.06682279225362819 ) ) ;
#11945 = CARTESIAN_POINT ( 'NONE',  ( 8.816778784387034662, 10.36474508437574471, 7.000000000000000000 ) ) ;
#11946 = EDGE_CURVE ( 'NONE', #20669, #15620, #26712, .T. ) ;
#11947 = CARTESIAN_POINT ( 'NONE',  ( -2.848530395113701985, 20.31062432315956201, -29.22165717386838679 ) ) ;
#11948 = VERTEX_POINT ( 'NONE', #1054 ) ;
#11949 = CARTESIAN_POINT ( 'NONE',  ( -34.69811016863992137, -6.555196379703267517, -6.328619236691829464 ) ) ;
#11950 = VECTOR ( 'NONE', #16813, 1000.000000000000000 ) ;
#11951 = CARTESIAN_POINT ( 'NONE',  ( -25.71480618105703542, 9.014447550988780478, 11.55979286844120324 ) ) ;
#11952 = ORIENTED_EDGE ( 'NONE', *, *, #29393, .F. ) ;
#11953 = DIRECTION ( 'NONE',  ( 1.000000000000000000, 0.000000000000000000, 0.000000000000000000 ) ) ;
#11954 = FACE_OUTER_BOUND ( 'NONE', #35016, .T. ) ;
#11955 = CARTESIAN_POINT ( 'NONE',  ( -29.42040707488883555, 0.4686144674514792219, -9.717579686123906768 ) ) ;
#11956 = CARTESIAN_POINT ( 'NONE',  ( 26.94378894143373770, -9.905954980331337367, -16.69510737975683057 ) ) ;
#11957 = CIRCLE ( 'NONE', #17165, 0.4999999999999999445 ) ;
#11958 = ORIENTED_EDGE ( 'NONE', *, *, #34357, .F. ) ;
#11959 = DIRECTION ( 'NONE',  ( 0.000000000000000000, 0.000000000000000000, 1.000000000000000000 ) ) ;
#11960 = VERTEX_POINT ( 'NONE', #28675 ) ;
#11961 = CARTESIAN_POINT ( 'NONE',  ( 8.927394655428276593, 11.06314620770945290, 7.000000000000000000 ) ) ;
#11962 = DIRECTION ( 'NONE',  ( 0.000000000000000000, 0.000000000000000000, 1.000000000000000000 ) ) ;
#11963 = CIRCLE ( 'NONE', #22334, 1.000000000000002665 ) ;
#11964 = LINE ( 'NONE', #30659, #28527 ) ;
#11965 = ORIENTED_EDGE ( 'NONE', *, *, #19795, .F. ) ;
#11966 = PRESENTATION_STYLE_ASSIGNMENT (( #11169 ) ) ;
#11967 = CARTESIAN_POINT ( 'NONE',  ( -3.829842517469123298, 8.490119531707978950, 10.66666666666666785 ) ) ;
#11968 = FACE_OUTER_BOUND ( 'NONE', #16392, .T. ) ;
#11969 = CARTESIAN_POINT ( 'NONE',  ( 4.444273797880263110, 24.85496137639062297, 23.00000000000000355 ) ) ;
#11970 = CARTESIAN_POINT ( 'NONE',  ( 16.27615822911637622, -12.47890632334475747, -29.22043922964566676 ) ) ;
#11971 = CARTESIAN_POINT ( 'NONE',  ( 17.93403218016955591, 14.29091524181443518, -16.94358179346269466 ) ) ;
#11972 = CARTESIAN_POINT ( 'NONE',  ( 7.524521118624930338, 19.14141286767502947, -28.57295515480274517 ) ) ;
#11973 = CIRCLE ( 'NONE', #19104, 1.000000000000000888 ) ;
#11974 = ORIENTED_EDGE ( 'NONE', *, *, #27882, .F. ) ;
#11975 = CARTESIAN_POINT ( 'NONE',  ( -18.67511144159872316, 8.486512637698147898, -29.42713777807604458 ) ) ;
#11976 = CARTESIAN_POINT ( 'NONE',  ( 14.31603901957230462, 19.98981538725069740, 7.500000000000010658 ) ) ;
#11977 = CARTESIAN_POINT ( 'NONE',  ( 13.88701526290651422, -24.14100214001190281, -13.49798790650252833 ) ) ;
#11978 = DIRECTION ( 'NONE',  ( 1.000000000000000000, 0.000000000000000000, 0.000000000000000000 ) ) ;
#11979 = CARTESIAN_POINT ( 'NONE',  ( 3.784955426773477072, 9.502919080911359728, 9.500000000000000000 ) ) ;
#11980 = CARTESIAN_POINT ( 'NONE',  ( -11.04466200716893276, 17.52154582185139020, -27.44559064709055818 ) ) ;
#11981 = CARTESIAN_POINT ( 'NONE',  ( -18.24003512488236467, -21.72694636099543075, -15.96283982311370941 ) ) ;
#11982 = CARTESIAN_POINT ( 'NONE',  ( 13.09383889318130301, -26.15137312895040722, -5.947571630415806609 ) ) ;
#11983 = EDGE_CURVE ( 'NONE', #26378, #26489, #16703, .T. ) ;
#11984 = CARTESIAN_POINT ( 'NONE',  ( -0.4999999999999998890, 37.00000000000000711, 11.00000000000000000 ) ) ;
#11985 = ORIENTED_EDGE ( 'NONE', *, *, #21993, .T. ) ;
#11986 = ORIENTED_EDGE ( 'NONE', *, *, #35923, .T. ) ;
#11987 = CARTESIAN_POINT ( 'NONE',  ( -9.942109246833966907, 33.34287839135563303, -9.382223997254289571 ) ) ;
#11988 = CARTESIAN_POINT ( 'NONE',  ( -14.44622163125246850, 19.97613264340537143, 10.49999999999999645 ) ) ;
#11989 = DIRECTION ( 'NONE',  ( 0.000000000000000000, 0.000000000000000000, 1.000000000000000000 ) ) ;
#11990 = CIRCLE ( 'NONE', #25583, 6.000000000000008882 ) ;
#11991 = DIRECTION ( 'NONE',  ( -0.1045284632676437703, 0.9945218953682745111, 0.000000000000000000 ) ) ;
#11992 = ORIENTED_EDGE ( 'NONE', *, *, #30112, .T. ) ;
#11993 = CARTESIAN_POINT ( 'NONE',  ( 27.14326651887064656, 0.2312572436680407628, -14.47629528729547133 ) ) ;
#11994 = EDGE_CURVE ( 'NONE', #9244, #24567, #28476, .T. ) ;
#11995 = FACE_OUTER_BOUND ( 'NONE', #32202, .T. ) ;
#11996 = DIRECTION ( 'NONE',  ( -0.000000000000000000, -0.000000000000000000, 1.000000000000000000 ) ) ;
#11997 = EDGE_CURVE ( 'NONE', #22687, #7930, #38627, .T. ) ;
#11998 = ORIENTED_EDGE ( 'NONE', *, *, #22309, .F. ) ;
#11999 = AXIS2_PLACEMENT_3D ( 'NONE', #12125, #15370, #30014 ) ;
#12000 = CARTESIAN_POINT ( 'NONE',  ( -28.33198621730845446, 0.1486562545012954650, -12.55068749093940639 ) ) ;
#12001 = DIRECTION ( 'NONE',  ( -1.000000000000000000, 0.000000000000000000, 0.000000000000000000 ) ) ;
#12002 = ORIENTED_EDGE ( 'NONE', *, *, #34823, .F. ) ;
#12003 = CARTESIAN_POINT ( 'NONE',  ( 26.67980387914269969, -3.134049882918540142, -17.05610665002131299 ) ) ;
#12004 = CIRCLE ( 'NONE', #34704, 22.50000000000000355 ) ;
#12005 = ORIENTED_EDGE ( 'NONE', *, *, #24548, .T. ) ;
#12006 = CARTESIAN_POINT ( 'NONE',  ( -5.726446540400362828, 39.49945686212554818, 12.14047268033097104 ) ) ;
#12007 = CARTESIAN_POINT ( 'NONE',  ( 4.332433290453930557E-14, -14.56650175400723946, 20.99999999999999645 ) ) ;
#12008 = LINE ( 'NONE', #36593, #4621 ) ;
#12009 = CARTESIAN_POINT ( 'NONE',  ( -0.9851783940330662848, 31.60047892813803827, 20.50957957746028626 ) ) ;
#12010 = DIRECTION ( 'NONE',  ( 1.000000000000000000, 0.000000000000000000, 0.000000000000000000 ) ) ;
#12011 = VERTEX_POINT ( 'NONE', #19532 ) ;
#12012 = CARTESIAN_POINT ( 'NONE',  ( -16.24129362380271857, 27.01431713449521510, 15.13084544680213384 ) ) ;
#12013 = ADVANCED_FACE ( 'NONE', ( #13433 ), #23193, .T. ) ;
#12014 = CARTESIAN_POINT ( 'NONE',  ( -15.41558956984166251, 26.78481017248024898, -5.000000000000000000 ) ) ;
#12015 = EDGE_CURVE ( 'NONE', #4321, #14003, #10801, .T. ) ;
#12016 = VECTOR ( 'NONE', #38355, 999.9999999999998863 ) ;
#12017 = CARTESIAN_POINT ( 'NONE',  ( 4.106875433146082166, 25.19931270338924989, -19.70517226477189965 ) ) ;
#12018 = LINE ( 'NONE', #24206, #20408 ) ;
#12019 = CARTESIAN_POINT ( 'NONE',  ( -3.713592597587352717, 7.966960743906856379, 7.499999999999997335 ) ) ;
#12020 = CARTESIAN_POINT ( 'NONE',  ( 10.69198779663409304, -17.56583795296588235, -28.65972484765404005 ) ) ;
#12021 = AXIS2_PLACEMENT_3D ( 'NONE', #39900, #30577, #27709 ) ;
#12022 = DIRECTION ( 'NONE',  ( 1.000000000000000000, 0.000000000000000000, 0.000000000000000000 ) ) ;
#12023 = FACE_OUTER_BOUND ( 'NONE', #10094, .T. ) ;
#12024 = ORIENTED_EDGE ( 'NONE', *, *, #36372, .F. ) ;
#12025 = ORIENTED_EDGE ( 'NONE', *, *, #24746, .T. ) ;
#12026 = AXIS2_PLACEMENT_3D ( 'NONE', #36849, #21209, #33619 ) ;
#12027 = CARTESIAN_POINT ( 'NONE',  ( -14.95102318841846412, 25.74959356765882390, -9.709746325769389230 ) ) ;
#12028 = CIRCLE ( 'NONE', #6822, 0.5000000000000002220 ) ;
#12029 = CARTESIAN_POINT ( 'NONE',  ( -29.28423149095540978, -1.632116715642781823, 18.42518152272108978 ) ) ;
#12030 = CARTESIAN_POINT ( 'NONE',  ( 9.727834406736230122, -18.58976127751570573, -26.23031535258787628 ) ) ;
#12031 = CARTESIAN_POINT ( 'NONE',  ( -3.781037291632698416, 7.996959361763665619, 10.49999999999999822 ) ) ;
#12032 = ORIENTED_EDGE ( 'NONE', *, *, #13963, .F. ) ;
#12033 = ORIENTED_EDGE ( 'NONE', *, *, #12514, .T. ) ;
#12035 = CARTESIAN_POINT ( 'NONE',  ( -6.557822374958138134, 35.99981354310120452, 10.49999999999999822 ) ) ;
#12034 = CARTESIAN_POINT ( 'NONE',  ( -10.51657528416702370, 20.72986206170195800, -21.37251766699545996 ) ) ;
#12036 = CARTESIAN_POINT ( 'NONE',  ( -18.32806035864107841, -25.83311609833614853, -10.45574956145189560 ) ) ;
#12037 = EDGE_CURVE ( 'NONE', #13902, #35341, #18044, .T. ) ;
#12038 = DIRECTION ( 'NONE',  ( -1.000000000000000000, 0.000000000000000000, 0.000000000000000000 ) ) ;
#12039 = EDGE_LOOP ( 'NONE', ( #22325, #26671 ) ) ;
#12040 = CARTESIAN_POINT ( 'NONE',  ( -33.38534935071415788, -11.45126148588078330, -10.21694987028886636 ) ) ;
#12041 = CARTESIAN_POINT ( 'NONE',  ( -12.38214629039859282, -22.55476777646130415, -16.46447605962150362 ) ) ;
#12042 = CARTESIAN_POINT ( 'NONE',  ( 18.77248997590679735, -31.35432035705766651, 11.00000000000000000 ) ) ;
#12043 = ORIENTED_EDGE ( 'NONE', *, *, #3219, .T. ) ;
#12044 = CARTESIAN_POINT ( 'NONE',  ( 28.68541928171654831, 0.3475515138929626269, -11.60796932871038756 ) ) ;
#12045 = CARTESIAN_POINT ( 'NONE',  ( -12.80736835487442349, 15.68301270189233954, 7.000000000000000000 ) ) ;
#12046 = CARTESIAN_POINT ( 'NONE',  ( 33.75875814100314187, 2.759858869446413010, 23.00000000000000000 ) ) ;
#12047 = ORIENTED_EDGE ( 'NONE', *, *, #7492, .T. ) ;
#12048 = CARTESIAN_POINT ( 'NONE',  ( -30.93630827890108037, -0.1109845943994294815, -5.945062553525370497 ) ) ;
#12049 = VERTEX_POINT ( 'NONE', #22575 ) ;
#12050 = CARTESIAN_POINT ( 'NONE',  ( 20.72896443152828283, 0.1975693286415366734, -27.40608702327256907 ) ) ;
#12051 = CARTESIAN_POINT ( 'NONE',  ( 20.52459090776396167, -25.56956579041154498, 17.92354375535250810 ) ) ;
#12052 = ORIENTED_EDGE ( 'NONE', *, *, #2319, .T. ) ;
#12053 = CARTESIAN_POINT ( 'NONE',  ( -20.56177667423478894, 2.892092975756595408, -26.97112085952661431 ) ) ;
#12054 = AXIS2_PLACEMENT_3D ( 'NONE', #20588, #11040, #23424 ) ;
#12055 = DIRECTION ( 'NONE',  ( -1.000000000000000000, 0.000000000000000000, 0.000000000000000000 ) ) ;
#12056 = DIRECTION ( 'NONE',  ( -0.000000000000000000, -0.000000000000000000, 1.000000000000000000 ) ) ;
#12057 = AXIS2_PLACEMENT_3D ( 'NONE', #24318, #18425, #2589 ) ;
#12058 = CIRCLE ( 'NONE', #34763, 0.9999999999999998890 ) ;
#12059 = CARTESIAN_POINT ( 'NONE',  ( -14.98890121934603314, -28.67928442654204346, 11.00000000000000000 ) ) ;
#12060 = DIRECTION ( 'NONE',  ( 0.000000000000000000, 0.000000000000000000, 1.000000000000000000 ) ) ;
#12061 = EDGE_CURVE ( 'NONE', #18383, #16182, #32547, .T. ) ;
#12062 = FACE_BOUND ( 'NONE', #37572, .T. ) ;
#12063 = CARTESIAN_POINT ( 'NONE',  ( 37.48557158514985588, -11.25000000000009415, -5.000000000000000000 ) ) ;
#12064 = ORIENTED_EDGE ( 'NONE', *, *, #3943, .T. ) ;
#12065 = CARTESIAN_POINT ( 'NONE',  ( -20.93482781216526689, 6.580497575008867450, -21.07328139004194156 ) ) ;
#12066 = FACE_OUTER_BOUND ( 'NONE', #26831, .T. ) ;
#12067 = DIRECTION ( 'NONE',  ( -0.000000000000000000, -0.000000000000000000, -1.000000000000000000 ) ) ;
#12068 = B_SPLINE_CURVE_WITH_KNOTS ( 'NONE', 3,
 ( #37094, #27746, #31584, #15752, #25294, #34250 ),
 .UNSPECIFIED., .F., .F.,
 ( 4, 2, 4 ),
 ( 0.000000000000000000, 0.5000000000000000000, 1.000000000000000000 ),
 .UNSPECIFIED. ) ;
#12069 = CARTESIAN_POINT ( 'NONE',  ( 15.08063968188699633, -13.89948965651085544, -29.99999999999999645 ) ) ;
#12070 = DIRECTION ( 'NONE',  ( 0.000000000000000000, -0.6216356077939705349, -0.7833065626704661666 ) ) ;
#12071 = CARTESIAN_POINT ( 'NONE',  ( 14.74369174452469089, 25.90307666149954713, -10.16263518668779398 ) ) ;
#12072 = CARTESIAN_POINT ( 'NONE',  ( -10.15481549915472570, -27.08512292516926223, 13.32518128617831010 ) ) ;
#12073 = ORIENTED_EDGE ( 'NONE', *, *, #7911, .F. ) ;
#12074 = CARTESIAN_POINT ( 'NONE',  ( -12.35093606704898228, 16.57560007382403455, -27.53901265143020183 ) ) ;
#12075 = CARTESIAN_POINT ( 'NONE',  ( -19.27923559247379970, -17.06979493269815151, 21.00000000000004619 ) ) ;
#12076 = CARTESIAN_POINT ( 'NONE',  ( 12.74038105676654453, 14.56698729810772264, 10.49999999999999822 ) ) ;
#12077 = CARTESIAN_POINT ( 'NONE',  ( 13.50121191754509908, 22.79660094963672634, -15.45185408499526680 ) ) ;
#12078 = ORIENTED_EDGE ( 'NONE', *, *, #12965, .F. ) ;
#12079 = CYLINDRICAL_SURFACE ( 'NONE', #11253, 1.000000000000000000 ) ;
#12080 = VERTEX_POINT ( 'NONE', #34985 ) ;
#12081 = AXIS2_PLACEMENT_3D ( 'NONE', #16277, #31518, #6520 ) ;
#12083 = DIRECTION ( 'NONE',  ( -0.000000000000000000, -0.000000000000000000, -1.000000000000000000 ) ) ;
#12082 = CARTESIAN_POINT ( 'NONE',  ( -13.71542125295547088, 23.51752206020428915, -14.46353376464415774 ) ) ;
#12084 = CARTESIAN_POINT ( 'NONE',  ( -10.63009531068781577, -19.54863766215186516, -22.72267709242899869 ) ) ;
#12085 = EDGE_CURVE ( 'NONE', #33602, #13627, #18670, .T. ) ;
#12086 = DIRECTION ( 'NONE',  ( 0.000000000000000000, 0.000000000000000000, 1.000000000000000000 ) ) ;
#12087 = AXIS2_PLACEMENT_3D ( 'NONE', #11095, #2354, #1752 ) ;
#12088 = CARTESIAN_POINT ( 'NONE',  ( -30.07688550757283608, -16.93187886526812136, -11.97280104394458711 ) ) ;
#12089 = CARTESIAN_POINT ( 'NONE',  ( -10.49402848346364259, -21.11063220854802935, -19.60472159036592288 ) ) ;
#12090 = CARTESIAN_POINT ( 'NONE',  ( -14.92615392307458144, 21.72537115092790216, 10.49999999999999822 ) ) ;
#12091 = CARTESIAN_POINT ( 'NONE',  ( 12.89744199737797992, 19.01286579302862734, -20.67027483038949498 ) ) ;
#12093 = ADVANCED_FACE ( 'NONE', ( #16091 ), #26026, .T. ) ;
#12092 = VERTEX_POINT ( 'NONE', #10598 ) ;
#12094 = CARTESIAN_POINT ( 'NONE',  ( 21.14538636724398657, 6.850996120451639193, -20.02713119748161930 ) ) ;
#12095 = AXIS2_PLACEMENT_3D ( 'NONE', #19411, #22652, #34267 ) ;
#12096 = DIRECTION ( 'NONE',  ( 1.000000000000000000, 0.000000000000000000, 0.000000000000000000 ) ) ;
#12097 = EDGE_CURVE ( 'NONE', #3986, #38536, #22372, .T. ) ;
#12098 = DIRECTION ( 'NONE',  ( 0.000000000000000000, 0.000000000000000000, 1.000000000000000000 ) ) ;
#12099 = CARTESIAN_POINT ( 'NONE',  ( -13.94482798346716201, 26.50521816028930999, 7.000000000000000000 ) ) ;
#12100 = ORIENTED_EDGE ( 'NONE', *, *, #33127, .T. ) ;
#12101 = CARTESIAN_POINT ( 'NONE',  ( -31.86521589244229702, -1.232139016781935492, -6.393609547768853929 ) ) ;
#12102 = CARTESIAN_POINT ( 'NONE',  ( 23.96264080723695500, 0.4348472519531068614, -19.48932385422077118 ) ) ;
#12103 = EDGE_CURVE ( 'NONE', #8501, #1841, #19326, .T. ) ;
#12104 = DIRECTION ( 'NONE',  ( 1.000000000000000000, 0.000000000000000000, 0.000000000000000000 ) ) ;
#12105 = CARTESIAN_POINT ( 'NONE',  ( 26.64268929643274930, -15.38216383723093550, 20.69868183039781329 ) ) ;
#12106 = CARTESIAN_POINT ( 'NONE',  ( -14.47283171447380035, 21.48159823030330884, 7.000000000000000000 ) ) ;
#12107 = DIRECTION ( 'NONE',  ( 0.000000000000000000, 0.000000000000000000, 1.000000000000000000 ) ) ;
#12108 = ORIENTED_EDGE ( 'NONE', *, *, #21156, .F. ) ;
#12109 = EDGE_CURVE ( 'NONE', #1553, #30133, #31653, .T. ) ;
#12110 = CARTESIAN_POINT ( 'NONE',  ( -5.490944681523147075, 34.83286367817517259, 7.000000000000000000 ) ) ;
#12111 = ADVANCED_FACE ( 'NONE', ( #19334 ), #32133, .F. ) ;
#12112 = EDGE_CURVE ( 'NONE', #33136, #17440, #13459, .T. ) ;
#12113 = AXIS2_PLACEMENT_3D ( 'NONE', #36881, #8855, #32849 ) ;
#12114 = AXIS2_PLACEMENT_3D ( 'NONE', #23019, #4538, #34614 ) ;
#12115 = DIRECTION ( 'NONE',  ( 1.000000000000000000, 0.000000000000000000, 0.000000000000000000 ) ) ;
#12116 = LINE ( 'NONE', #18617, #28771 ) ;
#12117 = CARTESIAN_POINT ( 'NONE',  ( 2.078853377173544903, 28.96599879814208123, -16.63595397449693536 ) ) ;
#12118 = DIRECTION ( 'NONE',  ( 0.000000000000000000, 0.000000000000000000, 1.000000000000000000 ) ) ;
#12119 = LINE ( 'NONE', #27555, #8485 ) ;
#12120 = CARTESIAN_POINT ( 'NONE',  ( 5.362728154695969529, 13.41753630677055753, 11.00000000000000000 ) ) ;
#12121 = CARTESIAN_POINT ( 'NONE',  ( -14.47283171447380390, 21.48159823030330884, 7.000000000000000000 ) ) ;
#12122 = DIRECTION ( 'NONE',  ( -0.000000000000000000, -0.000000000000000000, -1.000000000000000000 ) ) ;
#12123 = CARTESIAN_POINT ( 'NONE',  ( 14.09933648065468503, 26.02968990214155198, 10.50000000000000533 ) ) ;
#12124 = CARTESIAN_POINT ( 'NONE',  ( 14.81731206233621023, 27.65607728349727523, -7.787956928312406824 ) ) ;
#12125 = CARTESIAN_POINT ( 'NONE',  ( -10.44103466624267185, 32.57396620494226624, 7.000000000000000000 ) ) ;
#12126 = ORIENTED_EDGE ( 'NONE', *, *, #31722, .T. ) ;
#12128 = DIRECTION ( 'NONE',  ( 0.9135454576426059736, 0.4067366430757888285, 0.000000000000000000 ) ) ;
#12127 = CARTESIAN_POINT ( 'NONE',  ( -17.62030008941222547, 17.79749385453288113, -11.80820510887239827 ) ) ;
#12129 = CARTESIAN_POINT ( 'NONE',  ( -14.48927117870122316, -30.61587158504648087, 11.00000000000000000 ) ) ;
#12130 = CARTESIAN_POINT ( 'NONE',  ( 15.15893967609533455, -26.27887000457485200, -8.297842270817525900 ) ) ;
#12131 = CARTESIAN_POINT ( 'NONE',  ( -12.63282099796252034, -16.15870876741617579, -29.28150700448700405 ) ) ;
#12132 = CARTESIAN_POINT ( 'NONE',  ( 15.10138251737945936, 26.13808434145727944, -8.767643565617390777 ) ) ;
#12133 = CARTESIAN_POINT ( 'NONE',  ( 10.99175044165756709, 17.35733570206949494, -28.70635921313413164 ) ) ;
#12134 = VERTEX_POINT ( 'NONE', #19943 ) ;
#12135 = CARTESIAN_POINT ( 'NONE',  ( -4.003793318659595535, 8.455722206104626437, 10.49999999999999822 ) ) ;
#12136 = CARTESIAN_POINT ( 'NONE',  ( 36.53988292926447912, -0.5802930198997262590, 11.00000000000000178 ) ) ;
#12137 = EDGE_CURVE ( 'NONE', #34496, #34284, #1455, .T. ) ;
#12138 = CARTESIAN_POINT ( 'NONE',  ( -18.88614099607083929, -28.19481782898740718, 15.13084544680256549 ) ) ;
#12139 = CARTESIAN_POINT ( 'NONE',  ( -18.83962338116515056, -15.66599860280581602, -20.78005700281575230 ) ) ;
#12140 = CARTESIAN_POINT ( 'NONE',  ( -0.3299534963231213758, -22.70197746772678826, -16.98173616913636508 ) ) ;
#12141 = CARTESIAN_POINT ( 'NONE',  ( 13.76173484786665391, 22.29158688768309560, -15.48881288112352017 ) ) ;
#12142 = ADVANCED_FACE ( 'NONE', ( #2461 ), #23988, .T. ) ;
#12143 = CARTESIAN_POINT ( 'NONE',  ( 17.53305258709997716, 10.68547909316169608, -28.86305607330305634 ) ) ;
#12144 = CARTESIAN_POINT ( 'NONE',  ( 2.485571585149743523, -11.24999999999995737, 6.000000000000000000 ) ) ;
#12145 = CARTESIAN_POINT ( 'NONE',  ( -5.326384147119485490, 37.63231972733477448, -5.437470600199088899 ) ) ;
#12146 = ORIENTED_EDGE ( 'NONE', *, *, #25395, .F. ) ;
#12147 = CARTESIAN_POINT ( 'NONE',  ( -20.17828169183510667, -3.673208557823401943, -30.00000000000000355 ) ) ;
#12148 = CIRCLE ( 'NONE', #15356, 1.000000000000000888 ) ;
#12149 = AXIS2_PLACEMENT_3D ( 'NONE', #38166, #10335, #22716 ) ;
#12150 = CARTESIAN_POINT ( 'NONE',  ( -17.28285333401127133, 27.30382183499614612, 12.14047268033097460 ) ) ;
#12151 = VERTEX_POINT ( 'NONE', #5493 ) ;
#12152 = CARTESIAN_POINT ( 'NONE',  ( 2.605696033269626177, 17.55816537872232530, 13.00000000000000178 ) ) ;
#12153 = LINE ( 'NONE', #24543, #27144 ) ;
#12154 = CARTESIAN_POINT ( 'NONE',  ( -28.36600098059368236, 0.7354731085742703955, -11.62209496411426812 ) ) ;
#12155 = CARTESIAN_POINT ( 'NONE',  ( 19.43389763942624882, -6.523976669268586548, -29.23235429811387576 ) ) ;
#12156 = VECTOR ( 'NONE', #14968, 1000.000000000000000 ) ;
#12157 = ORIENTED_EDGE ( 'NONE', *, *, #20055, .T. ) ;
#12158 = LINE ( 'NONE', #28189, #27807 ) ;
#12159 = ORIENTED_EDGE ( 'NONE', *, *, #11715, .T. ) ;
#12160 = CARTESIAN_POINT ( 'NONE',  ( -9.625795778762141097, 10.95253033666833709, 11.00000000000000000 ) ) ;
#12161 = DIRECTION ( 'NONE',  ( -0.7431448254773862505, 0.6691306063588670083, 0.000000000000000000 ) ) ;
#12162 = CARTESIAN_POINT ( 'NONE',  ( -4.100643064501314328, 15.70406341247269211, 6.000000000000000000 ) ) ;
#12163 = ORIENTED_EDGE ( 'NONE', *, *, #4437, .F. ) ;
#12164 = CARTESIAN_POINT ( 'NONE',  ( -2.944636116024315520, 26.57046322055783349, -18.64425712812955993 ) ) ;
#12165 = FACE_OUTER_BOUND ( 'NONE', #36868, .T. ) ;
#12166 = DIRECTION ( 'NONE',  ( 0.9510565162951543083, 0.3090169943749450088, 0.000000000000000000 ) ) ;
#12167 = CARTESIAN_POINT ( 'NONE',  ( -3.399837471815634338, 8.909889435135630364, 7.499999999999997335 ) ) ;
#12168 = CARTESIAN_POINT ( 'NONE',  ( 18.29362116886485978, -14.93416125425190977, -21.91937720398613720 ) ) ;
#12169 = CARTESIAN_POINT ( 'NONE',  ( 15.76482823105918385, 13.10325120709816105, -29.42076664285941590 ) ) ;
#12170 = VECTOR ( 'NONE', #14902, 1000.000000000000000 ) ;
#12171 = CARTESIAN_POINT ( 'NONE',  ( 11.09465891820651784, 26.43777197077398355, -15.08134290002067246 ) ) ;
#12172 = AXIS2_PLACEMENT_3D ( 'NONE', #33453, #26938, #36291 ) ;
#12173 = VERTEX_POINT ( 'NONE', #17511 ) ;
#12174 = CARTESIAN_POINT ( 'NONE',  ( -21.78527990638771072, 10.57721431994490935, -10.88166847450601438 ) ) ;
#12175 = DIRECTION ( 'NONE',  ( 0.000000000000000000, 0.000000000000000000, 1.000000000000000000 ) ) ;
#12176 = CARTESIAN_POINT ( 'NONE',  ( 14.93814303287626544, -25.69500553019197042, -10.16968976574983685 ) ) ;
#12177 = DIRECTION ( 'NONE',  ( 1.000000000000000000, 0.000000000000000000, 0.000000000000000000 ) ) ;
#12178 = CIRCLE ( 'NONE', #18653, 6.000000000000014211 ) ;
#12179 = CARTESIAN_POINT ( 'NONE',  ( -16.77267017469754151, -29.13948811618693924, -5.000000000000000000 ) ) ;
#12180 = VECTOR ( 'NONE', #31182, 1000.000000000000000 ) ;
#12181 = CARTESIAN_POINT ( 'NONE',  ( -15.35363586822866289, 26.73755632045413932, -6.416160081111284441 ) ) ;
#12182 = CARTESIAN_POINT ( 'NONE',  ( -23.85290253531346849, -26.59866202527626555, -5.885430692555547516 ) ) ;
#12183 = CARTESIAN_POINT ( 'NONE',  ( 10.51335036728116279, -22.08948547754980751, -17.58519077309815870 ) ) ;
#12184 = CARTESIAN_POINT ( 'NONE',  ( 11.48173768534048556, 32.16538668264401934, 10.59344438985533721 ) ) ;
#12185 = EDGE_LOOP ( 'NONE', ( #19982, #30143, #13749, #14442 ) ) ;
#12186 = ORIENTED_EDGE ( 'NONE', *, *, #17363, .T. ) ;
#12187 = CARTESIAN_POINT ( 'NONE',  ( -10.30584816049105257, 34.79301137796964127, -5.000000000000004441 ) ) ;
#12188 = CARTESIAN_POINT ( 'NONE',  ( 0.6830608540009363017, 37.47223625998419294, 10.49999999999999822 ) ) ;
#12189 = CARTESIAN_POINT ( 'NONE',  ( 10.81260707898150386, 32.90853150812155548, 7.000000000000000000 ) ) ;
#12190 = CARTESIAN_POINT ( 'NONE',  ( 0.000000000000000000, 22.50000000000000355, 7.000000000000000000 ) ) ;
#12191 = EDGE_LOOP ( 'NONE', ( #6282, #31315 ) ) ;
#12192 = CARTESIAN_POINT ( 'NONE',  ( 30.34016821446444823, 0.008728377367246306986, -8.297816611031924694 ) ) ;
#12193 = CARTESIAN_POINT ( 'NONE',  ( 12.26832665498864294, 32.91590888319125696, -4.999999999999999112 ) ) ;
#12194 = DIRECTION ( 'NONE',  ( 0.000000000000000000, 0.000000000000000000, 1.000000000000000000 ) ) ;
#12195 = AXIS2_PLACEMENT_3D ( 'NONE', #37406, #633, #10178 ) ;
#12196 = EDGE_LOOP ( 'NONE', ( #35266, #20507, #1502 ) ) ;
#12197 = CARTESIAN_POINT ( 'NONE',  ( -30.31183173745759873, 0.03880945276234878255, -8.298106778462893018 ) ) ;
#12198 = DIRECTION ( 'NONE',  ( 1.000000000000000000, 0.000000000000000000, 0.000000000000000000 ) ) ;
#12199 = ORIENTED_EDGE ( 'NONE', *, *, #33261, .F. ) ;
#12200 = CARTESIAN_POINT ( 'NONE',  ( 34.59626701887397360, -6.235679855831036456, -6.331402358434438327 ) ) ;
#12201 = CIRCLE ( 'NONE', #19972, 1.000000000000000000 ) ;
#12202 = AXIS2_PLACEMENT_3D ( 'NONE', #36434, #33199, #11057 ) ;
#12203 = ORIENTED_EDGE ( 'NONE', *, *, #13731, .T. ) ;
#12204 = CARTESIAN_POINT ( 'NONE',  ( -7.565838454495246168, 38.87983827381766844, 12.14047268033080584 ) ) ;
#12205 = AXIS2_PLACEMENT_3D ( 'NONE', #34295, #21302, #21891 ) ;
#12206 = CARTESIAN_POINT ( 'NONE',  ( 5.661571401657415237, -19.51153516500234630, 19.99202127657103389 ) ) ;
#12207 = FACE_OUTER_BOUND ( 'NONE', #1507, .T. ) ;
#12208 = CARTESIAN_POINT ( 'NONE',  ( -8.883663045967775673, 28.52602195317091827, 19.99202127657103389 ) ) ;
#12209 = CIRCLE ( 'NONE', #15457, 0.5000000000000004441 ) ;
#12210 = CARTESIAN_POINT ( 'NONE',  ( -6.440836655099179353, 34.39106106163288246, 12.00000000000000000 ) ) ;
#12211 = ORIENTED_EDGE ( 'NONE', *, *, #24147, .T. ) ;
#12212 = CARTESIAN_POINT ( 'NONE',  ( 3.699151772511975800, 7.951170058885261405, 10.49999999999999822 ) ) ;
#12213 = EDGE_CURVE ( 'NONE', #35769, #22927, #6327, .T. ) ;
#12214 = CARTESIAN_POINT ( 'NONE',  ( 10.24611365915863281, 21.92584419919065652, 10.75000000000001421 ) ) ;
#12215 = CARTESIAN_POINT ( 'NONE',  ( 4.100636323082810009, 29.29593658752792962, 6.000000000000000000 ) ) ;
#12216 = CARTESIAN_POINT ( 'NONE',  ( 12.05736835487432579, 14.38397459621550567, 9.500000000000000000 ) ) ;
#12217 = CARTESIAN_POINT ( 'NONE',  ( 7.105293529131195385, 36.67938314382616483, -6.292395027995508094 ) ) ;
#12218 = EDGE_CURVE ( 'NONE', #31473, #35530, #32953, .T. ) ;
#12219 = CARTESIAN_POINT ( 'NONE',  ( -8.137585970691990411, 29.15429895402942861, 11.00000000000000000 ) ) ;
#12220 = EDGE_CURVE ( 'NONE', #4132, #16724, #29045, .T. ) ;
#12221 = CARTESIAN_POINT ( 'NONE',  ( 16.88068922968714247, -26.18916093630494757, -9.608643031638695930 ) ) ;
#12222 = DIRECTION ( 'NONE',  ( 1.000000000000000000, 0.000000000000000000, 0.000000000000000000 ) ) ;
#12223 = DIRECTION ( 'NONE',  ( 0.000000000000000000, 0.000000000000000000, 1.000000000000000000 ) ) ;
#12224 = CARTESIAN_POINT ( 'NONE',  ( -2.229437847141422679, 24.50739181907689712, 13.00000000000000178 ) ) ;
#12225 = ORIENTED_EDGE ( 'NONE', *, *, #9771, .F. ) ;
#12227 = VECTOR ( 'NONE', #20350, 1000.000000000000000 ) ;
#12226 = CARTESIAN_POINT ( 'NONE',  ( -11.02974916714818043, 17.33288907044355298, -28.70794164723638175 ) ) ;
#12228 = CARTESIAN_POINT ( 'NONE',  ( -33.67754748216002270, -6.175997133552459495, 17.42190598798435630 ) ) ;
#12229 = CARTESIAN_POINT ( 'NONE',  ( 14.83593602140731882, -25.95848014736257880, -9.240082701127958487 ) ) ;
#12230 = CARTESIAN_POINT ( 'NONE',  ( -3.523049899833476051, 8.330220536420963384, 10.99387789255783154 ) ) ;
#12231 = VERTEX_POINT ( 'NONE', #17908 ) ;
#12232 = ORIENTED_EDGE ( 'NONE', *, *, #25773, .T. ) ;
#12233 = CARTESIAN_POINT ( 'NONE',  ( -11.04724669754545729, 20.25032463904771163, -21.46035140199475322 ) ) ;
#12234 = CARTESIAN_POINT ( 'NONE',  ( -11.59581746604265184, -16.91849113041673647, -29.30341980017526993 ) ) ;
#12235 = FACE_OUTER_BOUND ( 'NONE', #18852, .T. ) ;
#12236 = CIRCLE ( 'NONE', #33019, 1.000000000000000888 ) ;
#12237 = ORIENTED_EDGE ( 'NONE', *, *, #25247, .F. ) ;
#12238 = CARTESIAN_POINT ( 'NONE',  ( -34.01910795266670817, -9.469880945013516182, -9.355061796818153752 ) ) ;
#12239 = CARTESIAN_POINT ( 'NONE',  ( -9.320207966883044648, -18.25898334416423197, -30.00000000000000000 ) ) ;
#12240 = CARTESIAN_POINT ( 'NONE',  ( 13.86512115012093638, 28.22494587244850450, 7.203056206335839207 ) ) ;
#12241 = EDGE_LOOP ( 'NONE', ( #454, #15891, #25024, #31618 ) ) ;
#12242 = CARTESIAN_POINT ( 'NONE',  ( 25.83939409753097749, 1.310542756611064785, -15.53056140694106091 ) ) ;
#12243 = CARTESIAN_POINT ( 'NONE',  ( -3.992867117591420545, 8.524771480177605554, 11.00000000000000000 ) ) ;
#12244 = CARTESIAN_POINT ( 'NONE',  ( -6.576253646258507501, 14.29921418520934395, 11.00000000000000000 ) ) ;
#12245 = ADVANCED_FACE ( 'NONE', ( #14244 ), #12924, .T. ) ;
#12246 = ORIENTED_EDGE ( 'NONE', *, *, #33997, .F. ) ;
#12247 = CARTESIAN_POINT ( 'NONE',  ( -20.82134614922586024, 0.7609143916134510910, -26.82519756432694180 ) ) ;
#12248 = VERTEX_POINT ( 'NONE', #32746 ) ;
#12249 = CARTESIAN_POINT ( 'NONE',  ( 32.63163926239240453, -2.293081498025231202, -6.377226414710281510 ) ) ;
#12250 = FACE_OUTER_BOUND ( 'NONE', #8331, .T. ) ;
#12251 = CARTESIAN_POINT ( 'NONE',  ( 18.95259542075067927, -26.31232456688672272, 17.42190598798396550 ) ) ;
#12252 = ORIENTED_EDGE ( 'NONE', *, *, #24311, .F. ) ;
#12253 = CARTESIAN_POINT ( 'NONE',  ( -20.41719577202367475, 3.595984569019347710, -27.00753783791186535 ) ) ;
#12254 = LINE ( 'NONE', #30752, #13840 ) ;
#12255 = B_SPLINE_CURVE_WITH_KNOTS ( 'NONE', 3,
 ( #34569, #31916, #37622, #22170, #25414, #13631 ),
 .UNSPECIFIED., .F., .F.,
 ( 4, 2, 4 ),
 ( 0.000000000000000000, 0.5000000000000000000, 1.000000000000000000 ),
 .UNSPECIFIED. ) ;
#12256 = FACE_OUTER_BOUND ( 'NONE', #12185, .T. ) ;
#12257 = VECTOR ( 'NONE', #1263, 1000.000000000000114 ) ;
#12258 = CIRCLE ( 'NONE', #15511, 1.000000000000000000 ) ;
#12259 = CARTESIAN_POINT ( 'NONE',  ( -13.64211604268330724, 20.79918788657763429, 12.00000000000000000 ) ) ;
#12260 = DIRECTION ( 'NONE',  ( 0.000000000000000000, 0.000000000000000000, 1.000000000000000000 ) ) ;
#12261 = CIRCLE ( 'NONE', #31089, 0.9999999999999998890 ) ;
#12262 = B_SPLINE_SURFACE_WITH_KNOTS ( 'NONE', 3, 3, ( 
 ( #29768, #25904, #20431, #29164, #35465, #20228, #36067, #8230, #1950, #1333, #16982, #22855, #20635, #29359, #35260, #14325, #38710, #8025, #1537, #26719, #13715, #32627, #26105, #39104, #38504 ),
 ( #13514, #11289, #13922, #35863, #4781, #10679, #17189, #23062, #26316, #10888, #16576, #23271, #14123, #35668, #29564, #28956, #1744, #38910, #1135, #26522, #11087, #37059, #12075, #40100, #11485 ),
 ( #8437, #33235, #39899, #27317, #5576, #24072, #21027, #27120, #33436, #17797, #8634, #36465, #17987, #20833, #36665, #33824, #17595, #24465, #23871, #27708, #2734, #5184, #9032, #14527, #2541 ),
 ( #5381, #2143, #30772, #11879, #15125, #18183, #5973, #30171, #21418, #30377, #33035, #12276, #14930, #29964, #39706, #2932, #36273, #24271, #8835, #27515, #9228, #26919, #36863, #39306, #21222 ),
 ( #30576, #33632, #2344, #18378, #11684, #14731, #15321, #5781, #24663, #39507, #3719, #3130, #25062, #6954, #31758, #12470, #28107, #10022, #15527, #37846, #21811, #12669, #25259, #13261, #25653 ),
 ( #15718, #3525, #3328, #285, #19361, #22400, #3921, #37655, #37258, #38049, #34018, #22013, #6368, #9431, #27910, #34214, #18773, #677, #16319, #31163, #16121, #85, #37459, #18576, #21613 ),
 ( #24862, #6175, #34411, #9633, #34803, #6562, #18969, #28704, #31356, #882, #9824, #15921, #30963, #28305, #484, #12867, #22203, #34606, #6758, #19161, #31553, #28505, #13057, #25447, #26266 ),
 ( #1693, #29112, #26667, #1284, #29517, #35619, #20384, #14069, #32779, #38863, #32575, #7776, #16932, #20178, #10220, #29316, #11039, #7571, #35413, #1086, #25854, #10424, #17140, #4530, #23011 ),
 ( #38255, #7364, #38659, #4733, #26466, #32164, #10832, #23423, #35013, #22807, #35815, #16525, #22606, #35205, #19770, #7164, #7972, #4325, #19976, #13463, #16730, #4937, #13666, #17342, #26056 ),
 ( #29718, #38455, #1899, #10629, #19563, #14276, #32374, #31952, #1486, #4120, #13875, #23223, #28908, #8786, #2885, #15277, #18138, #23624, #2495, #32984, #15076, #11830, #5136, #36416, #5529 ),
 ( #39852, #8580, #2295, #36022, #21175, #33779, #39057, #11234, #39458, #23820, #26868, #17542, #39258, #11437, #30528, #5927, #14476, #33578, #29916, #14682, #8180, #20586, #33182, #20978, #20785 ),
 ( #12029, #5333, #36225, #18328, #8389, #27465, #14883, #17745, #2096, #17940, #8984, #30122, #27071, #24418, #11639, #24022, #33385, #36812, #30323, #2687, #27270, #39657, #24219, #36616, #5730 ),
 ( #21373, #30724, #37805, #19121, #9978, #16072, #9782, #12821, #34368, #25216, #27664, #6516, #28461, #25015, #12625, #18529, #3083, #27866, #34563, #21968, #240, #18728, #15673, #21764, #28061 ),
 ( #31516, #9382, #15877, #636, #12228, #15476, #3678, #33968, #3878, #37, #12423, #40048, #37616, #37213, #37410, #30920, #24816, #22161, #34168, #6713, #6319, #13018, #25407, #34764, #31117 ),
 ( #24619, #6914, #3281, #37012, #18923, #22356, #9583, #31312, #3481, #19316, #31712, #9182, #21568, #6125, #28264, #440, #13821, #22965, #31908, #29465, #35162, #13214, #17090, #13624, #19725 ),
 ( #16479, #4076, #32729, #26216, #25814, #26010, #19518, #1040, #38608, #38213, #35567, #7318, #10786, #1643, #23377, #28863, #14025, #23169, #38407, #13420, #7524, #38008, #7119, #10381, #35772 ),
 ( #35368, #22759, #32115, #4280, #834, #19928, #10181, #32532, #29270, #22559, #10583, #32323, #4486, #16683, #16889, #4686, #26418, #10990, #16275, #28661, #29065, #1243, #1438, #34968, #7729 ),
 ( #38812, #20133, #7926, #20336, #25607, #37319, #18638, #2049, #8339, #26617, #9494, #5284, #20740, #31027, #11390, #14426, #12534, #26821, #34076, #21477, #23772, #14226, #12138, #15584, #39009 ),
 ( #39211, #30635, #11185, #3195, #33133, #37122, #33883, #36172, #18439, #29864, #32931, #39961, #6236, #18242, #15384, #2793, #15184, #24926, #24525, #40162, #27970, #27575, #12334, #21870, #24722 ),
 ( #36926, #35974, #20535, #5086, #9291, #9092, #6035, #30829, #2996, #27773, #21675, #144, #4883, #17296, #29668, #17496, #1850, #23577, #8127, #25717, #38111, #4184, #22665, #16382, #19424 ),
 ( #28769, #38313, #13322, #1145, #12729, #13121, #743, #25121, #31420, #37518, #10485, #16185, #34473, #9697, #3586, #10084, #31816, #10282, #15983, #22466, #35068, #18835, #22072, #7223, #346 ),
 ( #6620, #34275, #3982, #28364, #3782, #19028, #542, #945, #12928, #19623, #25318, #32018, #16588, #13526, #37718, #28969, #25916, #31613, #9883, #25512, #15780, #22263, #34668, #6431, #3386 ),
 ( #6820, #19223, #28568, #31222, #37912, #28170, #34871, #7021, #29178, #20241, #29574, #11097, #35476, #23480, #39114, #8239, #17604, #39316, #35270, #23282, #7632, #10689, #16790, #23074, #20037 ),
 ( #32434, #13931, #26532, #14536, #26930, #36078, #4592, #26326, #4386, #22866, #35679, #38721, #20645, #29371, #16993, #29974, #1548, #11300, #38921, #10898, #32224, #1754, #33044, #1343, #7425 ),
 ( #7833, #14336, #19834, #32638, #17199, #4792, #5195, #38514, #26729, #14134, #13727, #35876, #1961, #8035, #2153, #20442, #32839, #4994, #23680, #17405, #29779, #26118, #36283, #27130, #2943 ) ),
 .UNSPECIFIED., .F., .F., .F.,
 ( 4, 3, 3, 3, 3, 3, 3, 3, 4 ),
 ( 4, 3, 3, 3, 3, 3, 3, 3, 4 ),
 ( 0.000000000000000000, 0.1250000000000000000, 0.2500000000000000000, 0.3750000000000000000, 0.5000000000000000000, 0.6250000000000000000, 0.7500000000000000000, 0.8750000000000000000, 1.000000000000000000 ),
 ( 2.365504664328351048, 2.690426355543287240, 3.015348046758223433, 3.340269737973159181, 3.665191429188095373, 3.990113120403031566, 4.315034811617967314, 4.639956502832903951, 4.964878194047839699 ),
 .UNSPECIFIED. ) ;
#12263 = ADVANCED_FACE ( 'NONE', ( #26432 ), #36194, .T. ) ;
#12264 = FACE_BOUND ( 'NONE', #37590, .T. ) ;
#12265 = CARTESIAN_POINT ( 'NONE',  ( 17.01882136417861702, 27.23043334312144736, 13.32518128616608877 ) ) ;
#12266 = ORIENTED_EDGE ( 'NONE', *, *, #37201, .F. ) ;
#12267 = CARTESIAN_POINT ( 'NONE',  ( -22.24749944600915441, 6.755814336694140110, -16.88571461955177355 ) ) ;
#12268 = CARTESIAN_POINT ( 'NONE',  ( 5.348106467989403257, 35.16482219193073178, 6.000000000000000000 ) ) ;
#12269 = EDGE_CURVE ( 'NONE', #18776, #13281, #38829, .T. ) ;
#12270 = CARTESIAN_POINT ( 'NONE',  ( -14.47283171447380390, 21.48159823030330529, 11.00000000000000000 ) ) ;
#12271 = CARTESIAN_POINT ( 'NONE',  ( 24.17850601201823935, -26.54311662592617438, -5.883534236263519901 ) ) ;
#12272 = CARTESIAN_POINT ( 'NONE',  ( -2.835137251120299684, 29.44922644035488446, 13.00000000000000178 ) ) ;
#12273 = CARTESIAN_POINT ( 'NONE',  ( 13.91919597197520808, 24.20150807187953390, -13.48820975930131461 ) ) ;
#12274 = ORIENTED_EDGE ( 'NONE', *, *, #1118, .F. ) ;
#12275 = CARTESIAN_POINT ( 'NONE',  ( -12.55985620789771318, 17.00768640634399276, -25.16950739431023365 ) ) ;
#12276 = CARTESIAN_POINT ( 'NONE',  ( -26.32839453010153719, -14.27099112026725081, 20.82122704794093693 ) ) ;
#12277 = DIRECTION ( 'NONE',  ( 0.000000000000000000, 0.000000000000000000, 1.000000000000000000 ) ) ;
#12278 = CARTESIAN_POINT ( 'NONE',  ( 14.54626310194416305, 24.93267370481178347, -11.60010698176134447 ) ) ;
#12279 = EDGE_LOOP ( 'NONE', ( #5864, #34736, #32578 ) ) ;
#12280 = CARTESIAN_POINT ( 'NONE',  ( 2.853166178176219425, 23.42705098312512746, 12.00000000000000000 ) ) ;
#12281 = ORIENTED_EDGE ( 'NONE', *, *, #437, .T. ) ;
#12283 = CARTESIAN_POINT ( 'NONE',  ( -2.853172919594720192, 21.57294901687549427, 12.00000000000000000 ) ) ;
#12282 = CARTESIAN_POINT ( 'NONE',  ( -13.38683417315264279, 23.02748639848019607, -15.42644061306512171 ) ) ;
#12284 = CARTESIAN_POINT ( 'NONE',  ( -15.64016700958762307, -26.70521847281657202, -6.413594158090527131 ) ) ;
#12285 = CARTESIAN_POINT ( 'NONE',  ( 0.5000000000000000000, 37.50000000000000711, 7.000000000000000000 ) ) ;
#12286 = AXIS2_PLACEMENT_3D ( 'NONE', #34850, #12706, #722 ) ;
#12287 = CARTESIAN_POINT ( 'NONE',  ( -19.79882239781932540, -9.636344326736496768, -24.23038216571381653 ) ) ;
#12288 = CARTESIAN_POINT ( 'NONE',  ( -9.348295649430010457, -19.45916671671450970, -23.95518150547726322 ) ) ;
#12289 = CARTESIAN_POINT ( 'NONE',  ( 12.30736835487432579, 14.81698729810772619, 7.000000000000000000 ) ) ;
#12290 = CARTESIAN_POINT ( 'NONE',  ( 16.11351922548164950, 24.44051152376729519, -5.000000000000000888 ) ) ;
#12291 = ORIENTED_EDGE ( 'NONE', *, *, #10413, .F. ) ;
#12292 = CARTESIAN_POINT ( 'NONE',  ( 26.70883441844552664, 4.675912117059606743, -5.476516349963133301 ) ) ;
#12293 = DIRECTION ( 'NONE',  ( 1.000000000000000000, 0.000000000000000000, 0.000000000000000000 ) ) ;
#12294 = EDGE_CURVE ( 'NONE', #27076, #6337, #31038, .T. ) ;
#12295 = CARTESIAN_POINT ( 'NONE',  ( 6.973232007841551727, 35.78074362234890060, 7.338691926023217071 ) ) ;
#12296 = EDGE_CURVE ( 'NONE', #2033, #19314, #23219, .T. ) ;
#12297 = CARTESIAN_POINT ( 'NONE',  ( -19.72832818285809253, -26.19953226489505127, -9.498077945716184800 ) ) ;
#12298 = AXIS2_PLACEMENT_3D ( 'NONE', #34949, #38390, #7505 ) ;
#12299 = VERTEX_POINT ( 'NONE', #37583 ) ;
#12300 = CARTESIAN_POINT ( 'NONE',  ( -20.87864677930795310, -0.1800933656229730950, -26.75177554836502125 ) ) ;
#12301 = CARTESIAN_POINT ( 'NONE',  ( 30.40872510205566925, -0.06348338061482104722, -8.294560979537857648 ) ) ;
#12302 = DIRECTION ( 'NONE',  ( 0.000000000000000000, 0.000000000000000000, 1.000000000000000000 ) ) ;
#12303 = CARTESIAN_POINT ( 'NONE',  ( 26.61692196988907355, -13.50708991729936592, 20.82122704794081258 ) ) ;
#12304 = EDGE_LOOP ( 'NONE', ( #12002, #7142 ) ) ;
#12305 = CARTESIAN_POINT ( 'NONE',  ( 13.47223693944937750, 18.09844039693851769, -30.00000000000000355 ) ) ;
#12306 = FACE_OUTER_BOUND ( 'NONE', #13674, .T. ) ;
#12307 = EDGE_LOOP ( 'NONE', ( #22061, #38989, #28944 ) ) ;
#12308 = CARTESIAN_POINT ( 'NONE',  ( 14.48927117870123027, -30.61587158504688233, 11.00000000000000000 ) ) ;
#12309 = EDGE_CURVE ( 'NONE', #10807, #31289, #5702, .T. ) ;
#12310 = VECTOR ( 'NONE', #20824, 1000.000000000000000 ) ;
#12311 = CARTESIAN_POINT ( 'NONE',  ( -8.859192577249674017, 12.20922670551869516, 23.00000000000000000 ) ) ;
#12312 = CARTESIAN_POINT ( 'NONE',  ( 37.48530129358654506, -10.40311727728359692, -5.000000000000010658 ) ) ;
#12313 = CARTESIAN_POINT ( 'NONE',  ( 2.706689172267205290, 26.59357338535925308, -18.64150033707969811 ) ) ;
#12314 = CYLINDRICAL_SURFACE ( 'NONE', #13323, 17.00000000000000000 ) ;
#12315 = PLANE ( 'NONE',  #5235 ) ;
#12316 = DIRECTION ( 'NONE',  ( -0.000000000000000000, -0.000000000000000000, -1.000000000000000000 ) ) ;
#12317 = AXIS2_PLACEMENT_3D ( 'NONE', #971, #19862, #25342 ) ;
#12319 = EDGE_CURVE ( 'NONE', #12345, #13029, #3749, .T. ) ;
#12318 = CARTESIAN_POINT ( 'NONE',  ( 6.312035131040564906, 19.41226734497195849, 6.000000000000000000 ) ) ;
#12320 = CARTESIAN_POINT ( 'NONE',  ( 11.73118655278371492, 31.84795188348743622, 7.381627713044569106 ) ) ;
#12321 = CARTESIAN_POINT ( 'NONE',  ( 13.66396806110179973, 24.77360163986799435, -13.43593853470100186 ) ) ;
#12322 = DIRECTION ( 'NONE',  ( 1.000000000000000000, 0.000000000000000000, 0.000000000000000000 ) ) ;
#12323 = VERTEX_POINT ( 'NONE', #30495 ) ;
#12325 = DIRECTION ( 'NONE',  ( 0.000000000000000000, -0.5821182788257888152, 0.8131041196900314905 ) ) ;
#12324 = CARTESIAN_POINT ( 'NONE',  ( -15.42551642139064327, 13.50153766309080616, -30.00000000000001421 ) ) ;
#12326 = CARTESIAN_POINT ( 'NONE',  ( 7.309360666678370144, 9.887575703124513282, 7.000000000000000000 ) ) ;
#12327 = CARTESIAN_POINT ( 'NONE',  ( 11.18307060885532600, -20.46872301250157022, -20.54176180563865373 ) ) ;
#12328 = CARTESIAN_POINT ( 'NONE',  ( -21.68568904104562023, -27.13690135270087822, -5.452393508887768192 ) ) ;
#12329 = CARTESIAN_POINT ( 'NONE',  ( 15.33694215129139948, 26.62211003415151467, -6.887897498730077395 ) ) ;
#12330 = CARTESIAN_POINT ( 'NONE',  ( 15.09448029680397241, 26.16123611564987428, -8.766612590816048822 ) ) ;
#12331 = ORIENTED_EDGE ( 'NONE', *, *, #22945, .F. ) ;
#12332 = CARTESIAN_POINT ( 'NONE',  ( 2.853166178176219425, 23.42705098312512746, 6.000000000000000000 ) ) ;
#12333 = CARTESIAN_POINT ( 'NONE',  ( -9.432189322962019062, -18.20121415529274600, -29.34969478843057544 ) ) ;
#12334 = CARTESIAN_POINT ( 'NONE',  ( -18.87560410041185222, -28.49365963342004804, 14.53008259254054124 ) ) ;
#12335 = CARTESIAN_POINT ( 'NONE',  ( -15.95852086734116071, -13.25472829660814789, -27.74404909499182637 ) ) ;
#12336 = CARTESIAN_POINT ( 'NONE',  ( 1.306219793455511313, -21.01157610766281891, -24.41760533827341817 ) ) ;
#12337 = CARTESIAN_POINT ( 'NONE',  ( 15.39253874130542776, 25.56879223000222723, -8.303194391403303953 ) ) ;
#12338 = CARTESIAN_POINT ( 'NONE',  ( 21.87469278667276384, 10.95211447422776985, -9.392538902003625623 ) ) ;
#12339 = CARTESIAN_POINT ( 'NONE',  ( 13.48130249190479191, 27.93180293473185927, 7.500000000000000888 ) ) ;
#12340 = CARTESIAN_POINT ( 'NONE',  ( -3.458130042104726076, 20.20612265101129168, -29.99999999999998579 ) ) ;
#12341 = VERTEX_POINT ( 'NONE', #9752 ) ;
#12342 = CARTESIAN_POINT ( 'NONE',  ( -34.46511719672074747, -5.518907050001597092, -5.451568486426576321 ) ) ;
#12343 = EDGE_CURVE ( 'NONE', #17337, #26123, #1830, .T. ) ;
#12344 = CARTESIAN_POINT ( 'NONE',  ( -25.71480618105494642, 9.014447550991281588, 11.00000000000190603 ) ) ;
#12345 = VERTEX_POINT ( 'NONE', #24985 ) ;
#12346 = CARTESIAN_POINT ( 'NONE',  ( -9.997483185316564658, 21.95197631500770541, 10.00000000000000000 ) ) ;
#12347 = CARTESIAN_POINT ( 'NONE',  ( 5.064564986133971658, 13.54338174056915456, 12.00000000000000000 ) ) ;
#12348 = CIRCLE ( 'NONE', #9772, 0.5000000000000004441 ) ;
#12349 = CARTESIAN_POINT ( 'NONE',  ( -20.93293132456442152, 1.148100751203120939, -26.25406389234631988 ) ) ;
#12350 = CARTESIAN_POINT ( 'NONE',  ( 33.48600411488287421, -13.44844601827948694, -9.747306394059473078 ) ) ;
#12351 = EDGE_LOOP ( 'NONE', ( #24394, #13812, #15354, #23006, #34029, #11796 ) ) ;
#12352 = DIRECTION ( 'NONE',  ( 0.000000000000000000, 0.000000000000000000, 1.000000000000000000 ) ) ;
#12353 = ORIENTED_EDGE ( 'NONE', *, *, #11141, .T. ) ;
#12354 = DIRECTION ( 'NONE',  ( -1.000000000000000000, -1.224646799147353947E-16, 0.000000000000000000 ) ) ;
#12355 = CARTESIAN_POINT ( 'NONE',  ( 0.000000000000000000, 22.50000000000000355, 7.000000000000000000 ) ) ;
#12356 = EDGE_CURVE ( 'NONE', #18033, #8130, #2855, .T. ) ;
#12357 = AXIS2_PLACEMENT_3D ( 'NONE', #15408, #1572, #20062 ) ;
#12358 = DIRECTION ( 'NONE',  ( -1.000000000000000000, 0.000000000000000000, 0.000000000000000000 ) ) ;
#12359 = EDGE_LOOP ( 'NONE', ( #33653, #27825, #13788 ) ) ;
#12360 = EDGE_CURVE ( 'NONE', #11661, #33995, #3254, .T. ) ;
#12361 = CARTESIAN_POINT ( 'NONE',  ( -2.233363292134739275, 27.76951152815063395, -17.61292157057414443 ) ) ;
#12362 = AXIS2_PLACEMENT_3D ( 'NONE', #22493, #32256, #7252 ) ;
#12363 = LINE ( 'NONE', #9120, #4223 ) ;
#12364 = CARTESIAN_POINT ( 'NONE',  ( 3.610593701936716027, 31.83882289796390097, 10.00000000000000000 ) ) ;
#12365 = CARTESIAN_POINT ( 'NONE',  ( 3.295881626406578224, 9.398963235502483471, 9.500000000000000000 ) ) ;
#12366 = CARTESIAN_POINT ( 'NONE',  ( 18.06868231757531618, -13.86363220686757458, -23.03522161772968957 ) ) ;
#12367 = CARTESIAN_POINT ( 'NONE',  ( 19.62469028259190651, 14.57143679938034353, -10.37640014583656978 ) ) ;
#12368 = CARTESIAN_POINT ( 'NONE',  ( 8.965364566908062827, 21.09711902998411404, -22.32596467695269382 ) ) ;
#12369 = EDGE_LOOP ( 'NONE', ( #37726, #4002 ) ) ;
#12370 = ADVANCED_FACE ( 'NONE', ( #34337 ), #12393, .F. ) ;
#12371 = CARTESIAN_POINT ( 'NONE',  ( -20.70514017605514923, 13.67614408150934580, -5.967130309997563664 ) ) ;
#12372 = CARTESIAN_POINT ( 'NONE',  ( -4.672335726382881305, 24.36080358023109227, 23.00000000000000000 ) ) ;
#12373 = CARTESIAN_POINT ( 'NONE',  ( 13.83086666455825053, -24.13364333532040007, -13.50291250830041889 ) ) ;
#12374 = CARTESIAN_POINT ( 'NONE',  ( -13.47830981910552772, 21.58612669357095015, 10.50000000000000000 ) ) ;
#12375 = AXIS2_PLACEMENT_3D ( 'NONE', #11574, #39596, #23962 ) ;
#12376 = CARTESIAN_POINT ( 'NONE',  ( -8.937590682902627037, -20.71651963383551731, -21.24786896499727007 ) ) ;
#12377 = CARTESIAN_POINT ( 'NONE',  ( -8.401171878996500197, 21.11424711454089476, 7.000000000000000000 ) ) ;
#12378 = CARTESIAN_POINT ( 'NONE',  ( -12.37187468849621474, 20.51614643895100087, -19.49228216629809651 ) ) ;
#12379 = CARTESIAN_POINT ( 'NONE',  ( -24.87088375429694054, -26.22384022550785687, -6.313645004022516716 ) ) ;
#12380 = CARTESIAN_POINT ( 'NONE',  ( 8.607094368180748134, -18.65170925544331126, -28.74046143688874366 ) ) ;
#12381 = FACE_OUTER_BOUND ( 'NONE', #4446, .T. ) ;
#12382 = ORIENTED_EDGE ( 'NONE', *, *, #1071, .F. ) ;
#12383 = CARTESIAN_POINT ( 'NONE',  ( -11.00990894457517477, 33.49669252407993270, -7.634107675710282592 ) ) ;
#12384 = EDGE_CURVE ( 'NONE', #39240, #18776, #6488, .T. ) ;
#12385 = CARTESIAN_POINT ( 'NONE',  ( 0.5000000000000000000, 37.23829181893393070, 10.94387467462633623 ) ) ;
#12386 = DIRECTION ( 'NONE',  ( -0.3090169943749414005, 0.9510565162951555296, 0.000000000000000000 ) ) ;
#12387 = ADVANCED_FACE ( 'NONE', ( #18893 ), #2656, .F. ) ;
#12388 = AXIS2_PLACEMENT_3D ( 'NONE', #16263, #6308, #19302 ) ;
#12389 = CARTESIAN_POINT ( 'NONE',  ( 12.99377146717205989, 26.19620116591418935, 9.500000000000000000 ) ) ;
#12390 = ORIENTED_EDGE ( 'NONE', *, *, #20360, .T. ) ;
#12391 = CARTESIAN_POINT ( 'NONE',  ( 27.71930269395751623, 0.2145384403578754484, -13.51489228889109029 ) ) ;
#12392 = FACE_OUTER_BOUND ( 'NONE', #7483, .T. ) ;
#12393 = PLANE ( 'NONE',  #16726 ) ;
#12394 = ORIENTED_EDGE ( 'NONE', *, *, #21707, .T. ) ;
#12395 = CARTESIAN_POINT ( 'NONE',  ( -30.57930627834187831, 0.02004245076167957690, -7.358024370966995242 ) ) ;
#12396 = CARTESIAN_POINT ( 'NONE',  ( -14.09933648065464062, 26.02968990214173317, 9.500000000000000000 ) ) ;
#12397 = ORIENTED_EDGE ( 'NONE', *, *, #32488, .F. ) ;
#12398 = CARTESIAN_POINT ( 'NONE',  ( 34.34316617829726681, -7.172350984383295547, -8.073188482078531791 ) ) ;
#12399 = ORIENTED_EDGE ( 'NONE', *, *, #21193, .T. ) ;
#12400 = CARTESIAN_POINT ( 'NONE',  ( 12.30427675147600297, 35.50736440027970531, 12.73282698324849171 ) ) ;
#12401 = AXIS2_PLACEMENT_3D ( 'NONE', #7056, #13153, #17025 ) ;
#12402 = CARTESIAN_POINT ( 'NONE',  ( -18.23649648353769948, -16.09146789626166196, 20.99999999999999645 ) ) ;
#12403 = DIRECTION ( 'NONE',  ( 1.000000000000000000, 0.000000000000000000, 0.000000000000000000 ) ) ;
#12404 = EDGE_CURVE ( 'NONE', #27087, #21540, #26462, .T. ) ;
#12405 = CARTESIAN_POINT ( 'NONE',  ( -8.810143528080892850, 27.17887818198020611, 20.25080042701568317 ) ) ;
#12406 = DIRECTION ( 'NONE',  ( 1.000000000000000000, 0.000000000000000000, -0.000000000000000000 ) ) ;
#12407 = ORIENTED_EDGE ( 'NONE', *, *, #25769, .F. ) ;
#12408 = EDGE_CURVE ( 'NONE', #33298, #12173, #12830, .T. ) ;
#12409 = CARTESIAN_POINT ( 'NONE',  ( 3.513409677696501365, 8.375574215747722207, 11.00000000000000355 ) ) ;
#12410 = CARTESIAN_POINT ( 'NONE',  ( -17.34253826607193361, 27.32041144404004740, 11.55979286843935050 ) ) ;
#12411 = FACE_OUTER_BOUND ( 'NONE', #26031, .T. ) ;
#12412 = DIRECTION ( 'NONE',  ( 1.000000000000000000, 0.000000000000000000, 0.000000000000000000 ) ) ;
#12413 = CARTESIAN_POINT ( 'NONE',  ( 5.157905742752888045, 22.93259919978908457, -21.98816088478811182 ) ) ;
#12414 = AXIS2_PLACEMENT_3D ( 'NONE', #30262, #36956, #9121 ) ;
#12415 = LINE ( 'NONE', #15465, #13999 ) ;
#12416 = CIRCLE ( 'NONE', #39590, 1.000000000000000000 ) ;
#12417 = CARTESIAN_POINT ( 'NONE',  ( 15.60024655210046163, -23.09233175402551197, -15.20950988053776420 ) ) ;
#12418 = DIRECTION ( 'NONE',  ( 0.000000000000000000, 0.000000000000000000, 1.000000000000000000 ) ) ;
#12419 = CARTESIAN_POINT ( 'NONE',  ( 11.14716901145161643, 12.46304090461738667, 13.00000000000000178 ) ) ;
#12420 = CARTESIAN_POINT ( 'NONE',  ( 1.281526940109136037, 37.44563527730423402, 7.102474990965860435 ) ) ;
#12421 = ORIENTED_EDGE ( 'NONE', *, *, #35953, .T. ) ;
#12422 = CARTESIAN_POINT ( 'NONE',  ( -15.35173535111459131, 26.57026200220170509, -6.888001712493197815 ) ) ;
#12423 = CARTESIAN_POINT ( 'NONE',  ( -33.85500357264719185, -15.79720895789074575, 17.42190598798393708 ) ) ;
#12424 = CARTESIAN_POINT ( 'NONE',  ( 15.17959409457666098, -26.46972997935209904, -7.358350661662780290 ) ) ;
#12425 = AXIS2_PLACEMENT_3D ( 'NONE', #21530, #24384, #33545 ) ;
#12426 = LINE ( 'NONE', #24818, #34758 ) ;
#12427 = VERTEX_POINT ( 'NONE', #27434 ) ;
#12428 = ORIENTED_EDGE ( 'NONE', *, *, #36274, .F. ) ;
#12429 = CARTESIAN_POINT ( 'NONE',  ( -13.93864121817066248, 26.51574797513629989, -11.48636496174305499 ) ) ;
#12430 = CARTESIAN_POINT ( 'NONE',  ( -13.98800961053418490, -21.23703842434798972, -18.20997924916034805 ) ) ;
#12431 = FACE_BOUND ( 'NONE', #8073, .T. ) ;
#12432 = VERTEX_POINT ( 'NONE', #37181 ) ;
#12433 = CARTESIAN_POINT ( 'NONE',  ( -29.12014979997558228, -9.039752278382179540, -14.83108018992303023 ) ) ;
#12434 = CARTESIAN_POINT ( 'NONE',  ( -9.523195312559730397, -18.67992273108535528, -26.24930059924759718 ) ) ;
#12435 = CARTESIAN_POINT ( 'NONE',  ( 0.5000000000000000000, 37.50000000000000711, 10.49999999999999822 ) ) ;
#12436 = ORIENTED_EDGE ( 'NONE', *, *, #23555, .T. ) ;
#12437 = CARTESIAN_POINT ( 'NONE',  ( 22.66673786582151706, 0.8234316233675766927, -21.64362386725597176 ) ) ;
#12438 = DIRECTION ( 'NONE',  ( 1.000000000000000000, 0.000000000000000000, 0.000000000000000000 ) ) ;
#12439 = CARTESIAN_POINT ( 'NONE',  ( -9.927394655428436465, 11.06314620770957013, 7.000000000000000000 ) ) ;
#12440 = EDGE_CURVE ( 'NONE', #40188, #14680, #24388, .T. ) ;
#12441 = ORIENTED_EDGE ( 'NONE', *, *, #26045, .T. ) ;
#12442 = CARTESIAN_POINT ( 'NONE',  ( -23.32581642294337598, 0.5282185752115819977, -20.53879718575241142 ) ) ;
#12443 = ORIENTED_EDGE ( 'NONE', *, *, #37203, .F. ) ;
#12444 = CARTESIAN_POINT ( 'NONE',  ( 23.80926127916344726, -0.9845178533687296563, -20.33980794348563492 ) ) ;
#12445 = B_SPLINE_CURVE_WITH_KNOTS ( 'NONE', 3,
 ( #27953, #18422, #40143, #12320, #127, #24706, #37106, #18623 ),
 .UNSPECIFIED., .F., .F.,
 ( 4, 2, 2, 4 ),
 ( 0.000000000000000000, 0.0002364868538934288911, 0.0004729737077868577822, 0.0009459474155737128539 ),
 .UNSPECIFIED. ) ;
#12446 = CIRCLE ( 'NONE', #39037, 0.4999999999999998335 ) ;
#12447 =( REPRESENTATION_RELATIONSHIP ('NONE','NONE', #15382, #33787 ) REPRESENTATION_RELATIONSHIP_WITH_TRANSFORMATION ( #35947 )SHAPE_REPRESENTATION_RELATIONSHIP( ) );
#12448 = CARTESIAN_POINT ( 'NONE',  ( 23.05386822411318803, -7.747535282638377652, 20.99999999999999645 ) ) ;
#12449 = CARTESIAN_POINT ( 'NONE',  ( 15.89892447185075497, -25.15199583021637508, 17.92354375535250810 ) ) ;
#12450 = ORIENTED_EDGE ( 'NONE', *, *, #35490, .F. ) ;
#12451 = CARTESIAN_POINT ( 'NONE',  ( -26.19606766578834467, 4.393075645995596190, -9.799521558767215978 ) ) ;
#12452 = PLANE ( 'NONE',  #36915 ) ;
#12453 = FACE_OUTER_BOUND ( 'NONE', #38291, .T. ) ;
#12454 = CARTESIAN_POINT ( 'NONE',  ( -18.87179230188976220, -27.32956261471019133, -4.999999999999999112 ) ) ;
#12455 = CIRCLE ( 'NONE', #19591, 1.000000000000000888 ) ;
#12456 = DIRECTION ( 'NONE',  ( 1.000000000000000000, 0.000000000000000000, 0.000000000000000000 ) ) ;
#12457 = AXIS2_PLACEMENT_3D ( 'NONE', #16746, #6773, #22621 ) ;
#12458 = FACE_BOUND ( 'NONE', #5993, .T. ) ;
#12459 = CARTESIAN_POINT ( 'NONE',  ( 18.37899676820244110, 22.33688965558069128, 13.32518128614809605 ) ) ;
#12460 = CARTESIAN_POINT ( 'NONE',  ( -19.88990440888141009, 6.451044192260599885, -25.43228481840965216 ) ) ;
#12461 = DIRECTION ( 'NONE',  ( 1.000000000000000000, 0.000000000000000000, 0.000000000000000000 ) ) ;
#12462 = EDGE_CURVE ( 'NONE', #9140, #26271, #15243, .T. ) ;
#12463 = CARTESIAN_POINT ( 'NONE',  ( -0.4999999999999998890, 37.00000000000000711, 7.000000000000000000 ) ) ;
#12464 = CARTESIAN_POINT ( 'NONE',  ( 16.74526845675677578, -17.41194385859613902, -20.93759567407294853 ) ) ;
#12465 = LINE ( 'NONE', #15120, #13186 ) ;
#12466 = CARTESIAN_POINT ( 'NONE',  ( 14.85865438977763375, 26.03933603557532095, -9.695787514185630229 ) ) ;
#12467 = ORIENTED_EDGE ( 'NONE', *, *, #22968, .T. ) ;
#12468 = CARTESIAN_POINT ( 'NONE',  ( -13.10226789136070380, 16.53484623785779561, -25.23106048629698961 ) ) ;
#12469 = AXIS2_PLACEMENT_3D ( 'NONE', #7358, #876, #38045 ) ;
#12470 = CARTESIAN_POINT ( 'NONE',  ( -24.94906875546841363, -17.45075080782938315, 20.69868183039781329 ) ) ;
#12471 = DIRECTION ( 'NONE',  ( 0.000000000000000000, 0.000000000000000000, 1.000000000000000000 ) ) ;
#12472 = CARTESIAN_POINT ( 'NONE',  ( 14.86387305504814726, 25.53751346079465989, -10.18168596463881137 ) ) ;
#12473 = EDGE_LOOP ( 'NONE', ( #2453, #12108, #30792, #26198 ) ) ;
#12474 = CARTESIAN_POINT ( 'NONE',  ( 0.3582258883630317636, 11.68927977431952137, 12.00000000000000000 ) ) ;
#12475 = VERTEX_POINT ( 'NONE', #21345 ) ;
#12477 = DIRECTION ( 'NONE',  ( -0.000000000000000000, -0.000000000000000000, -1.000000000000000000 ) ) ;
#12476 = CARTESIAN_POINT ( 'NONE',  ( -12.53799127256666956, 21.22453523357990335, -18.42692599694124667 ) ) ;
#12478 = CARTESIAN_POINT ( 'NONE',  ( -13.56363600825507199, -23.64209565141708325, -14.45832144993096691 ) ) ;
#12479 = CARTESIAN_POINT ( 'NONE',  ( 5.237540274239914417, 35.49300472853430222, 7.500000000000000000 ) ) ;
#12480 = EDGE_LOOP ( 'NONE', ( #25001, #6270 ) ) ;
#12481 = CARTESIAN_POINT ( 'NONE',  ( -34.55317057183779639, -15.49588746005725959, -7.124090691308525791 ) ) ;
#12482 = CARTESIAN_POINT ( 'NONE',  ( -11.15263382927128966, -25.10807195756887467, -9.767712422240766301 ) ) ;
#12483 = DIRECTION ( 'NONE',  ( -0.000000000000000000, -0.000000000000000000, -1.000000000000000000 ) ) ;
#12484 = CARTESIAN_POINT ( 'NONE',  ( 14.12418929389014011, 20.63997023270749054, -16.57871110594469855 ) ) ;
#12485 = ORIENTED_EDGE ( 'NONE', *, *, #11811, .F. ) ;
#12486 = CARTESIAN_POINT ( 'NONE',  ( 25.71414162338313858, 4.640216332958793544, -10.78049592915970400 ) ) ;
#12487 = ADVANCED_FACE ( 'NONE', ( #6093 ), #37489, .T. ) ;
#12488 = DIRECTION ( 'NONE',  ( 0.5877852522924691403, -0.8090169943749503378, -1.734723475976808672E-15 ) ) ;
#12489 = CYLINDRICAL_SURFACE ( 'NONE', #18647, 0.5000000000000004441 ) ;
#12490 = DIRECTION ( 'NONE',  ( -0.000000000000000000, -0.000000000000000000, -1.000000000000000000 ) ) ;
#12491 = VERTEX_POINT ( 'NONE', #12595 ) ;
#12492 = CARTESIAN_POINT ( 'NONE',  ( -25.40327909237853632, 0.02527255523525553590, -17.39221788563712678 ) ) ;
#12493 = EDGE_CURVE ( 'NONE', #7370, #31948, #24526, .T. ) ;
#12494 = CARTESIAN_POINT ( 'NONE',  ( 25.38697857826957005, 0.05609946110438526062, -17.39619723301043663 ) ) ;
#12495 = AXIS2_PLACEMENT_3D ( 'NONE', #16946, #500, #19784 ) ;
#12496 = CARTESIAN_POINT ( 'NONE',  ( -5.578816091646024766, 36.25952276447313949, 10.87262190629284930 ) ) ;
#12497 = ADVANCED_FACE ( 'NONE', ( #36984 ), #9150, .F. ) ;
#12498 = CARTESIAN_POINT ( 'NONE',  ( 27.58732789242641203, -12.88115193908554978, 20.69868183039782394 ) ) ;
#12499 = EDGE_LOOP ( 'NONE', ( #30321, #26637, #13819, #18495 ) ) ;
#12500 = EDGE_CURVE ( 'NONE', #24748, #28626, #19091, .T. ) ;
#12501 = CARTESIAN_POINT ( 'NONE',  ( 19.79815887584821610, 19.84782313723624370, -5.000000000000007994 ) ) ;
#12502 = FACE_OUTER_BOUND ( 'NONE', #33390, .T. ) ;
#12503 = VERTEX_POINT ( 'NONE', #16858 ) ;
#12504 = LINE ( 'NONE', #19196, #35962 ) ;
#12505 = B_SPLINE_CURVE_WITH_KNOTS ( 'NONE', 3,
 ( #5746, #3293, #12240, #21775, #37024, #2701, #2510, #24432 ),
 .UNSPECIFIED., .F., .F.,
 ( 4, 2, 2, 4 ),
 ( 0.000000000000000000, 0.0004726692273637226271, 0.0007090038410455847808, 0.0009453384547274468804 ),
 .UNSPECIFIED. ) ;
#12506 = AXIS2_PLACEMENT_3D ( 'NONE', #14720, #23461, #33223 ) ;
#12507 = LINE ( 'NONE', #40136, #30513 ) ;
#12508 = CARTESIAN_POINT ( 'NONE',  ( 37.48538792151179422, -11.24999995791135809, -5.000000000000002665 ) ) ;
#12509 = CARTESIAN_POINT ( 'NONE',  ( 2.647469807785585605, 36.69595272411527986, -9.286360570462178998 ) ) ;
#12510 = DIRECTION ( 'NONE',  ( 0.000000000000000000, 0.000000000000000000, 1.000000000000000000 ) ) ;
#12511 = EDGE_CURVE ( 'NONE', #32321, #22892, #25688, .T. ) ;
#12512 = CARTESIAN_POINT ( 'NONE',  ( 14.50704651774852927, 20.00412295564763099, 10.49999999999999822 ) ) ;
#12513 = CIRCLE ( 'NONE', #10576, 0.5000000000000004441 ) ;
#12514 = EDGE_CURVE ( 'NONE', #26968, #33412, #12201, .T. ) ;
#12515 = FACE_OUTER_BOUND ( 'NONE', #19125, .T. ) ;
#12516 = CARTESIAN_POINT ( 'NONE',  ( 2.672146553953306025, 12.33340603770390764, 10.00000000000000000 ) ) ;
#12517 = CARTESIAN_POINT ( 'NONE',  ( -14.36830325120615903, 20.48707633493503621, 7.000000000000000000 ) ) ;
#12518 = CARTESIAN_POINT ( 'NONE',  ( -14.36830325120615548, 20.48707633493503621, 7.000000000000000000 ) ) ;
#12519 = CARTESIAN_POINT ( 'NONE',  ( 14.40253865757656904, 26.32860937628373676, -10.59413652422460217 ) ) ;
#12520 = CARTESIAN_POINT ( 'NONE',  ( -8.927394655428429360, 11.06314620770957013, 11.00000000000000000 ) ) ;
#12521 = VERTEX_POINT ( 'NONE', #10348 ) ;
#12522 = AXIS2_PLACEMENT_3D ( 'NONE', #9397, #30735, #15685 ) ;
#12524 = LINE ( 'NONE', #31211, #1242 ) ;
#12523 = CARTESIAN_POINT ( 'NONE',  ( -18.56076843189209313, 17.44795389765408444, -8.382486478387699336 ) ) ;
#12525 = FACE_OUTER_BOUND ( 'NONE', #19492, .T. ) ;
#12526 = CARTESIAN_POINT ( 'NONE',  ( 9.796177435753577356, -18.55921797199988532, -26.22383286036198768 ) ) ;
#12527 = CARTESIAN_POINT ( 'NONE',  ( -22.70315127378580300, -26.84338220279167331, -6.331427942688537591 ) ) ;
#12528 = CARTESIAN_POINT ( 'NONE',  ( 10.99090272494190046, 17.30462611091308034, -30.00000000000000711 ) ) ;
#12529 = CARTESIAN_POINT ( 'NONE',  ( 15.36357391709072040, 26.70243454889372003, -6.416728717100916413 ) ) ;
#12530 = ORIENTED_EDGE ( 'NONE', *, *, #16852, .T. ) ;
#12531 = CARTESIAN_POINT ( 'NONE',  ( -23.05386822411323422, -7.747535282638357224, 23.00000000000000000 ) ) ;
#12532 = CARTESIAN_POINT ( 'NONE',  ( -15.23883232513551533, -26.48425076293248281, -7.358141420259828536 ) ) ;
#12533 = AXIS2_PLACEMENT_3D ( 'NONE', #20020, #3964, #37699 ) ;
#12534 = CARTESIAN_POINT ( 'NONE',  ( -29.26100170765952058, -25.10377279865925004, 15.13084544680221377 ) ) ;
#12535 = CARTESIAN_POINT ( 'NONE',  ( -27.45201627647075426, -18.96585292318375693, -12.89829047187982525 ) ) ;
#12536 = CARTESIAN_POINT ( 'NONE',  ( -0.3875490619503205725, -24.70434061326229269, -6.939883883725533664 ) ) ;
#12537 = CARTESIAN_POINT ( 'NONE',  ( 11.46070356447341076, 17.55389630813125024, -26.25396252495082905 ) ) ;
#12538 = CARTESIAN_POINT ( 'NONE',  ( 21.01290135064779463, 10.57244385225932781, -13.90025499387392216 ) ) ;
#12539 = FACE_OUTER_BOUND ( 'NONE', #5328, .T. ) ;
#12540 = CIRCLE ( 'NONE', #35241, 1.000000000000000888 ) ;
#12541 = ORIENTED_EDGE ( 'NONE', *, *, #7809, .F. ) ;
#12542 = CARTESIAN_POINT ( 'NONE',  ( -20.35866630304074221, -2.409458700188494618, -29.28927096481215031 ) ) ;
#12543 = EDGE_CURVE ( 'NONE', #31959, #30328, #25577, .T. ) ;
#12544 = VECTOR ( 'NONE', #35559, 1000.000000000000000 ) ;
#12545 = CARTESIAN_POINT ( 'NONE',  ( -12.55429062395547035, 25.98950339718248870, 18.87996532025784902 ) ) ;
#12546 = EDGE_LOOP ( 'NONE', ( #31894, #32692 ) ) ;
#12547 = DIRECTION ( 'NONE',  ( 0.4067366430757888840, -0.9135454576426058626, -0.000000000000000000 ) ) ;
#12548 = DIRECTION ( 'NONE',  ( 0.000000000000000000, 0.000000000000000000, 1.000000000000000000 ) ) ;
#12549 = CARTESIAN_POINT ( 'NONE',  ( -21.20053173203535835, 1.290506853206223381, -25.06817133786373475 ) ) ;
#12550 = CARTESIAN_POINT ( 'NONE',  ( 19.65282344174659457, -6.596692726057402645, -27.76040915297549461 ) ) ;
#12551 = CARTESIAN_POINT ( 'NONE',  ( 36.01432606574135065, -5.340291233615181987, 13.92931973827784908 ) ) ;
#12552 = CONICAL_SURFACE ( 'NONE', #8644, 1.000000000000004441, 0.7853981633974524978 ) ;
#12553 = ORIENTED_EDGE ( 'NONE', *, *, #29898, .F. ) ;
#12554 = FACE_OUTER_BOUND ( 'NONE', #27485, .T. ) ;
#12555 = ORIENTED_EDGE ( 'NONE', *, *, #2053, .T. ) ;
#12556 = PLANE ( 'NONE',  #26850 ) ;
#12557 = CARTESIAN_POINT ( 'NONE',  ( 15.21690391738993320, 27.44427296666788862, 13.00000000000000178 ) ) ;
#12558 = DIRECTION ( 'NONE',  ( -0.000000000000000000, -0.000000000000000000, -1.000000000000000000 ) ) ;
#12559 = ORIENTED_EDGE ( 'NONE', *, *, #6603, .T. ) ;
#12560 = CIRCLE ( 'NONE', #5436, 15.00000000000000000 ) ;
#12561 = CARTESIAN_POINT ( 'NONE',  ( -3.812539336066663065, 34.03298746155307697, -11.98968657202452448 ) ) ;
#12562 = CYLINDRICAL_SURFACE ( 'NONE', #31456, 18.00000000000003553 ) ;
#12563 = CARTESIAN_POINT ( 'NONE',  ( -7.935100905948476502, 11.57827057593827469, 7.000000000000000000 ) ) ;
#12564 = EDGE_CURVE ( 'NONE', #22450, #37934, #28402, .T. ) ;
#12565 = DIRECTION ( 'NONE',  ( 0.4999999999999919509, -0.8660254037844432595, 0.000000000000000000 ) ) ;
#12566 = DIRECTION ( 'NONE',  ( 0.000000000000000000, 0.000000000000000000, -1.000000000000000000 ) ) ;
#12567 = AXIS2_PLACEMENT_3D ( 'NONE', #10722, #32469, #13967 ) ;
#12568 = CARTESIAN_POINT ( 'NONE',  ( 8.747848026427400114, 18.74166680801365104, -27.94534499906865221 ) ) ;
#12569 = EDGE_LOOP ( 'NONE', ( #21951, #27029, #12672, #17270 ) ) ;
#12570 = CARTESIAN_POINT ( 'NONE',  ( -20.71763460597477291, 13.68537009249746461, -4.999999999999996447 ) ) ;
#12571 = CARTESIAN_POINT ( 'NONE',  ( 17.76739295965371923, 31.93461338995193799, 23.00000000000000711 ) ) ;
#12572 = CARTESIAN_POINT ( 'NONE',  ( 15.55607442552794950, -26.68487202370114630, -6.414919209907756326 ) ) ;
#12573 = CARTESIAN_POINT ( 'NONE',  ( 37.48557158514984167, -11.25000000000009237, 3.000000000000000000 ) ) ;
#12574 = CARTESIAN_POINT ( 'NONE',  ( 10.93327523444657778, 17.34109439532409525, -29.99999999999999289 ) ) ;
#12575 = CARTESIAN_POINT ( 'NONE',  ( 21.88499642459564143, -5.528038495964486820, -29.99999999999998224 ) ) ;
#12576 = CARTESIAN_POINT ( 'NONE',  ( 11.19134295108988830, 14.88397459621551100, 10.00000000000000000 ) ) ;
#12577 = CARTESIAN_POINT ( 'NONE',  ( -11.15585325849543707, 17.77692559745511858, -26.22179184702690691 ) ) ;
#12578 = AXIS2_PLACEMENT_3D ( 'NONE', #25339, #28390, #21699 ) ;
#12579 = CARTESIAN_POINT ( 'NONE',  ( -25.75211752115588126, -25.63936478115028450, -7.167472985298198651 ) ) ;
#12580 = CARTESIAN_POINT ( 'NONE',  ( 8.739015621761494046, -22.16521160953498182, -17.72474713041751215 ) ) ;
#12581 = CARTESIAN_POINT ( 'NONE',  ( 11.07558645076263737, 17.30325621831820371, -28.70984248050030985 ) ) ;
#12582 = CARTESIAN_POINT ( 'NONE',  ( 22.56924115802582875, -16.29358669976124219, -17.62083569142466288 ) ) ;
#12583 = CARTESIAN_POINT ( 'NONE',  ( -3.118678732975735279, 7.827785988993307242, 13.00000000000000178 ) ) ;
#12584 = ORIENTED_EDGE ( 'NONE', *, *, #39945, .T. ) ;
#12585 = CARTESIAN_POINT ( 'NONE',  ( -7.826018490237524716, 23.62355187122631506, -19.93686502536784033 ) ) ;
#12586 = CARTESIAN_POINT ( 'NONE',  ( 0.5000000000000000000, 37.50000000000000711, 10.49999999999999822 ) ) ;
#12587 = EDGE_CURVE ( 'NONE', #38149, #27435, #29714, .T. ) ;
#12588 = CARTESIAN_POINT ( 'NONE',  ( -11.11016527260153630, 31.83082137946488643, 9.500000000000000000 ) ) ;
#12589 = VECTOR ( 'NONE', #37750, 1000.000000000000114 ) ;
#12590 = CARTESIAN_POINT ( 'NONE',  ( 14.84898236231943258, 21.81673761604075779, 10.49999999999999822 ) ) ;
#12591 = VERTEX_POINT ( 'NONE', #13791 ) ;
#12592 = CARTESIAN_POINT ( 'NONE',  ( 22.72806502780237992, 0.6194066608261846740, -21.61851103361042803 ) ) ;
#12593 = EDGE_CURVE ( 'NONE', #36614, #39958, #35132, .T. ) ;
#12594 = CARTESIAN_POINT ( 'NONE',  ( 11.06069781764610305, 34.19033620402622375, -5.000000000000000888 ) ) ;
#12595 = CARTESIAN_POINT ( 'NONE',  ( 10.18324034840045478, 28.21559575157615996, 13.00000000000000178 ) ) ;
#12596 = VERTEX_POINT ( 'NONE', #38578 ) ;
#12597 = CARTESIAN_POINT ( 'NONE',  ( -28.85991493692416299, 0.1377318499120018247, -11.60034766336565504 ) ) ;
#12598 = FACE_OUTER_BOUND ( 'NONE', #33783, .T. ) ;
#12599 = ORIENTED_EDGE ( 'NONE', *, *, #36274, .T. ) ;
#12600 = CARTESIAN_POINT ( 'NONE',  ( 32.11642246959483771, -5.701442053666191612, -11.24895573057437481 ) ) ;
#12601 =( GEOMETRIC_REPRESENTATION_CONTEXT ( 3 ) GLOBAL_UNCERTAINTY_ASSIGNED_CONTEXT ( ( #4703 ) ) GLOBAL_UNIT_ASSIGNED_CONTEXT ( ( #37207, #30717, #34164 ) ) REPRESENTATION_CONTEXT ( 'NONE', 'WORKASPACE' ) );
#12602 = ADVANCED_FACE ( 'NONE', ( #38377 ), #22133, .T. ) ;
#12603 = EDGE_LOOP ( 'NONE', ( #3637, #5857, #34971, #4382 ) ) ;
#12604 = CARTESIAN_POINT ( 'NONE',  ( 15.93457153376149193, 30.96347702964845539, 12.14047268033087690 ) ) ;
#12605 = DIRECTION ( 'NONE',  ( 1.000000000000000000, 0.000000000000000000, 0.000000000000000000 ) ) ;
#12606 = DIRECTION ( 'NONE',  ( 0.000000000000000000, 0.000000000000000000, 1.000000000000000000 ) ) ;
#12607 = CARTESIAN_POINT ( 'NONE',  ( 10.03134041160893375, 26.49437744576689724, 19.99202127657225603 ) ) ;
#12608 = VECTOR ( 'NONE', #2377, 1000.000000000000000 ) ;
#12609 = DIRECTION ( 'NONE',  ( -0.5000000000000038858, -0.8660254037844364872, 0.000000000000000000 ) ) ;
#12610 = ORIENTED_EDGE ( 'NONE', *, *, #28726, .T. ) ;
#12611 = DIRECTION ( 'NONE',  ( -1.000000000000000000, 0.000000000000000000, 0.000000000000000000 ) ) ;
#12612 = CARTESIAN_POINT ( 'NONE',  ( -18.30496497598766581, 9.321025232647617287, -29.99999999999999289 ) ) ;
#12613 = CARTESIAN_POINT ( 'NONE',  ( 19.26948696230200397, 27.85601271560037162, 23.00000000000000355 ) ) ;
#12614 = EDGE_CURVE ( 'NONE', #38107, #13490, #38175, .T. ) ;
#12615 = ADVANCED_FACE ( 'NONE', ( #13588 ), #4248, .F. ) ;
#12616 = CARTESIAN_POINT ( 'NONE',  ( -12.80736835487442349, 15.68301270189233954, 9.000000000000001776 ) ) ;
#12617 = ADVANCED_FACE ( 'NONE', ( #606 ), #6683, .F. ) ;
#12618 = CARTESIAN_POINT ( 'NONE',  ( 4.627278376603056742, 20.58541896761892431, -26.35737439622670664 ) ) ;
#12619 = CARTESIAN_POINT ( 'NONE',  ( 10.75002496752869341, -17.64495920642993454, -28.01020103939122308 ) ) ;
#12620 = CARTESIAN_POINT ( 'NONE',  ( 11.77090408390491305, 15.39748370681878775, 13.00000000000000178 ) ) ;
#12621 = CARTESIAN_POINT ( 'NONE',  ( -9.840690490415104463, 20.46019347195529647, 10.49999999999999467 ) ) ;
#12622 = AXIS2_PLACEMENT_3D ( 'NONE', #36966, #18086, #30476 ) ;
#12623 = ORIENTED_EDGE ( 'NONE', *, *, #32604, .T. ) ;
#12624 = CARTESIAN_POINT ( 'NONE',  ( -15.11672449564866128, 26.08808756446744681, -8.768129095627141822 ) ) ;
#12625 = CARTESIAN_POINT ( 'NONE',  ( -30.14286744058730250, -20.99504498967513300, 17.92354375535250099 ) ) ;
#12626 = CARTESIAN_POINT ( 'NONE',  ( 14.58906216886622431, -25.77273076839362886, -9.713267811317372491 ) ) ;
#12627 = FACE_OUTER_BOUND ( 'NONE', #33457, .T. ) ;
#12628 = ORIENTED_EDGE ( 'NONE', *, *, #29498, .T. ) ;
#12629 = VERTEX_POINT ( 'NONE', #7084 ) ;
#12630 = CARTESIAN_POINT ( 'NONE',  ( -11.71558024193440062, 23.44492113552537660, -17.20205828893062616 ) ) ;
#12631 = CIRCLE ( 'NONE', #38587, 5.999999999999996447 ) ;
#12632 = CARTESIAN_POINT ( 'NONE',  ( -15.73389691588134376, -22.37440482904794337, -16.14369830803590844 ) ) ;
#12633 = EDGE_CURVE ( 'NONE', #36832, #19894, #31880, .T. ) ;
#12634 = FACE_OUTER_BOUND ( 'NONE', #31590, .T. ) ;
#12635 = CIRCLE ( 'NONE', #2894, 0.5000000000000004441 ) ;
#12636 = ORIENTED_EDGE ( 'NONE', *, *, #36600, .T. ) ;
#12637 = CARTESIAN_POINT ( 'NONE',  ( -27.20412735585551900, -7.570742992334142940, -16.78134040425078410 ) ) ;
#12638 = CARTESIAN_POINT ( 'NONE',  ( -13.24729829976488205, -23.61164488198660294, -14.48312679232910760 ) ) ;
#12639 = CARTESIAN_POINT ( 'NONE',  ( 16.58691282011809420, -31.15705289669448064, 11.00000000000000000 ) ) ;
#12640 = ORIENTED_EDGE ( 'NONE', *, *, #34551, .T. ) ;
#12641 = CARTESIAN_POINT ( 'NONE',  ( 21.67083567045098746, 0.9273911989265315459, -23.87724168837842242 ) ) ;
#12642 = ADVANCED_FACE ( 'NONE', ( #25781 ), #7284, .F. ) ;
#12643 = CARTESIAN_POINT ( 'NONE',  ( -6.354454053420244719, 35.54304081427989814, 9.500000000000000000 ) ) ;
#12644 = CARTESIAN_POINT ( 'NONE',  ( 12.37435565298211415, 15.93301270189216545, 7.000000000000000000 ) ) ;
#12645 = ORIENTED_EDGE ( 'NONE', *, *, #33487, .F. ) ;
#12646 = CARTESIAN_POINT ( 'NONE',  ( -22.23112559094391827, 0.6234443325065696095, -22.72982244255366524 ) ) ;
#12647 = EDGE_LOOP ( 'NONE', ( #31709, #32580, #438, #297, #27832, #29479, #14578 ) ) ;
#12648 = CARTESIAN_POINT ( 'NONE',  ( 20.55275704333539011, -0.2804796770642928316, -28.66667438445236726 ) ) ;
#12649 = CARTESIAN_POINT ( 'NONE',  ( 17.84039878628271936, -10.10400010744520571, -30.00000000000005329 ) ) ;
#12650 = CARTESIAN_POINT ( 'NONE',  ( 15.60391421430543524, -26.29546805949240351, 16.87380292611441490 ) ) ;
#12651 = VERTEX_POINT ( 'NONE', #26786 ) ;
#12652 = CARTESIAN_POINT ( 'NONE',  ( -20.85387373749717810, 4.297652806957183103, -24.19551209732460606 ) ) ;
#12653 = CARTESIAN_POINT ( 'NONE',  ( -14.44277748876678302, 26.55045409923029354, 7.000000000000000000 ) ) ;
#12654 = AXIS2_PLACEMENT_3D ( 'NONE', #16485, #28872, #10387 ) ;
#12655 = CARTESIAN_POINT ( 'NONE',  ( 4.137850160811998634, 25.30681243524901447, 21.00000000000000355 ) ) ;
#12656 = CARTESIAN_POINT ( 'NONE',  ( -13.48130249190472796, 27.93180293473203690, 7.499999999999993783 ) ) ;
#12657 = FACE_OUTER_BOUND ( 'NONE', #29124, .T. ) ;
#12658 = VECTOR ( 'NONE', #39106, 1000.000000000000000 ) ;
#12659 = FACE_BOUND ( 'NONE', #38868, .T. ) ;
#12660 = CARTESIAN_POINT ( 'NONE',  ( 22.45707936798469717, 12.96560081831818501, 14.53008259254011136 ) ) ;
#12661 = CARTESIAN_POINT ( 'NONE',  ( -19.69137326279327027, 5.702251777040514114, -30.00000000000000355 ) ) ;
#12662 = CARTESIAN_POINT ( 'NONE',  ( 4.524139159579314118, 31.43208625488810171, 10.49999999999999822 ) ) ;
#12663 = CARTESIAN_POINT ( 'NONE',  ( 3.784364466546041417, 47.62563423532509432, 7.500000000000005329 ) ) ;
#12664 = CARTESIAN_POINT ( 'NONE',  ( 23.94622488899277712, -26.31671797062173113, -7.190667588222269480 ) ) ;
#12665 = CARTESIAN_POINT ( 'NONE',  ( -7.312041872459064784, 25.58773265502866678, 13.00000000000000178 ) ) ;
#12666 = CARTESIAN_POINT ( 'NONE',  ( 10.97710528508702765, 17.90433831621321303, -26.20245233466055623 ) ) ;
#12667 = VERTEX_POINT ( 'NONE', #2216 ) ;
#12668 = CARTESIAN_POINT ( 'NONE',  ( -14.77449872868504421, 22.25468481093715312, -13.59554605823010931 ) ) ;
#12669 = CARTESIAN_POINT ( 'NONE',  ( -20.08365402398563759, -19.49265790308138335, 20.69868183039781329 ) ) ;
#12670 = CARTESIAN_POINT ( 'NONE',  ( 11.41267482483262619, 26.20820393249957192, 12.00000000000000000 ) ) ;
#12671 = CARTESIAN_POINT ( 'NONE',  ( 12.42496545568594968, 20.44575147035703822, -19.50238972058703268 ) ) ;
#12672 = ORIENTED_EDGE ( 'NONE', *, *, #22769, .T. ) ;
#12673 = DIRECTION ( 'NONE',  ( 0.9135454576426059736, 0.4067366430757888285, 0.000000000000000000 ) ) ;
#12674 = ORIENTED_EDGE ( 'NONE', *, *, #19251, .T. ) ;
#12676 = DIRECTION ( 'NONE',  ( -0.000000000000000000, -0.000000000000000000, -1.000000000000000000 ) ) ;
#12675 = CARTESIAN_POINT ( 'NONE',  ( -15.02016821374818534, 26.40324407494122028, -8.755937702507523568 ) ) ;
#12677 = CARTESIAN_POINT ( 'NONE',  ( -15.46270586958304172, -26.44519224899418575, -7.820922189861058804 ) ) ;
#12678 = DIRECTION ( 'NONE',  ( 1.000000000000000000, 0.000000000000000000, 0.000000000000000000 ) ) ;
#12679 = EDGE_LOOP ( 'NONE', ( #11739, #5119, #1016, #32761, #30456 ) ) ;
#12680 = CARTESIAN_POINT ( 'NONE',  ( -23.75646719861951439, -12.44796170920469613, -18.61696717325561323 ) ) ;
#12681 = CARTESIAN_POINT ( 'NONE',  ( -14.16578816422650711, -25.94200127604465678, -8.776735216617021607 ) ) ;
#12682 = FACE_OUTER_BOUND ( 'NONE', #4252, .T. ) ;
#12683 = CARTESIAN_POINT ( 'NONE',  ( 14.11166830150711426, 19.77494500827953772, -17.62012407019295779 ) ) ;
#12684 = ORIENTED_EDGE ( 'NONE', *, *, #32149, .T. ) ;
#12685 = CARTESIAN_POINT ( 'NONE',  ( 19.82805615916967312, 5.207665154685881426, -30.00000000000000355 ) ) ;
#12686 = CARTESIAN_POINT ( 'NONE',  ( 0.5000000000000000000, 37.00000000000000711, 7.000000000000000000 ) ) ;
#12687 = CARTESIAN_POINT ( 'NONE',  ( 6.789742187716170108, 35.87551282667536157, 7.455539900862802938 ) ) ;
#12688 = CARTESIAN_POINT ( 'NONE',  ( -10.81260707898136708, 32.90853150812171179, 10.49999999999999822 ) ) ;
#12689 = VECTOR ( 'NONE', #39854, 1000.000000000000000 ) ;
#12690 = VERTEX_POINT ( 'NONE', #39379 ) ;
#12691 = CARTESIAN_POINT ( 'NONE',  ( -21.32151666823140701, 0.4344076493211833645, -24.97710971221515663 ) ) ;
#12692 = CARTESIAN_POINT ( 'NONE',  ( 25.34039414564677983, 0.1439692079819893111, -17.40756292650477022 ) ) ;
#12693 = VECTOR ( 'NONE', #22127, 1000.000000000000114 ) ;
#12694 = CARTESIAN_POINT ( 'NONE',  ( 28.40703083259912987, -13.04618529600540811, 20.50957957746029336 ) ) ;
#12695 = ORIENTED_EDGE ( 'NONE', *, *, #26182, .T. ) ;
#12696 = CARTESIAN_POINT ( 'NONE',  ( 5.636483973512840251, -22.01575377102106046, -21.50719306941234876 ) ) ;
#12697 = FACE_OUTER_BOUND ( 'NONE', #19330, .T. ) ;
#12698 = VERTEX_POINT ( 'NONE', #30042 ) ;
#12699 = DIRECTION ( 'NONE',  ( 0.2185080122244111578, -0.6724985119639586006, -0.7071067811865462405 ) ) ;
#12700 = LINE ( 'NONE', #2578, #7145 ) ;
#12701 = DIRECTION ( 'NONE',  ( 0.000000000000000000, 0.000000000000000000, 1.000000000000000000 ) ) ;
#12702 = CARTESIAN_POINT ( 'NONE',  ( 3.826396457843638022, 37.43840591691041908, -7.552972810893269440 ) ) ;
#12703 = DIRECTION ( 'NONE',  ( -1.000000000000000000, 0.000000000000000000, 0.000000000000000000 ) ) ;
#12704 = EDGE_CURVE ( 'NONE', #36810, #39240, #3894, .T. ) ;
#12705 = CARTESIAN_POINT ( 'NONE',  ( -8.412270287199726582, 10.07085245822961994, 11.00000000000000000 ) ) ;
#12706 = DIRECTION ( 'NONE',  ( 0.9945218953682729568, -0.1045284632676570929, -0.000000000000000000 ) ) ;
#12707 = VECTOR ( 'NONE', #33740, 1000.000000000000000 ) ;
#12708 = DIRECTION ( 'NONE',  ( 1.000000000000000000, 0.000000000000000000, 0.000000000000000000 ) ) ;
#12709 = DIRECTION ( 'NONE',  ( -0.9510565162951504226, 0.3090169943749573322, 0.000000000000000000 ) ) ;
#12710 = DIRECTION ( 'NONE',  ( -0.8090169943749426773, 0.5877852522924796874, 0.000000000000000000 ) ) ;
#12711 = CARTESIAN_POINT ( 'NONE',  ( 10.15111435463817280, 17.86907098534008043, -28.67154087780474470 ) ) ;
#12713 = AXIS2_PLACEMENT_3D ( 'NONE', #17234, #17438, #38349 ) ;
#12712 = CARTESIAN_POINT ( 'NONE',  ( 13.05736835487433289, 16.11602540378438420, 10.50000000000000178 ) ) ;
#12714 = ORIENTED_EDGE ( 'NONE', *, *, #13395, .F. ) ;
#12717 = AXIS2_PLACEMENT_3D ( 'NONE', #22754, #28859, #35159 ) ;
#12716 = DIRECTION ( 'NONE',  ( 0.000000000000000000, -0.000000000000000000, -1.000000000000000000 ) ) ;
#12715 = CARTESIAN_POINT ( 'NONE',  ( -15.04174557779704635, 14.20451568885117588, -27.10768944337526065 ) ) ;
#12718 = EDGE_CURVE ( 'NONE', #26207, #14734, #20299, .T. ) ;
#12719 = DIRECTION ( 'NONE',  ( 0.000000000000000000, 0.000000000000000000, -1.000000000000000000 ) ) ;
#12720 = CIRCLE ( 'NONE', #33512, 0.9999999999999996669 ) ;
#12721 = CARTESIAN_POINT ( 'NONE',  ( 9.562392075367188937, -18.27749775416154066, -28.07786222914176477 ) ) ;
#12722 = ADVANCED_FACE ( 'NONE', ( #5254 ), #6747, .T. ) ;
#12723 = CARTESIAN_POINT ( 'NONE',  ( -19.98910163558307573, -25.17004345428989609, -11.28674626201566511 ) ) ;
#12724 = CARTESIAN_POINT ( 'NONE',  ( 15.33919115406833278, 26.61414219747821619, -6.888072233219839191 ) ) ;
#12725 = CARTESIAN_POINT ( 'NONE',  ( 13.75833282284662751, 23.42126009408847409, -14.47362935452958155 ) ) ;
#12726 = ORIENTED_EDGE ( 'NONE', *, *, #8815, .T. ) ;
#12727 = CARTESIAN_POINT ( 'NONE',  ( -6.282361020112269934, 14.70372268239681368, 10.00000000000000000 ) ) ;
#12728 = CARTESIAN_POINT ( 'NONE',  ( -15.16405052498309836, -26.37334731087130990, -7.828243992827849773 ) ) ;
#12729 = CARTESIAN_POINT ( 'NONE',  ( -36.21547910512273916, -5.268304678878102720, 13.32518128616653286 ) ) ;
#12730 = CARTESIAN_POINT ( 'NONE',  ( -16.15747483659607298, -12.61697622026560772, -30.00000000000000711 ) ) ;
#12731 = CARTESIAN_POINT ( 'NONE',  ( -2.540214017920780165, -24.49585459483449412, -8.898735351503297863 ) ) ;
#12732 = CARTESIAN_POINT ( 'NONE',  ( 15.75662360411219787, 25.59993261007102561, -4.999999999999999112 ) ) ;
#12733 = CARTESIAN_POINT ( 'NONE',  ( 20.75214263285785421, 9.441152523992672130, -16.96792007788538115 ) ) ;
#12734 = CARTESIAN_POINT ( 'NONE',  ( 11.56932667689157057, 32.06810925246610822, 10.49999999999999645 ) ) ;
#12735 = ORIENTED_EDGE ( 'NONE', *, *, #6145, .T. ) ;
#12736 = CARTESIAN_POINT ( 'NONE',  ( -28.94549850962602378, -2.870772275164490850, -14.18330164410991401 ) ) ;
#12737 = CARTESIAN_POINT ( 'NONE',  ( -21.00262217608306869, 5.738642561619127669, 19.27171037444162494 ) ) ;
#12738 = ORIENTED_EDGE ( 'NONE', *, *, #27897, .F. ) ;
#12739 = LINE ( 'NONE', #21689, #3072 ) ;
#12740 = ADVANCED_FACE ( 'NONE', ( #20707 ), #33305, .T. ) ;
#12741 = CARTESIAN_POINT ( 'NONE',  ( -14.36830325120616081, 20.48707633493503977, 11.00000000000000000 ) ) ;
#12742 = EDGE_CURVE ( 'NONE', #4655, #20339, #6353, .T. ) ;
#12743 = CARTESIAN_POINT ( 'NONE',  ( -27.43844334215360448, 0.5923872920799873043, -13.53615638127614318 ) ) ;
#12744 = CARTESIAN_POINT ( 'NONE',  ( 35.11830485971632498, -14.14517689978181103, -6.284369114096038267 ) ) ;
#12745 = CARTESIAN_POINT ( 'NONE',  ( 31.16314261583367085, -24.50336240592831416, 13.32518128616608344 ) ) ;
#12746 = AXIS2_PLACEMENT_3D ( 'NONE', #11887, #5192, #2151 ) ;
#12747 = AXIS2_PLACEMENT_3D ( 'NONE', #7176, #296, #3932 ) ;
#12748 = ORIENTED_EDGE ( 'NONE', *, *, #20565, .T. ) ;
#12749 = DIRECTION ( 'NONE',  ( 0.9781476007338042455, -0.2079116908177664480, 0.000000000000000000 ) ) ;
#12750 = VERTEX_POINT ( 'NONE', #11357 ) ;
#12751 = CARTESIAN_POINT ( 'NONE',  ( 4.591666147298500533, 15.32946292166668556, 9.000000000000001776 ) ) ;
#12752 = CARTESIAN_POINT ( 'NONE',  ( 22.48079666814421884, 18.61591633950141755, 22.99999999999999645 ) ) ;
#12753 = B_SPLINE_CURVE_WITH_KNOTS ( 'NONE', 3,
 ( #36052, #2719, #15109, #21403, #5364, #5561, #27497, #33016, #21010, #23852, #39690, #26899, #20617, #9014, #30357, #33611, #36648, #12059 ),
 .UNSPECIFIED., .F., .F.,
 ( 4, 2, 2, 2, 2, 2, 2, 2, 4 ),
 ( 0.000000000000000000, 0.1250000000000000000, 0.2500000000000000000, 0.3750000000000000000, 0.5000000000000000000, 0.6250000000000000000, 0.7500000000000000000, 0.8750000000000000000, 1.000000000000000000 ),
 .UNSPECIFIED. ) ;
#12754 = DIRECTION ( 'NONE',  ( 0.000000000000000000, 0.000000000000000000, 1.000000000000000000 ) ) ;
#12755 = ORIENTED_EDGE ( 'NONE', *, *, #3069, .F. ) ;
#12756 = CARTESIAN_POINT ( 'NONE',  ( -3.992774750912768678, 35.67860805316688300, -10.18623164847826423 ) ) ;
#12757 = CARTESIAN_POINT ( 'NONE',  ( -9.427394962683591118, 11.06314620782489833, 10.49999999999999822 ) ) ;
#12758 = CARTESIAN_POINT ( 'NONE',  ( -19.48557158514998022, -11.24999999999982414, 3.000000000000000000 ) ) ;
#12759 = CARTESIAN_POINT ( 'NONE',  ( -7.848705329595171420, 10.27943253798625989, 10.66666666666666607 ) ) ;
#12760 = SHAPE_REPRESENTATION ( 'Protective Travel Cap', ( #24238 ), #31997 ) ;
#12762 = ADVANCED_FACE ( 'NONE', ( #32901 ), #35938, .T. ) ;
#12761 = CYLINDRICAL_SURFACE ( 'NONE', #22964, 1.000000000000000000 ) ;
#12763 = FACE_OUTER_BOUND ( 'NONE', #5461, .T. ) ;
#12764 = CARTESIAN_POINT ( 'NONE',  ( 13.73220224370217579, 30.78478150535875457, -5.457670766714417532 ) ) ;
#12765 = ORIENTED_EDGE ( 'NONE', *, *, #8884, .F. ) ;
#12766 = CARTESIAN_POINT ( 'NONE',  ( -17.99203688690355207, 9.826896140120286560, -29.99999999999999289 ) ) ;
#12767 = DIRECTION ( 'NONE',  ( 1.000000000000000000, 0.000000000000000000, 0.000000000000000000 ) ) ;
#12768 = CARTESIAN_POINT ( 'NONE',  ( 9.772342709178570175, -18.26604441824505187, -27.43687354787681087 ) ) ;
#12769 = LINE ( 'NONE', #3828, #6802 ) ;
#12770 = CARTESIAN_POINT ( 'NONE',  ( 14.81731930227308425, 25.68027610000711292, -10.17593115926348091 ) ) ;
#12771 = CARTESIAN_POINT ( 'NONE',  ( 35.36940577612500647, -20.42053594592276866, -4.999999999999997335 ) ) ;
#12772 = CARTESIAN_POINT ( 'NONE',  ( -10.33648234394568632, 33.08013173297169374, 10.49999999999999467 ) ) ;
#12773 = AXIS2_PLACEMENT_3D ( 'NONE', #18600, #28525, #30983 ) ;
#12774 = CONICAL_SURFACE ( 'NONE', #11484, 1.000000000000002665, 0.7853981633974530530 ) ;
#12775 = CARTESIAN_POINT ( 'NONE',  ( -20.65407906065966515, -20.62528606208020321, -15.83079615351305058 ) ) ;
#12776 = CARTESIAN_POINT ( 'NONE',  ( 9.344820083231123675, -20.32964934627687015, -21.78656791573911633 ) ) ;
#12777 = CARTESIAN_POINT ( 'NONE',  ( 13.59683655979047145, 22.61026046561213576, -15.46554287034021158 ) ) ;
#12778 = CARTESIAN_POINT ( 'NONE',  ( 29.83403652028378517, -20.21430139748671806, -10.17890540654461695 ) ) ;
#12779 = CARTESIAN_POINT ( 'NONE',  ( 13.48130249190479191, 27.93180293473185927, 10.49999999999999822 ) ) ;
#12780 = DIRECTION ( 'NONE',  ( 1.000000000000000000, 0.000000000000000000, 0.000000000000000000 ) ) ;
#12781 = VERTEX_POINT ( 'NONE', #10750 ) ;
#12782 = CARTESIAN_POINT ( 'NONE',  ( -7.438509353473058638, 24.90914914033339755, -18.85218860379452366 ) ) ;
#12783 = CARTESIAN_POINT ( 'NONE',  ( -1.871208588069141143, 13.69667159339610762, 6.000000000000000000 ) ) ;
#12784 = LINE ( 'NONE', #9746, #36694 ) ;
#12785 = AXIS2_PLACEMENT_3D ( 'NONE', #12121, #9677, #15365 ) ;
#12786 = CARTESIAN_POINT ( 'NONE',  ( 11.77090408390491305, 15.39748370681878775, 13.00000000000000178 ) ) ;
#12787 = ORIENTED_EDGE ( 'NONE', *, *, #12213, .F. ) ;
#12788 = CARTESIAN_POINT ( 'NONE',  ( 21.70460829199038244, 0.7520035140130953977, -23.85688495828296496 ) ) ;
#12789 = DIRECTION ( 'NONE',  ( 0.000000000000000000, 0.000000000000000000, 1.000000000000000000 ) ) ;
#12790 = EDGE_CURVE ( 'NONE', #36749, #38004, #35536, .T. ) ;
#12791 = CARTESIAN_POINT ( 'NONE',  ( -12.83926296998452798, 26.67172942406192604, 7.000000000000000000 ) ) ;
#12792 = EDGE_CURVE ( 'NONE', #14009, #33298, #14603, .T. ) ;
#12793 = ORIENTED_EDGE ( 'NONE', *, *, #10502, .F. ) ;
#12794 = CARTESIAN_POINT ( 'NONE',  ( -30.86332187973009056, -0.0005132856539958949174, -4.999999999999999112 ) ) ;
#12795 = DIRECTION ( 'NONE',  ( -0.4731467892558211541, -0.5254827454987550661, -0.7071067811865462405 ) ) ;
#12796 = ORIENTED_EDGE ( 'NONE', *, *, #22264, .F. ) ;
#12797 = CARTESIAN_POINT ( 'NONE',  ( 29.92351859954650095, -6.183656610847034329, -13.99975621931235636 ) ) ;
#12798 = EDGE_LOOP ( 'NONE', ( #20149, #6523, #166, #15895, #27431 ) ) ;
#12799 = CARTESIAN_POINT ( 'NONE',  ( -5.638963013753754971, 39.23975437003352340, 13.32518128616608521 ) ) ;
#12800 = DIRECTION ( 'NONE',  ( -1.000000000000000000, 0.000000000000000000, 0.000000000000000000 ) ) ;
#12801 = CARTESIAN_POINT ( 'NONE',  ( -7.713869163866016621, 10.18146832927085121, 10.50000000000000711 ) ) ;
#12802 = CARTESIAN_POINT ( 'NONE',  ( -5.180310612586867869, 33.71427074068270002, 19.27171037444158586 ) ) ;
#12803 = CIRCLE ( 'NONE', #38081, 1.000000000000000888 ) ;
#12804 = DIRECTION ( 'NONE',  ( 0.000000000000000000, 0.000000000000000000, -1.000000000000000000 ) ) ;
#12805 = ORIENTED_EDGE ( 'NONE', *, *, #31466, .T. ) ;
#12806 = PLANE ( 'NONE',  #14458 ) ;
#12807 = CARTESIAN_POINT ( 'NONE',  ( -20.39749650821323712, -2.159697320963449130, -30.00000000000000355 ) ) ;
#12808 = DIRECTION ( 'NONE',  ( 0.000000000000000000, 0.000000000000000000, 1.000000000000000000 ) ) ;
#12809 = VECTOR ( 'NONE', #18805, 1000.000000000000000 ) ;
#12810 = CARTESIAN_POINT ( 'NONE',  ( 13.13581098909226696, 27.45627467658428955, 7.500000000000000888 ) ) ;
#12811 = EDGE_CURVE ( 'NONE', #32326, #163, #5054, .T. ) ;
#12812 = CARTESIAN_POINT ( 'NONE',  ( 13.91075386486431320, 15.49308367278315046, -26.46882179040325056 ) ) ;
#12813 = CIRCLE ( 'NONE', #23867, 1.000000000000000000 ) ;
#12814 = CARTESIAN_POINT ( 'NONE',  ( 5.194277563714346790, 20.21734125709076224, -27.07613456391705853 ) ) ;
#12815 = EDGE_CURVE ( 'NONE', #15842, #333, #13993, .T. ) ;
#12816 = CARTESIAN_POINT ( 'NONE',  ( 13.32124143939226713, -19.97798892781937141, -20.26999631390010848 ) ) ;
#12817 = CARTESIAN_POINT ( 'NONE',  ( 4.096822963000107620, 8.035697679810645866, 11.00000000000000000 ) ) ;
#12818 = DIRECTION ( 'NONE',  ( -0.000000000000000000, -0.000000000000000000, -1.000000000000000000 ) ) ;
#12819 = VERTEX_POINT ( 'NONE', #2807 ) ;
#12820 = CARTESIAN_POINT ( 'NONE',  ( -14.93905414659889352, 25.78616324827421735, -9.709672390330473135 ) ) ;
#12821 = CARTESIAN_POINT ( 'NONE',  ( -33.92416433109639229, -10.98373637526240643, 17.92354375535328614 ) ) ;
#12822 = CARTESIAN_POINT ( 'NONE',  ( 9.420782162276523763, -18.34804325365140798, -28.08566532578938180 ) ) ;
#12823 = DIRECTION ( 'NONE',  ( 1.000000000000000000, 0.000000000000000000, 0.000000000000000000 ) ) ;
#12824 = EDGE_LOOP ( 'NONE', ( #29813, #1627, #7520, #26874 ) ) ;
#12825 = ORIENTED_EDGE ( 'NONE', *, *, #2219, .F. ) ;
#12826 = AXIS2_PLACEMENT_3D ( 'NONE', #11824, #30522, #2682 ) ;
#12827 = CARTESIAN_POINT ( 'NONE',  ( -13.71280609171516218, 27.90080846771834544, -10.50245461074293196 ) ) ;
#12828 = CARTESIAN_POINT ( 'NONE',  ( -11.29934442612571388, -17.60818932157431149, -26.68958922436052106 ) ) ;
#12829 = FACE_BOUND ( 'NONE', #32113, .T. ) ;
#12830 = CIRCLE ( 'NONE', #27742, 1.000000000000000000 ) ;
#12831 = VECTOR ( 'NONE', #30982, 1000.000000000000000 ) ;
#12832 = VERTEX_POINT ( 'NONE', #21098 ) ;
#12833 = CARTESIAN_POINT ( 'NONE',  ( -20.38661749552379732, -6.361484682545848202, -25.69238726493766833 ) ) ;
#12834 = CARTESIAN_POINT ( 'NONE',  ( -10.13786778044513959, -19.19472683054627637, -23.86456005356567545 ) ) ;
#12835 = CARTESIAN_POINT ( 'NONE',  ( -13.59328760765163224, 16.15712598384885013, 7.083533146543740777 ) ) ;
#12836 = VERTEX_POINT ( 'NONE', #12347 ) ;
#12837 = CARTESIAN_POINT ( 'NONE',  ( 21.53391398595842077, 1.629941546267092756, -23.95798976520841705 ) ) ;
#12838 = DIRECTION ( 'NONE',  ( -0.4067366430757888840, 0.9135454576426058626, 0.000000000000000000 ) ) ;
#12839 = DIRECTION ( 'NONE',  ( 1.000000000000000000, 0.000000000000000000, 0.000000000000000000 ) ) ;
#12840 = AXIS2_PLACEMENT_3D ( 'NONE', #27495, #39880, #6349 ) ;
#12841 = ORIENTED_EDGE ( 'NONE', *, *, #11042, .T. ) ;
#12842 = ADVANCED_FACE ( 'NONE', ( #11954 ), #5854, .T. ) ;
#12843 = CARTESIAN_POINT ( 'NONE',  ( -28.91287382066377631, 0.07518806480736967002, -11.59674810764759201 ) ) ;
#12845 = ADVANCED_FACE ( 'NONE', ( #21884 ), #24344, .F. ) ;
#12844 = EDGE_LOOP ( 'NONE', ( #32160, #28141, #10123, #35913 ) ) ;
#12846 = CARTESIAN_POINT ( 'NONE',  ( 31.83309823342235489, -1.783519987017442077, -8.218906981704529713 ) ) ;
#12847 = CARTESIAN_POINT ( 'NONE',  ( 19.82764311455687078, -5.383684237423299379, -29.99999999999997513 ) ) ;
#12848 = CARTESIAN_POINT ( 'NONE',  ( 30.57450045107875169, -0.3656520783190762014, 16.87380292611442201 ) ) ;
#12849 = VERTEX_POINT ( 'NONE', #24139 ) ;
#12850 = CYLINDRICAL_SURFACE ( 'NONE', #38342, 1.000000000000000000 ) ;
#12851 = CARTESIAN_POINT ( 'NONE',  ( -3.025308588020407363, 26.48089285804710613, 20.99999999999998934 ) ) ;
#12852 = CARTESIAN_POINT ( 'NONE',  ( -13.49038105676664223, 15.86602540378456361, 10.49999999999999822 ) ) ;
#12853 = CARTESIAN_POINT ( 'NONE',  ( -7.713869163866016621, 10.18146832927085121, 11.00000000000000000 ) ) ;
#12854 = EDGE_CURVE ( 'NONE', #29281, #29040, #19350, .T. ) ;
#12855 = AXIS2_PLACEMENT_3D ( 'NONE', #34183, #9600, #36828 ) ;
#12856 = FACE_BOUND ( 'NONE', #7609, .T. ) ;
#12857 = EDGE_CURVE ( 'NONE', #10635, #19442, #33703, .T. ) ;
#12858 = CARTESIAN_POINT ( 'NONE',  ( 23.18947492591157555, 13.38844959084118358, 11.00000000000000000 ) ) ;
#12859 = CARTESIAN_POINT ( 'NONE',  ( -23.50810587197001311, 8.940726895909143934, -6.932906322231784380 ) ) ;
#12860 = CARTESIAN_POINT ( 'NONE',  ( 20.78048496889905650, -24.27834333958334412, -12.16204984203799988 ) ) ;
#12861 = CONICAL_SURFACE ( 'NONE', #3791, 0.4999999999999897304, 0.7853981633974508325 ) ;
#12862 = LINE ( 'NONE', #37650, #6003 ) ;
#12863 = CARTESIAN_POINT ( 'NONE',  ( 15.35355722042785054, 26.91131673440186844, -5.944390809853191904 ) ) ;
#12864 = EDGE_LOOP ( 'NONE', ( #35534, #8312, #19786, #7983 ) ) ;
#12865 = CARTESIAN_POINT ( 'NONE',  ( -13.53391903102045113, 18.98539088064760705, -19.68245357048784783 ) ) ;
#12866 = EDGE_CURVE ( 'NONE', #32396, #33978, #40121, .T. ) ;
#12867 = CARTESIAN_POINT ( 'NONE',  ( -26.04200899061306274, -18.69117426458536357, 20.25080042701566541 ) ) ;
#12868 = CARTESIAN_POINT ( 'NONE',  ( 10.17939521785132051, 33.00296324411745275, 10.49999999999999822 ) ) ;
#12869 = CARTESIAN_POINT ( 'NONE',  ( 14.55518902956964666, 24.90832010759994120, -11.60082918595498036 ) ) ;
#12870 = ORIENTED_EDGE ( 'NONE', *, *, #15601, .T. ) ;
#12871 = FACE_OUTER_BOUND ( 'NONE', #36277, .T. ) ;
#12872 = ORIENTED_EDGE ( 'NONE', *, *, #29294, .F. ) ;
#12874 = DIRECTION ( 'NONE',  ( -1.000000000000000000, 0.000000000000000000, 0.000000000000000000 ) ) ;
#12873 = CARTESIAN_POINT ( 'NONE',  ( -12.27358052226857765, 20.64665722953253635, -19.47164098058547665 ) ) ;
#12875 = CARTESIAN_POINT ( 'NONE',  ( -15.63755959170095089, -26.78052150289263622, -5.000000000000000888 ) ) ;
#12876 = CARTESIAN_POINT ( 'NONE',  ( 7.330070799514983193, 27.28854476845134513, 6.000000000000000000 ) ) ;
#12877 = ORIENTED_EDGE ( 'NONE', *, *, #28544, .F. ) ;
#12878 = CARTESIAN_POINT ( 'NONE',  ( -34.54285066864272835, -16.78341526201209533, -5.000000000000000000 ) ) ;
#12879 = CARTESIAN_POINT ( 'NONE',  ( -13.78313613767150692, -25.73547777514550106, -9.253468020048730480 ) ) ;
#12880 = DIRECTION ( 'NONE',  ( 0.1045284632676570929, 0.9945218953682730678, 0.000000000000000000 ) ) ;
#12881 = CARTESIAN_POINT ( 'NONE',  ( 12.67230126945890412, 16.91222923427146085, -25.18277393341357850 ) ) ;
#12882 = EDGE_LOOP ( 'NONE', ( #28157, #39625, #5932 ) ) ;
#12883 = CARTESIAN_POINT ( 'NONE',  ( 19.64403038794415224, 5.908213622717614300, -29.41334968421891816 ) ) ;
#12884 = CARTESIAN_POINT ( 'NONE',  ( -0.5000000000000004441, 36.50000000000000711, 7.500000000000000888 ) ) ;
#12885 = CARTESIAN_POINT ( 'NONE',  ( 14.57486473880226185, 26.18419839932902349, 10.50000000000000533 ) ) ;
#12886 = DIRECTION ( 'NONE',  ( 0.9945218953682729568, -0.1045284632676569680, 0.000000000000000000 ) ) ;
#12887 = ORIENTED_EDGE ( 'NONE', *, *, #2842, .T. ) ;
#12888 = ADVANCED_FACE ( 'NONE', ( #9307 ), #31046, .F. ) ;
#12889 = CARTESIAN_POINT ( 'NONE',  ( -21.36309669107243892, 0.09765983062926059111, -24.94016949773846292 ) ) ;
#12890 = ADVANCED_FACE ( 'NONE', ( #5648 ), #3210, .T. ) ;
#12892 = CARTESIAN_POINT ( 'NONE',  ( 20.48743909015156106, 0.7225425954259894201, -30.00000000000000000 ) ) ;
#12891 = CIRCLE ( 'NONE', #35605, 1.000000000000000000 ) ;
#12893 = AXIS2_PLACEMENT_3D ( 'NONE', #20277, #8685, #30018 ) ;
#12894 = CARTESIAN_POINT ( 'NONE',  ( 19.10350568547219297, -22.04057959011761625, 19.99202127657101968 ) ) ;
#12895 = ORIENTED_EDGE ( 'NONE', *, *, #12587, .T. ) ;
#12896 = CONICAL_SURFACE ( 'NONE', #2528, 1.000000000000007772, 0.7853981633974554954 ) ;
#12897 = CARTESIAN_POINT ( 'NONE',  ( -16.77267017469754151, -29.13948811618693924, -5.000000000000000000 ) ) ;
#12898 = DIRECTION ( 'NONE',  ( 0.000000000000000000, 0.000000000000000000, 1.000000000000000000 ) ) ;
#12899 = ORIENTED_EDGE ( 'NONE', *, *, #34199, .T. ) ;
#12900 = CARTESIAN_POINT ( 'NONE',  ( -9.697889840765284930, 31.90483559858340357, 10.50000000000000000 ) ) ;
#12901 = DIRECTION ( 'NONE',  ( 0.000000000000000000, 0.000000000000000000, 1.000000000000000000 ) ) ;
#12902 = CARTESIAN_POINT ( 'NONE',  ( -5.947717410344459665, 34.62949535663729250, 9.500000000000000000 ) ) ;
#12903 = CARTESIAN_POINT ( 'NONE',  ( 4.462315839921594751, 27.28163392174084123, -17.66356109337273494 ) ) ;
#12904 = EDGE_CURVE ( 'NONE', #4586, #5579, #11568, .T. ) ;
#12905 = CARTESIAN_POINT ( 'NONE',  ( 9.997483185316561105, 21.95197631500756685, 10.00000000000000000 ) ) ;
#12906 = CARTESIAN_POINT ( 'NONE',  ( 14.70550430380716023, 20.45163507617042242, 10.87262190629277647 ) ) ;
#12907 = DIRECTION ( 'NONE',  ( -0.000000000000000000, -0.000000000000000000, -1.000000000000000000 ) ) ;
#12908 = FACE_OUTER_BOUND ( 'NONE', #24879, .T. ) ;
#12909 = CARTESIAN_POINT ( 'NONE',  ( 13.37378135583784911, 20.59160479820249634, 7.000000000000000000 ) ) ;
#12910 = CARTESIAN_POINT ( 'NONE',  ( -0.5000000000000004441, 36.50000000000000711, 7.500000000000000888 ) ) ;
#12911 = CIRCLE ( 'NONE', #35640, 1.000000000000002665 ) ;
#12912 = CARTESIAN_POINT ( 'NONE',  ( 10.62804704006517653, 18.54916539939932463, -24.92187189847329165 ) ) ;
#12913 = CARTESIAN_POINT ( 'NONE',  ( 13.30736835483207692, 15.77027916469364577, 10.49999999999999822 ) ) ;
#12914 = AXIS2_PLACEMENT_3D ( 'NONE', #39547, #14967, #36506 ) ;
#12915 = EDGE_LOOP ( 'NONE', ( #3053, #4455, #21058, #19989 ) ) ;
#12917 = CARTESIAN_POINT ( 'NONE',  ( 2.629601561899396422, 7.723830143584014429, 10.50000000000000533 ) ) ;
#12916 = CARTESIAN_POINT ( 'NONE',  ( -18.31827171329678450, 17.14654578878874602, -10.34362890045172279 ) ) ;
#12918 = CARTESIAN_POINT ( 'NONE',  ( 12.74038105676654453, 14.56698729810772264, 11.00000000000000000 ) ) ;
#12919 = CARTESIAN_POINT ( 'NONE',  ( 10.82536310076888952, -19.99331871519654769, -21.61878681921504608 ) ) ;
#12920 = CARTESIAN_POINT ( 'NONE',  ( 14.33346043011691329, 20.15556903647874165, 10.66666666666666963 ) ) ;
#12921 = CARTESIAN_POINT ( 'NONE',  ( 11.31067235875530130, 18.03752733997335511, -25.01467926984602030 ) ) ;
#12922 = CARTESIAN_POINT ( 'NONE',  ( 12.64338984711987379, 21.06830844464534991, -18.45004776435698446 ) ) ;
#12923 = AXIS2_PLACEMENT_3D ( 'NONE', #9165, #30901, #15861 ) ;
#12924 = B_SPLINE_SURFACE_WITH_KNOTS ( 'NONE', 1, 3, ( 
 ( #39422, #39623, #11202, #11605, #21142, #20944, #24185, #2065, #26634, #36581 ),
 ( #23593, #4702, #33148, #33351, #4903, #20351, #1866, #5301, #17107, #35989 ) ),
 .UNSPECIFIED., .F., .F., .F.,
 ( 2, 2 ),
 ( 4, 2, 2, 2, 4 ),
 ( 0.000000000000000000, 1.000000000000000000 ),
 ( 4.563205465131944472, 4.955904546830669943, 5.348603628529396303, 5.741302710228122663, 6.134001791926849023 ),
 .UNSPECIFIED. ) ;
#12925 = ORIENTED_EDGE ( 'NONE', *, *, #31386, .T. ) ;
#12926 = LINE ( 'NONE', #15182, #8168 ) ;
#12927 = CARTESIAN_POINT ( 'NONE',  ( -15.37705579490140195, -26.68840604134194194, -5.946092059939837249 ) ) ;
#12928 = CARTESIAN_POINT ( 'NONE',  ( -37.31659891191868184, -12.87518290988868586, 12.73282698324829809 ) ) ;
#12929 = CARTESIAN_POINT ( 'NONE',  ( -17.04493828242456033, -12.50648979017474538, -26.27989544973046421 ) ) ;
#12930 = CARTESIAN_POINT ( 'NONE',  ( -3.977639621222068378, -22.37851689048354942, -17.96835865857241643 ) ) ;
#12931 = CARTESIAN_POINT ( 'NONE',  ( 11.52998930085336937, 17.50220035821725162, -26.26108509606446617 ) ) ;
#12932 = VERTEX_POINT ( 'NONE', #3400 ) ;
#12933 = CARTESIAN_POINT ( 'NONE',  ( 21.27561741872812462, 9.625452138548039827, -14.90836893165563914 ) ) ;
#12934 = FACE_OUTER_BOUND ( 'NONE', #39529, .T. ) ;
#12935 = CARTESIAN_POINT ( 'NONE',  ( -11.88159808435120013, 30.55960002361344507, 17.92354375535250810 ) ) ;
#12936 = ORIENTED_EDGE ( 'NONE', *, *, #15353, .F. ) ;
#12937 = CARTESIAN_POINT ( 'NONE',  ( -32.22282324793545172, -3.298326783855909827, -9.525552920251982414 ) ) ;
#12938 = CARTESIAN_POINT ( 'NONE',  ( -18.88552629894566692, 10.90356369248249280, 18.87996532025784546 ) ) ;
#12939 = EDGE_LOOP ( 'NONE', ( #8608, #17877 ) ) ;
#12940 = CARTESIAN_POINT ( 'NONE',  ( 23.98526753813946044, -9.069922861307770035, 20.99999999999999645 ) ) ;
#12941 = CARTESIAN_POINT ( 'NONE',  ( 24.37710423125464487, -10.07883586999013303, 23.00000000000000000 ) ) ;
#12942 = EDGE_CURVE ( 'NONE', #21619, #31370, #39454, .T. ) ;
#12943 = CARTESIAN_POINT ( 'NONE',  ( -21.22731311515731534, 1.116805269015000990, -25.05052939645603516 ) ) ;
#12944 = CARTESIAN_POINT ( 'NONE',  ( 22.78213498135489701, -9.193927964998984237, -20.75049135688346169 ) ) ;
#12945 = CARTESIAN_POINT ( 'NONE',  ( 18.86510067431754933, -28.79249900932126849, 13.92931973827835002 ) ) ;
#12946 = CIRCLE ( 'NONE', #23341, 6.000000000000015987 ) ;
#12947 = ORIENTED_EDGE ( 'NONE', *, *, #2912, .F. ) ;
#12948 = EDGE_LOOP ( 'NONE', ( #28906, #25288 ) ) ;
#12949 = ADVANCED_FACE ( 'NONE', ( #36939 ), #30450, .F. ) ;
#12950 = AXIS2_PLACEMENT_3D ( 'NONE', #28392, #3019, #31249 ) ;
#12951 = DIRECTION ( 'NONE',  ( -0.000000000000000000, -0.000000000000000000, -1.000000000000000000 ) ) ;
#12952 = CYLINDRICAL_SURFACE ( 'NONE', #39685, 0.5000000000000000000 ) ;
#12953 = DIRECTION ( 'NONE',  ( 0.3090169943749450643, -0.9510565162951544194, 0.000000000000000000 ) ) ;
#12954 = VERTEX_POINT ( 'NONE', #24939 ) ;
#12955 = CARTESIAN_POINT ( 'NONE',  ( -2.308138231165596466, 21.01458932961489978, -26.27989553671341483 ) ) ;
#12956 = DIRECTION ( 'NONE',  ( -0.000000000000000000, -0.000000000000000000, -1.000000000000000000 ) ) ;
#12957 = CARTESIAN_POINT ( 'NONE',  ( 2.605696033269626177, 17.55816537872232530, 12.00000000000000000 ) ) ;
#12958 = DIRECTION ( 'NONE',  ( 0.000000000000000000, 0.000000000000000000, 1.000000000000000000 ) ) ;
#12959 = CARTESIAN_POINT ( 'NONE',  ( 10.54700836463452518, 22.39697303105787540, 10.50000000000000533 ) ) ;
#12960 = CARTESIAN_POINT ( 'NONE',  ( 11.54666566735224364, 32.07468077621332725, 7.499999999999997335 ) ) ;
#12961 = CARTESIAN_POINT ( 'NONE',  ( 13.01198037208728842, 31.38676150821800803, -7.241395499289373205 ) ) ;
#12962 = EDGE_LOOP ( 'NONE', ( #7412, #10545, #18337, #21991 ) ) ;
#12963 = CARTESIAN_POINT ( 'NONE',  ( -19.72377957101126711, 11.77771347321402651, -15.94900687590660660 ) ) ;
#12964 = CARTESIAN_POINT ( 'NONE',  ( -10.37659644360395106, 39.73422260060542754, 11.00000000000000000 ) ) ;
#12965 = EDGE_CURVE ( 'NONE', #11714, #21064, #27589, .T. ) ;
#12966 = CARTESIAN_POINT ( 'NONE',  ( 15.04210785476277934, -26.00471334787457067, -9.235286766544799519 ) ) ;
#12967 = PLANE ( 'NONE',  #39244 ) ;
#12968 = CARTESIAN_POINT ( 'NONE',  ( 11.07830671788882881, 17.64536026459691342, -26.82601358146755999 ) ) ;
#12969 = CARTESIAN_POINT ( 'NONE',  ( 37.49625565938770677, -14.69322820095493221, -4.999999999999991118 ) ) ;
#12970 = CARTESIAN_POINT ( 'NONE',  ( 10.36702044712426840, 31.16169077310587809, 9.500000000000000000 ) ) ;
#12971 = VECTOR ( 'NONE', #1636, 1000.000000000000114 ) ;
#12972 = CARTESIAN_POINT ( 'NONE',  ( -26.86432650658507271, -25.19322975956973920, -6.728586538145628460 ) ) ;
#12973 = CARTESIAN_POINT ( 'NONE',  ( 8.383450201187182316, -25.09682772003503359, -7.878769048704421074 ) ) ;
#12974 = CARTESIAN_POINT ( 'NONE',  ( 15.16724506842761500, 25.92448480984241144, -8.769736773116987294 ) ) ;
#12975 = CARTESIAN_POINT ( 'NONE',  ( 27.61701753510086021, -18.71320982384436959, -12.89761149929025663 ) ) ;
#12976 = CARTESIAN_POINT ( 'NONE',  ( 13.95827473762443027, 27.56104949980340280, 10.87262190629280845 ) ) ;
#12977 = DIRECTION ( 'NONE',  ( -0.9781476007338072431, -0.2079116908177516265, 0.000000000000000000 ) ) ;
#12978 = ORIENTED_EDGE ( 'NONE', *, *, #36204, .F. ) ;
#12979 = VECTOR ( 'NONE', #22638, 1000.000000000000000 ) ;
#12980 = CARTESIAN_POINT ( 'NONE',  ( -8.453943144716905778, 36.13191751627968529, -5.441173800798977389 ) ) ;
#12981 = CARTESIAN_POINT ( 'NONE',  ( -7.790810073469786268, 10.07556825234761533, 10.49999999999999645 ) ) ;
#12982 = CARTESIAN_POINT ( 'NONE',  ( 10.47804177580207607, 33.28010392086025604, 7.000000000000000000 ) ) ;
#12983 = EDGE_LOOP ( 'NONE', ( #25627, #24043, #34494, #27307 ) ) ;
#12984 = CARTESIAN_POINT ( 'NONE',  ( 23.95345493350577826, 0.4562929689794089083, -19.49228041339053519 ) ) ;
#12985 = CARTESIAN_POINT ( 'NONE',  ( 13.26584437371809777, 27.13525491562438319, 6.000000000000000000 ) ) ;
#12986 = EDGE_CURVE ( 'NONE', #16736, #1570, #18703, .T. ) ;
#12987 = DIRECTION ( 'NONE',  ( -1.000000000000000000, 0.000000000000000000, 0.000000000000000000 ) ) ;
#12988 = VERTEX_POINT ( 'NONE', #39975 ) ;
#12989 = CARTESIAN_POINT ( 'NONE',  ( -30.75477483822581348, 0.007422296481196848095, -6.417047845488035307 ) ) ;
#12990 = CARTESIAN_POINT ( 'NONE',  ( 9.151574469205250750, 1.945227203041362207, 7.000000000000000000 ) ) ;
#12991 = ORIENTED_EDGE ( 'NONE', *, *, #30031, .F. ) ;
#12992 = CARTESIAN_POINT ( 'NONE',  ( 23.50924913396118399, -4.123401132657353862, -21.07160444102285268 ) ) ;
#12993 = CIRCLE ( 'NONE', #34493, 0.5000000000000004441 ) ;
#12994 = EDGE_CURVE ( 'NONE', #5398, #11410, #12153, .T. ) ;
#12995 = ORIENTED_EDGE ( 'NONE', *, *, #23533, .T. ) ;
#12996 = CARTESIAN_POINT ( 'NONE',  ( -9.340438144419737299, 38.00965938231843211, 10.99999999999993605 ) ) ;
#12997 = EDGE_CURVE ( 'NONE', #24869, #39423, #17010, .T. ) ;
#12998 = CARTESIAN_POINT ( 'NONE',  ( -4.591666147298613332, 15.32946292166675306, 9.000000000000001776 ) ) ;
#12999 = CARTESIAN_POINT ( 'NONE',  ( 11.16520467992603294, 20.33931832809677331, 13.00000000000000178 ) ) ;
#13000 = CARTESIAN_POINT ( 'NONE',  ( 1.410291641398409679, 35.53022820328503428, 18.87996532025784546 ) ) ;
#13001 = FACE_OUTER_BOUND ( 'NONE', #2102, .T. ) ;
#13002 = ORIENTED_EDGE ( 'NONE', *, *, #15926, .F. ) ;
#13003 = DIRECTION ( 'NONE',  ( 1.000000000000000000, 0.000000000000000000, 0.000000000000000000 ) ) ;
#13004 = CARTESIAN_POINT ( 'NONE',  ( -19.88226695332659588, 5.007750446913723508, -30.00000000000000000 ) ) ;
#13005 = DIRECTION ( 'NONE',  ( 1.000000000000000000, 0.000000000000000000, 0.000000000000000000 ) ) ;
#13006 = TOROIDAL_SURFACE ( 'NONE', #38975, 1.000000000000000000, 0.5000000000000000000 ) ;
#13007 = FACE_OUTER_BOUND ( 'NONE', #17499, .T. ) ;
#13008 = CARTESIAN_POINT ( 'NONE',  ( 14.33908007195274692, 14.82388666928050647, -27.64946332230921655 ) ) ;
#13009 = CARTESIAN_POINT ( 'NONE',  ( 8.982065559873033678, 34.94785179831643518, -8.031862189828427034 ) ) ;
#13010 = VERTEX_POINT ( 'NONE', #15998 ) ;
#13011 = EDGE_CURVE ( 'NONE', #26241, #33406, #25332, .T. ) ;
#13012 = ADVANCED_FACE ( 'NONE', ( #13543 ), #22881, .T. ) ;
#13013 = CARTESIAN_POINT ( 'NONE',  ( 11.89829529493479221, -20.33063158364313239, -20.44835590138199066 ) ) ;
#13014 = DIRECTION ( 'NONE',  ( -0.9781476007338069101, -0.2079116908177533751, 0.000000000000000000 ) ) ;
#13015 = LINE ( 'NONE', #31510, #34901 ) ;
#13016 = VERTEX_POINT ( 'NONE', #19638 ) ;
#13017 = CARTESIAN_POINT ( 'NONE',  ( -11.90856329309679218, 19.36478525622990787, -21.61991777980233920 ) ) ;
#13018 = CARTESIAN_POINT ( 'NONE',  ( -20.56996978659371678, -26.19496882840758545, 17.42190598798392998 ) ) ;
#13019 = CARTESIAN_POINT ( 'NONE',  ( 13.25977140536878807, -23.61272118971784906, -14.48244016720286176 ) ) ;
#13020 = DIRECTION ( 'NONE',  ( -0.000000000000000000, -0.000000000000000000, -1.000000000000000000 ) ) ;
#13021 = ORIENTED_EDGE ( 'NONE', *, *, #23913, .F. ) ;
#13022 = EDGE_LOOP ( 'NONE', ( #18172, #12714, #14702, #34423 ) ) ;
#13023 = CARTESIAN_POINT ( 'NONE',  ( -8.851921390983532589, 18.49121495627866452, -29.99999999999998579 ) ) ;
#13024 = PLANE ( 'NONE',  #23035 ) ;
#13025 = FACE_BOUND ( 'NONE', #16401, .T. ) ;
#13026 = CARTESIAN_POINT ( 'NONE',  ( -32.71123478963491493, -10.14810845015363050, -11.13421304303691350 ) ) ;
#13027 = CARTESIAN_POINT ( 'NONE',  ( -9.881661346875441509, -18.84796558037550795, -25.02421141044853670 ) ) ;
#13028 = CARTESIAN_POINT ( 'NONE',  ( 11.11016527260166953, 31.83082137946472656, 11.00000000000000000 ) ) ;
#13029 = VERTEX_POINT ( 'NONE', #13338 ) ;
#13030 = CARTESIAN_POINT ( 'NONE',  ( 30.21135594116120160, 0.1457432374558486343, -8.299147896465123964 ) ) ;
#13031 = DIRECTION ( 'NONE',  ( 0.000000000000000000, 0.000000000000000000, 1.000000000000000000 ) ) ;
#13032 = CARTESIAN_POINT ( 'NONE',  ( 7.766013557953380442, 28.81973365084987293, 10.49999999999999467 ) ) ;
#13033 = VECTOR ( 'NONE', #7667, 1000.000000000000000 ) ;
#13034 = ORIENTED_EDGE ( 'NONE', *, *, #33614, .F. ) ;
#13035 = CARTESIAN_POINT ( 'NONE',  ( -27.18275240598519815, 0.1768051309694248507, -14.47033692342836098 ) ) ;
#13036 = EDGE_CURVE ( 'NONE', #34540, #19729, #9619, .T. ) ;
#13037 = ORIENTED_EDGE ( 'NONE', *, *, #26727, .T. ) ;
#13038 = CARTESIAN_POINT ( 'NONE',  ( 26.73663087904732905, -1.280630175484808397, -16.25687896506618557 ) ) ;
#13039 = DIRECTION ( 'NONE',  ( 0.000000000000000000, 0.000000000000000000, 1.000000000000000000 ) ) ;
#13040 = CARTESIAN_POINT ( 'NONE',  ( 34.20211996652216868, -5.988425181405260034, 16.87380292611403121 ) ) ;
#13041 = VERTEX_POINT ( 'NONE', #9900 ) ;
#13042 = LINE ( 'NONE', #37831, #1372 ) ;
#13043 = CARTESIAN_POINT ( 'NONE',  ( -2.442402655125509359, 27.78651631404546052, 20.99999999999999645 ) ) ;
#13044 = AXIS2_PLACEMENT_3D ( 'NONE', #29098, #8371, #30310 ) ;
#13045 = CYLINDRICAL_SURFACE ( 'NONE', #7708, 16.99999999999999645 ) ;
#13046 = VECTOR ( 'NONE', #23604, 1000.000000000000000 ) ;
#13047 = PLANE ( 'NONE',  #24054 ) ;
#13048 = FACE_BOUND ( 'NONE', #30721, .T. ) ;
#13049 = CARTESIAN_POINT ( 'NONE',  ( -4.794796183862964689, 36.71301971979259804, 7.000000000000000000 ) ) ;
#13050 = CARTESIAN_POINT ( 'NONE',  ( -21.63082554306499716, 8.459712576583205745, -15.90695635898583404 ) ) ;
#13051 = CARTESIAN_POINT ( 'NONE',  ( 17.08717224709219451, -21.22693275917435329, -16.97485990036564729 ) ) ;
#13052 = LINE ( 'NONE', #10419, #20922 ) ;
#13053 = ADVANCED_FACE ( 'NONE', ( #22089 ), #10252, .T. ) ;
#13054 = CARTESIAN_POINT ( 'NONE',  ( 10.86351183210297400, 17.43903252575687546, -28.70101831061248987 ) ) ;
#13055 = VERTEX_POINT ( 'NONE', #6835 ) ;
#13056 = CARTESIAN_POINT ( 'NONE',  ( -12.17604136976394358, 17.00510967891084135, -26.32489337626220660 ) ) ;
#13057 = CARTESIAN_POINT ( 'NONE',  ( -19.13252718791541440, -21.21924719729587139, 20.25080042701590699 ) ) ;
#13058 = CARTESIAN_POINT ( 'NONE',  ( 10.47540670418223208, 32.60491492691330961, 10.99999999999999645 ) ) ;
#13059 = CARTESIAN_POINT ( 'NONE',  ( 14.95773614117678996, 25.72884227512856370, -9.710064219024593157 ) ) ;
#13060 = ORIENTED_EDGE ( 'NONE', *, *, #12811, .F. ) ;
#13061 = CARTESIAN_POINT ( 'NONE',  ( 19.59609834480663082, -10.05714783815784052, -24.22289641939408256 ) ) ;
#13062 = LINE ( 'NONE', #31558, #20326 ) ;
#13063 = ORIENTED_EDGE ( 'NONE', *, *, #25974, .F. ) ;
#13065 = CARTESIAN_POINT ( 'NONE',  ( 8.315274455032101386, 10.01576150750513250, 7.500000000000000888 ) ) ;
#13064 = CARTESIAN_POINT ( 'NONE',  ( -11.03568212627763678, 17.86295559657867216, -26.20877666994450550 ) ) ;
#13066 = CARTESIAN_POINT ( 'NONE',  ( -14.04776079454142490, -23.13890183802322653, -15.34726994745094686 ) ) ;
#13067 = CARTESIAN_POINT ( 'NONE',  ( 12.48446084878463225, 14.34248059624565563, 10.49999999999999822 ) ) ;
#13068 = VECTOR ( 'NONE', #4671, 1000.000000000000000 ) ;
#13069 = ORIENTED_EDGE ( 'NONE', *, *, #29468, .F. ) ;
#13070 = CARTESIAN_POINT ( 'NONE',  ( -33.15023676467436786, -14.84419029601833806, -9.736194267565831950 ) ) ;
#13071 = CARTESIAN_POINT ( 'NONE',  ( -11.58176784450557761, -22.04669522693308181, -17.49831374786357330 ) ) ;
#13072 = DIRECTION ( 'NONE',  ( 1.000000000000000000, 0.000000000000000000, 0.000000000000000000 ) ) ;
#13073 = CARTESIAN_POINT ( 'NONE',  ( 16.22052397401369461, 22.81938114578490584, -8.804735524812913994 ) ) ;
#13074 = ORIENTED_EDGE ( 'NONE', *, *, #2328, .T. ) ;
#13075 = CARTESIAN_POINT ( 'NONE',  ( 26.70883441844552664, 4.675912117059606743, -5.000000000000001776 ) ) ;
#13076 = AXIS2_PLACEMENT_3D ( 'NONE', #37343, #567, #168 ) ;
#13077 = DIRECTION ( 'NONE',  ( 0.000000000000000000, 0.000000000000000000, 1.000000000000000000 ) ) ;
#13078 = DIRECTION ( 'NONE',  ( 0.000000000000000000, 0.000000000000000000, 1.000000000000000000 ) ) ;
#13079 = CARTESIAN_POINT ( 'NONE',  ( -10.17939521785135071, 33.00296324411767301, 10.49999999999999822 ) ) ;
#13080 = ORIENTED_EDGE ( 'NONE', *, *, #21156, .T. ) ;
#13081 = CARTESIAN_POINT ( 'NONE',  ( -21.03058350190238457, 0.1347426989242972717, -26.16529232141537875 ) ) ;
#13082 = EDGE_CURVE ( 'NONE', #36614, #32296, #15054, .T. ) ;
#13083 = CARTESIAN_POINT ( 'NONE',  ( 30.22740896235442776, -0.2270326147911990722, -9.222382858374048809 ) ) ;
#13084 = EDGE_CURVE ( 'NONE', #2909, #1082, #34488, .T. ) ;
#13085 = CARTESIAN_POINT ( 'NONE',  ( 27.94267071599651686, -5.959630984681780319, 20.25080042701592831 ) ) ;
#13086 = ORIENTED_EDGE ( 'NONE', *, *, #30958, .F. ) ;
#13087 = CARTESIAN_POINT ( 'NONE',  ( -13.28992586503615847, -18.25382200079944539, -30.00000000000000711 ) ) ;
#13088 = DIRECTION ( 'NONE',  ( 1.000000000000000000, 0.000000000000000000, 0.000000000000000000 ) ) ;
#13089 = ADVANCED_FACE ( 'NONE', ( #25931 ), #38330, .T. ) ;
#13090 = EDGE_LOOP ( 'NONE', ( #26795, #16644, #36132, #23744, #29365 ) ) ;
#13091 = FACE_OUTER_BOUND ( 'NONE', #18936, .T. ) ;
#13092 = CARTESIAN_POINT ( 'NONE',  ( -10.44103466624267362, 32.57396620494225914, 11.00000000000000000 ) ) ;
#13093 = DIRECTION ( 'NONE',  ( -0.9135454576426059736, -0.4067366430757889395, 0.000000000000000000 ) ) ;
#13094 = CARTESIAN_POINT ( 'NONE',  ( 3.503322964093031455, 26.44893706114941523, -18.65895197296932650 ) ) ;
#13095 = DIRECTION ( 'NONE',  ( 1.000000000000000000, 0.000000000000000000, -0.000000000000000000 ) ) ;
#13096 = ORIENTED_EDGE ( 'NONE', *, *, #12500, .T. ) ;
#13097 = CARTESIAN_POINT ( 'NONE',  ( 8.910254037844367758, 17.93301270189219210, 10.00000000000000000 ) ) ;
#13098 = CARTESIAN_POINT ( 'NONE',  ( 1.439880186556678821, -2.006054360071897857, 9.500000000000000000 ) ) ;
#13099 = CARTESIAN_POINT ( 'NONE',  ( 28.63180867286471809, -22.06108345148580696, -9.744445364747779337 ) ) ;
#13100 = EDGE_CURVE ( 'NONE', #37186, #7787, #32331, .T. ) ;
#13101 = ADVANCED_FACE ( 'NONE', ( #31631, #3799 ), #10100, .T. ) ;
#13102 = CARTESIAN_POINT ( 'NONE',  ( -14.23945615837876311, -31.58416516429889853, 3.000000000000000000 ) ) ;
#13103 = CARTESIAN_POINT ( 'NONE',  ( -12.01838097023000529, 23.73363068877903359, 12.00000000000000000 ) ) ;
#13104 = CARTESIAN_POINT ( 'NONE',  ( -7.312041872459064784, 25.58773265502866678, 6.000000000000000000 ) ) ;
#13105 = ADVANCED_FACE ( 'NONE', ( #28787 ), #7238, .F. ) ;
#13106 = CARTESIAN_POINT ( 'NONE',  ( 14.93523343043905882, 27.03121972480990820, -8.269414059510982185 ) ) ;
#13107 = FACE_OUTER_BOUND ( 'NONE', #39902, .T. ) ;
#13108 = EDGE_LOOP ( 'NONE', ( #13520, #20429, #2899, #31364 ) ) ;
#13110 = DIRECTION ( 'NONE',  ( -0.000000000000000000, -0.000000000000000000, -1.000000000000000000 ) ) ;
#13109 = CARTESIAN_POINT ( 'NONE',  ( -16.11915739853855811, 18.74155883991118898, -14.73719238174496127 ) ) ;
#13111 = DIRECTION ( 'NONE',  ( 0.000000000000000000, 0.000000000000000000, 1.000000000000000000 ) ) ;
#13112 = AXIS2_PLACEMENT_3D ( 'NONE', #31731, #19536, #16293 ) ;
#13113 = CARTESIAN_POINT ( 'NONE',  ( 9.950384810341901698, -18.82026468017858889, -25.01640556310974972 ) ) ;
#13114 = CARTESIAN_POINT ( 'NONE',  ( -7.929471891321301591, 25.60217271033470610, 9.000000000000001776 ) ) ;
#13115 = CARTESIAN_POINT ( 'NONE',  ( 15.37331383236014126, 26.66785149480303119, -6.417008027727837849 ) ) ;
#13116 = VERTEX_POINT ( 'NONE', #38126 ) ;
#13117 = CARTESIAN_POINT ( 'NONE',  ( 14.73499465698446009, 25.40345112443975495, -10.65306111367642927 ) ) ;
#13118 = ORIENTED_EDGE ( 'NONE', *, *, #30794, .T. ) ;
#13119 = CARTESIAN_POINT ( 'NONE',  ( 14.42035624161478857, 26.65972665747660031, 10.49999999999999822 ) ) ;
#13120 = CARTESIAN_POINT ( 'NONE',  ( -15.08926872483068315, -26.26244385881013699, -8.298346565395871011 ) ) ;
#13121 = CARTESIAN_POINT ( 'NONE',  ( -36.76835206499502107, -7.129807841006686964, 13.32518128616540665 ) ) ;
#13122 = CARTESIAN_POINT ( 'NONE',  ( -16.73268231713828058, -12.27567335498239842, -27.72086002018244599 ) ) ;
#13123 = CARTESIAN_POINT ( 'NONE',  ( -4.261170676688491810, -23.24522659430452265, -14.87884297781055842 ) ) ;
#13124 = CARTESIAN_POINT ( 'NONE',  ( 13.01467249004550020, 20.52916449794418696, -18.51329633673889674 ) ) ;
#13125 = ORIENTED_EDGE ( 'NONE', *, *, #31466, .F. ) ;
#13126 = CARTESIAN_POINT ( 'NONE',  ( 22.62620251215892253, 10.10101068805073865, -7.914309724494427378 ) ) ;
#13127 = DIRECTION ( 'NONE',  ( -0.000000000000000000, -0.000000000000000000, -1.000000000000000000 ) ) ;
#13128 = CARTESIAN_POINT ( 'NONE',  ( -9.066401385854234718, 34.43014579340745485, 17.42190598798393353 ) ) ;
#13129 = VERTEX_POINT ( 'NONE', #10300 ) ;
#13130 = CARTESIAN_POINT ( 'NONE',  ( -33.78064619886176700, -4.467697089185144854, -6.796441298519896534 ) ) ;
#13131 = EDGE_CURVE ( 'NONE', #20339, #37305, #16604, .T. ) ;
#13132 = CARTESIAN_POINT ( 'NONE',  ( -23.22986302875264641, 7.287013008511430634, 17.42190598798427459 ) ) ;
#13133 = CIRCLE ( 'NONE', #17042, 0.5000000000000004441 ) ;
#13134 = EDGE_LOOP ( 'NONE', ( #32941, #831, #30296, #28742 ) ) ;
#13135 = ADVANCED_FACE ( 'NONE', ( #28984 ), #1162, .T. ) ;
#13136 = CYLINDRICAL_SURFACE ( 'NONE', #19276, 18.00000000000000000 ) ;
#13137 = DIRECTION ( 'NONE',  ( 0.9945218953682730678, -0.1045284632676569819, 0.000000000000000000 ) ) ;
#13138 = AXIS2_PLACEMENT_3D ( 'NONE', #12106, #11711, #21055 ) ;
#13139 = CARTESIAN_POINT ( 'NONE',  ( 32.85715722811898587, -14.37096278579205411, -10.18737089092998538 ) ) ;
#13140 = AXIS2_PLACEMENT_3D ( 'NONE', #19400, #19603, #1124 ) ;
#13141 = CARTESIAN_POINT ( 'NONE',  ( 22.71959475104719317, -29.00055231699513669, 12.14047268033058025 ) ) ;
#13142 = VERTEX_POINT ( 'NONE', #32855 ) ;
#13143 = AXIS2_PLACEMENT_3D ( 'NONE', #3055, #33754, #12198 ) ;
#13144 = ORIENTED_EDGE ( 'NONE', *, *, #1376, .T. ) ;
#13145 = CARTESIAN_POINT ( 'NONE',  ( -34.47241746879593904, 3.460351812918829761, 0.000000000000000000 ) ) ;
#13146 = DIRECTION ( 'NONE',  ( 0.000000000000000000, 0.000000000000000000, 1.000000000000000000 ) ) ;
#13147 = CIRCLE ( 'NONE', #12495, 1.000000000000000888 ) ;
#13148 = DIRECTION ( 'NONE',  ( 0.000000000000000000, 0.000000000000000000, 1.000000000000000000 ) ) ;
#13149 = ORIENTED_EDGE ( 'NONE', *, *, #35765, .T. ) ;
#13150 = CARTESIAN_POINT ( 'NONE',  ( -1.226217677998840516, 24.65685218365392828, -20.69626040025250902 ) ) ;
#13151 = CARTESIAN_POINT ( 'NONE',  ( -14.03791758423776592, 27.78611923485716773, 7.485699520496972070 ) ) ;
#13152 = CARTESIAN_POINT ( 'NONE',  ( -14.94482798346716557, 26.50521816028930999, 7.000000000000000000 ) ) ;
#13153 = DIRECTION ( 'NONE',  ( 0.000000000000000000, 0.000000000000000000, 1.000000000000000000 ) ) ;
#13154 = CARTESIAN_POINT ( 'NONE',  ( 1.265502442671760264, 36.24516302788250499, 6.000000000000000000 ) ) ;
#13155 = DIRECTION ( 'NONE',  ( 0.9781476007338042455, -0.2079116908177663647, 0.000000000000000000 ) ) ;
#13156 = CARTESIAN_POINT ( 'NONE',  ( 10.61980620388852969, 20.62470325590637898, -21.39191359161199202 ) ) ;
#13157 = DIRECTION ( 'NONE',  ( 1.000000000000000000, 0.000000000000000000, 0.000000000000000000 ) ) ;
#13158 = ORIENTED_EDGE ( 'NONE', *, *, #9815, .T. ) ;
#13160 = DIRECTION ( 'NONE',  ( 0.000000000000000000, 0.000000000000000000, 1.000000000000000000 ) ) ;
#13159 = CARTESIAN_POINT ( 'NONE',  ( -18.06822122341611347, 9.865462442820332356, -27.73584775015774539 ) ) ;
#13161 = DIRECTION ( 'NONE',  ( 0.000000000000000000, 0.000000000000000000, 1.000000000000000000 ) ) ;
#13162 = CARTESIAN_POINT ( 'NONE',  ( 15.51572609547548254, -26.72387080533473380, -5.945569791504813573 ) ) ;
#13163 = LINE ( 'NONE', #16227, #37970 ) ;
#13164 = EDGE_CURVE ( 'NONE', #32632, #21064, #13948, .T. ) ;
#13165 = CARTESIAN_POINT ( 'NONE',  ( 13.73891004957165940, 23.46505885318682516, -14.46902604110928969 ) ) ;
#13166 = CARTESIAN_POINT ( 'NONE',  ( -16.84920187454419960, 29.09530251867925443, -13.79123840944734170 ) ) ;
#13167 = CARTESIAN_POINT ( 'NONE',  ( 4.440829913680675034, 10.60893893836775348, 6.000000000000000000 ) ) ;
#13168 = CARTESIAN_POINT ( 'NONE',  ( -25.11387969369502215, -25.04874519970718083, -8.917861276085261579 ) ) ;
#13169 = CARTESIAN_POINT ( 'NONE',  ( 7.004305706416510624, -19.31551653162770776, -30.00000000000000000 ) ) ;
#13170 = CARTESIAN_POINT ( 'NONE',  ( 15.49934645862682103, 26.48612375915841710, -4.999999999999998224 ) ) ;
#13171 = CARTESIAN_POINT ( 'NONE',  ( 16.84105033895882642, -12.12787018219099089, -27.71828030521067632 ) ) ;
#13172 = AXIS2_PLACEMENT_3D ( 'NONE', #12280, #34611, #30581 ) ;
#13173 = CARTESIAN_POINT ( 'NONE',  ( 14.08493436138100030, 27.60220370627940767, 10.68306085400108074 ) ) ;
#13174 = PLANE ( 'NONE',  #36490 ) ;
#13175 = ORIENTED_EDGE ( 'NONE', *, *, #27650, .T. ) ;
#13176 = CARTESIAN_POINT ( 'NONE',  ( -8.269738542359823086, 35.15571153379752900, -8.458646650837764014 ) ) ;
#13177 = AXIS2_PLACEMENT_3D ( 'NONE', #2030, #32299, #20111 ) ;
#13178 = DIRECTION ( 'NONE',  ( 0.000000000000000000, 0.000000000000000000, 1.000000000000000000 ) ) ;
#13179 = ORIENTED_EDGE ( 'NONE', *, *, #22198, .T. ) ;
#13180 = CARTESIAN_POINT ( 'NONE',  ( 29.37565202589770763, 0.04982724068811738433, -10.65280254111669045 ) ) ;
#13181 = CARTESIAN_POINT ( 'NONE',  ( -2.036571916123809167, 8.108948098542077432, 9.500000000000000000 ) ) ;
#13182 = CARTESIAN_POINT ( 'NONE',  ( -27.14644468510207886, -3.730463242937111179, 19.99202127657103745 ) ) ;
#13183 = ORIENTED_EDGE ( 'NONE', *, *, #4049, .F. ) ;
#13184 = CARTESIAN_POINT ( 'NONE',  ( -21.27098901970252598, 0.8144016237283049353, -25.01870527535232469 ) ) ;
#13185 = CARTESIAN_POINT ( 'NONE',  ( -20.14086772481481447, -26.69671823294502744, -8.145045411856523643 ) ) ;
#13186 = VECTOR ( 'NONE', #24857, 1000.000000000000000 ) ;
#13187 = VERTEX_POINT ( 'NONE', #23091 ) ;
#13188 = CARTESIAN_POINT ( 'NONE',  ( 35.24432775889728475, -8.480040233932975013, -5.445055975222005351 ) ) ;
#13189 = VECTOR ( 'NONE', #11323, 1000.000000000000227 ) ;
#13190 = ORIENTED_EDGE ( 'NONE', *, *, #29239, .T. ) ;
#13191 = PRODUCT_CONTEXT ( 'NONE', #15056, 'mechanical' ) ;
#13192 = CARTESIAN_POINT ( 'NONE',  ( 13.80292604922466460, 34.21633694312856733, 11.55979286843946774 ) ) ;
#13193 = CARTESIAN_POINT ( 'NONE',  ( 6.651296319737277862, 27.81603774131160023, 9.000000000000001776 ) ) ;
#13194 = CARTESIAN_POINT ( 'NONE',  ( -0.9674447320696243358, 37.46890771325332281, 7.339470489435490741 ) ) ;
#13195 = CARTESIAN_POINT ( 'NONE',  ( 9.006936242053848574, 32.02107499576887761, 18.87996532025784546 ) ) ;
#13196 = CIRCLE ( 'NONE', #35924, 1.000000000000000888 ) ;
#13197 = FACE_OUTER_BOUND ( 'NONE', #28361, .T. ) ;
#13198 = EDGE_LOOP ( 'NONE', ( #5692, #8899, #13403, #21303 ) ) ;
#13199 = PRESENTATION_STYLE_ASSIGNMENT (( #14010 ) ) ;
#13200 = CARTESIAN_POINT ( 'NONE',  ( 8.088808017670798378, 18.84043440346156473, -29.99999999999999645 ) ) ;
#13201 = CARTESIAN_POINT ( 'NONE',  ( 19.26948696230199687, 27.85601271560034675, 11.00000000000000000 ) ) ;
#13202 = PLANE ( 'NONE',  #32519 ) ;
#13203 = CARTESIAN_POINT ( 'NONE',  ( 17.30437301942612294, 17.82039300084830202, -12.79526519019998432 ) ) ;
#13204 = CARTESIAN_POINT ( 'NONE',  ( 7.825189179823995644, 30.28281593568562258, -13.92036688199892680 ) ) ;
#13205 = AXIS2_PLACEMENT_3D ( 'NONE', #7294, #29644, #14207 ) ;
#13206 = ORIENTED_EDGE ( 'NONE', *, *, #22684, .F. ) ;
#13207 = EDGE_CURVE ( 'NONE', #28046, #4170, #17624, .T. ) ;
#13208 = CARTESIAN_POINT ( 'NONE',  ( 12.48152888332789878, -21.43928621844884574, -18.38220065339488940 ) ) ;
#13209 = DIRECTION ( 'NONE',  ( 0.7771459614569745655, 0.6293203910498328391, 0.000000000000000000 ) ) ;
#13210 = FACE_OUTER_BOUND ( 'NONE', #7779, .T. ) ;
#13211 = ORIENTED_EDGE ( 'NONE', *, *, #969, .F. ) ;
#13212 = CARTESIAN_POINT ( 'NONE',  ( -15.36719073388214341, 26.68956433499065994, -6.416937597740959731 ) ) ;
#13213 = AXIS2_PLACEMENT_3D ( 'NONE', #1521, #14108, #38697 ) ;
#13214 = CARTESIAN_POINT ( 'NONE',  ( -20.61005271883044543, -26.74738414229389249, 16.87380292611441490 ) ) ;
#13215 = CARTESIAN_POINT ( 'NONE',  ( 11.84140825053389001, -22.03755937975082446, -17.47623322197002338 ) ) ;
#13216 = ADVANCED_FACE ( 'NONE', ( #8462 ), #33062, .F. ) ;
#13217 = FACE_OUTER_BOUND ( 'NONE', #33564, .T. ) ;
#13218 = EDGE_CURVE ( 'NONE', #38584, #40188, #18068, .T. ) ;
#13219 = VERTEX_POINT ( 'NONE', #29994 ) ;
#13220 = ORIENTED_EDGE ( 'NONE', *, *, #8221, .F. ) ;
#13221 = CARTESIAN_POINT ( 'NONE',  ( -9.391599613247716860, 21.62240220123701917, -21.21144781721583072 ) ) ;
#13222 = CARTESIAN_POINT ( 'NONE',  ( -10.44103466624267185, 32.57396620494226624, 9.000000000000001776 ) ) ;
#13223 = FACE_BOUND ( 'NONE', #21301, .T. ) ;
#13224 = VECTOR ( 'NONE', #3371, 999.9999999999998863 ) ;
#13225 = CARTESIAN_POINT ( 'NONE',  ( -20.24777750044549762, -4.334933572263888202, -27.83540287325038776 ) ) ;
#13226 = DIRECTION ( 'NONE',  ( 1.000000000000000000, 0.000000000000000000, 0.000000000000000000 ) ) ;
#13227 = EDGE_LOOP ( 'NONE', ( #14845, #35933, #7243, #38899 ) ) ;
#13228 = CARTESIAN_POINT ( 'NONE',  ( 30.72030077726637032, 0.1104180286406396816, -5.946111898128993545 ) ) ;
#13229 = CARTESIAN_POINT ( 'NONE',  ( 10.98647152928294446, 17.30743895948372213, -29.99999999999999289 ) ) ;
#13230 = CARTESIAN_POINT ( 'NONE',  ( -12.33616729053609795, -27.99489201236593061, -4.999999999999999112 ) ) ;
#13231 = CARTESIAN_POINT ( 'NONE',  ( 14.64659974985904967, 21.96608861361208298, 10.49999999999999645 ) ) ;
#13232 = EDGE_LOOP ( 'NONE', ( #29492, #20880 ) ) ;
#13233 = CARTESIAN_POINT ( 'NONE',  ( -27.74642324427214390, 0.1782721915882912456, -13.51284498012490509 ) ) ;
#13234 = CARTESIAN_POINT ( 'NONE',  ( -36.77472485986697137, -21.41827268707265830, 10.99999999999999645 ) ) ;
#13235 = ORIENTED_EDGE ( 'NONE', *, *, #21061, .T. ) ;
#13236 = CARTESIAN_POINT ( 'NONE',  ( 27.66764765329071807, -1.745514196759363035, -15.23339469188658235 ) ) ;
#13237 = AXIS2_PLACEMENT_3D ( 'NONE', #18807, #31195, #9466 ) ;
#13238 = CARTESIAN_POINT ( 'NONE',  ( 11.56212933365550377, 16.94202105496415456, -30.00000000000001421 ) ) ;
#13239 = CARTESIAN_POINT ( 'NONE',  ( 33.13500937546621117, -2.712167277691212242, 16.30093088680227709 ) ) ;
#13240 = EDGE_CURVE ( 'NONE', #5911, #9357, #2170, .T. ) ;
#13241 = ORIENTED_EDGE ( 'NONE', *, *, #2346, .T. ) ;
#13242 = CARTESIAN_POINT ( 'NONE',  ( 8.305703523983371639, 36.29191545080498571, 16.30093088680192537 ) ) ;
#13243 = ADVANCED_FACE ( 'NONE', ( #14555 ), #36886, .T. ) ;
#13244 = DIRECTION ( 'NONE',  ( -0.000000000000000000, -0.000000000000000000, -1.000000000000000000 ) ) ;
#13245 = CARTESIAN_POINT ( 'NONE',  ( -4.439344921102643227, 26.26892614308282603, 20.99999999999999645 ) ) ;
#13246 = VECTOR ( 'NONE', #23810, 1000.000000000000000 ) ;
#13247 = CARTESIAN_POINT ( 'NONE',  ( 12.30736835487432579, 14.81698729810772619, 7.499999999999997335 ) ) ;
#13248 = LINE ( 'NONE', #6944, #18858 ) ;
#13249 = PRODUCT ( 'Protective Beveled Outer Blade Guard', 'Protective Beveled Outer Blade Guard', '', ( #1017 ) ) ;
#13250 = CONICAL_SURFACE ( 'NONE', #32765, 0.5000000000000002220, 0.7853981633974514986 ) ;
#13251 = FACE_BOUND ( 'NONE', #12546, .T. ) ;
#13252 = CARTESIAN_POINT ( 'NONE',  ( 17.92566989745171568, 16.47414500506706503, 17.42190598798409695 ) ) ;
#13253 = CARTESIAN_POINT ( 'NONE',  ( -23.53973944703488286, 8.948669315374337074, -6.448443132398569588 ) ) ;
#13254 = CARTESIAN_POINT ( 'NONE',  ( 19.67723955058091789, -23.00962397103849000, -14.03145724330032529 ) ) ;
#13255 = CARTESIAN_POINT ( 'NONE',  ( -13.19674782540811186, 16.00858767546144534, 10.49999999999999467 ) ) ;
#13256 = ADVANCED_FACE ( 'NONE', ( #32653 ), #17420, .F. ) ;
#13257 = ORIENTED_EDGE ( 'NONE', *, *, #21062, .F. ) ;
#13258 = CARTESIAN_POINT ( 'NONE',  ( 14.67936663452034907, 25.57073318950553542, -10.64181656390416286 ) ) ;
#13259 = ORIENTED_EDGE ( 'NONE', *, *, #9158, .T. ) ;
#13260 = CARTESIAN_POINT ( 'NONE',  ( -15.03545123130942507, 24.54682575326017968, -10.67232211706494560 ) ) ;
#13261 = CARTESIAN_POINT ( 'NONE',  ( -18.28744585352635355, -19.47582948098888522, 20.69868183039782394 ) ) ;
#13262 = DIRECTION ( 'NONE',  ( 0.000000000000000000, -0.6037757019622788102, -0.7971542521494553446 ) ) ;
#13263 = CARTESIAN_POINT ( 'NONE',  ( 11.50520882153597846, 18.41930897395437938, -23.85713326318693106 ) ) ;
#13264 = ORIENTED_EDGE ( 'NONE', *, *, #571, .F. ) ;
#13265 = CARTESIAN_POINT ( 'NONE',  ( 33.70372332681250782, -18.58847439657466083, -4.999999999999997335 ) ) ;
#13266 = CARTESIAN_POINT ( 'NONE',  ( -10.39021566973307031, 20.90519018800561568, 11.00000000000000000 ) ) ;
#13267 = VERTEX_POINT ( 'NONE', #39131 ) ;
#13269 = DIRECTION ( 'NONE',  ( 1.000000000000000000, 0.000000000000000000, 0.000000000000000000 ) ) ;
#13268 = CARTESIAN_POINT ( 'NONE',  ( -12.18834851601500269, 20.75798833321451653, -19.45407312999939009 ) ) ;
#13270 = CARTESIAN_POINT ( 'NONE',  ( -12.06810631748702178, -20.91201952217128834, -19.43044751594679909 ) ) ;
#13271 = DIRECTION ( 'NONE',  ( 1.000000000000000000, 0.000000000000000000, 0.000000000000000000 ) ) ;
#13272 = VERTEX_POINT ( 'NONE', #29388 ) ;
#13273 = CARTESIAN_POINT ( 'NONE',  ( -18.70070976566389831, -8.421454915599365876, -29.21689156567847334 ) ) ;
#13274 = CARTESIAN_POINT ( 'NONE',  ( -14.25032268057046991, -26.07042913507176962, -8.304725559915748789 ) ) ;
#13275 = FACE_OUTER_BOUND ( 'NONE', #35931, .T. ) ;
#13276 = CARTESIAN_POINT ( 'NONE',  ( 15.94966356142663777, 23.22048705160648652, -9.275927655557403284 ) ) ;
#13277 = ORIENTED_EDGE ( 'NONE', *, *, #11770, .F. ) ;
#13278 = CARTESIAN_POINT ( 'NONE',  ( 26.66957287664490295, 3.773598562717486615, -9.786777780698315610 ) ) ;
#13279 = DIRECTION ( 'NONE',  ( 0.000000000000000000, 0.000000000000000000, 1.000000000000000000 ) ) ;
#13280 = CARTESIAN_POINT ( 'NONE',  ( -21.91981567634960371, -15.65087685632114045, 23.00000000000000000 ) ) ;
#13281 = VERTEX_POINT ( 'NONE', #35892 ) ;
#13282 = CARTESIAN_POINT ( 'NONE',  ( -30.34199328301418674, -0.3569055445810484506, -9.214469955534525525 ) ) ;
#13283 = AXIS2_PLACEMENT_3D ( 'NONE', #29217, #10941, #26975 ) ;
#13284 = CARTESIAN_POINT ( 'NONE',  ( 21.76708849998995277, 0.4128473488999230834, -23.81551767858415047 ) ) ;
#13285 = CARTESIAN_POINT ( 'NONE',  ( 24.31339772227982365, -19.97941014234455537, 20.25080042701539185 ) ) ;
#13286 = ORIENTED_EDGE ( 'NONE', *, *, #7533, .T. ) ;
#13287 = EDGE_CURVE ( 'NONE', #36438, #13219, #14199, .T. ) ;
#13288 = AXIS2_PLACEMENT_3D ( 'NONE', #10268, #28156, #332 ) ;
#13289 = CARTESIAN_POINT ( 'NONE',  ( 15.72991998290128990, -16.18894361744929000, -29.99999999999998579 ) ) ;
#13290 = PLANE ( 'NONE',  #6309 ) ;
#13291 = AXIS2_PLACEMENT_3D ( 'NONE', #31646, #16214, #28597 ) ;
#13292 = ORIENTED_EDGE ( 'NONE', *, *, #21163, .F. ) ;
#13293 = DIRECTION ( 'NONE',  ( 0.000000000000000000, 0.000000000000000000, 1.000000000000000000 ) ) ;
#13294 = CARTESIAN_POINT ( 'NONE',  ( 0.000000000000000000, 37.50000000000000711, 7.000000000000000000 ) ) ;
#13295 = FACE_OUTER_BOUND ( 'NONE', #32891, .T. ) ;
#13296 = LINE ( 'NONE', #29348, #19835 ) ;
#13297 = ORIENTED_EDGE ( 'NONE', *, *, #13544, .F. ) ;
#13298 = CARTESIAN_POINT ( 'NONE',  ( -2.587667106213709101, 35.31811204475769728, 13.00000000000000178 ) ) ;
#13299 = DIRECTION ( 'NONE',  ( -0.000000000000000000, 0.000000000000000000, 1.000000000000000000 ) ) ;
#13300 = CARTESIAN_POINT ( 'NONE',  ( 17.80350308363193079, -15.45044821450308703, -21.94968374958370916 ) ) ;
#13301 = CARTESIAN_POINT ( 'NONE',  ( 10.44103466624280507, 32.57396620494213124, 11.00000000000000000 ) ) ;
#13302 = CARTESIAN_POINT ( 'NONE',  ( 9.771904059883945948, 33.31711103041952526, 7.000000000000000000 ) ) ;
#13303 = EDGE_CURVE ( 'NONE', #8057, #26968, #29795, .T. ) ;
#13304 = VECTOR ( 'NONE', #29871, 1000.000000000000000 ) ;
#13305 = CARTESIAN_POINT ( 'NONE',  ( 14.02888686415674613, 25.13130688616161734, -12.49550152463516284 ) ) ;
#13306 = DIRECTION ( 'NONE',  ( 1.000000000000000000, 0.000000000000000000, 0.000000000000000000 ) ) ;
#13307 = EDGE_LOOP ( 'NONE', ( #5344, #18503 ) ) ;
#13309 = CARTESIAN_POINT ( 'NONE',  ( 2.247466774197339756, 28.36888560440311480, 6.000000000000000000 ) ) ;
#13308 = CARTESIAN_POINT ( 'NONE',  ( -16.32417823649820932, 19.06887375611960067, -13.74019203237465625 ) ) ;
#13310 = CARTESIAN_POINT ( 'NONE',  ( 13.28710335604435144, 15.51393809808774549, 10.49999999999999822 ) ) ;
#13311 = EDGE_CURVE ( 'NONE', #31854, #37897, #33045, .T. ) ;
#13312 = CARTESIAN_POINT ( 'NONE',  ( 13.68675488944363394, -24.11442831246780472, -13.51430495698268253 ) ) ;
#13313 = CARTESIAN_POINT ( 'NONE',  ( -3.597409820281606940, 14.42008525284352594, 9.000000000000001776 ) ) ;
#13314 = CARTESIAN_POINT ( 'NONE',  ( 11.47989394144907216, 18.44111857959351752, -23.85327845104777467 ) ) ;
#13315 = ORIENTED_EDGE ( 'NONE', *, *, #20103, .F. ) ;
#13316 = CARTESIAN_POINT ( 'NONE',  ( 13.20572627864892290, 22.24225191886345598, -16.44350126499534426 ) ) ;
#13317 = ORIENTED_EDGE ( 'NONE', *, *, #27356, .T. ) ;
#13318 = AXIS2_PLACEMENT_3D ( 'NONE', #15977, #23064, #34660 ) ;
#13320 = FACE_OUTER_BOUND ( 'NONE', #32342, .T. ) ;
#13319 = CARTESIAN_POINT ( 'NONE',  ( -13.44580646965103377, 22.90880309117785529, -15.44002879919819193 ) ) ;
#13321 = CARTESIAN_POINT ( 'NONE',  ( -9.545403281521043226, -18.28601644545607030, -28.07880677660388358 ) ) ;
#13322 = CARTESIAN_POINT ( 'NONE',  ( -34.54873536671436085, -1.828132805472219680, 13.32518128616564468 ) ) ;
#13323 = AXIS2_PLACEMENT_3D ( 'NONE', #34645, #28147, #12703 ) ;
#13324 = ADVANCED_FACE ( 'NONE', ( #14354 ), #1884, .T. ) ;
#13325 = CIRCLE ( 'NONE', #18528, 0.5000000000000004441 ) ;
#13326 = CARTESIAN_POINT ( 'NONE',  ( -30.24448231779780372, -20.88974531296291914, -9.287890822320301609 ) ) ;
#13327 = CARTESIAN_POINT ( 'NONE',  ( -4.167622576179086380, -22.95801459329689820, -15.90121958565441496 ) ) ;
#13328 = CARTESIAN_POINT ( 'NONE',  ( 11.53991419820319919, 17.31783527090524899, -26.86815565160901897 ) ) ;
#13329 = EDGE_LOOP ( 'NONE', ( #36152, #24643 ) ) ;
#13330 = CARTESIAN_POINT ( 'NONE',  ( 21.49103779673273706, 8.702945238107675507, -15.91587550759767211 ) ) ;
#13331 = CARTESIAN_POINT ( 'NONE',  ( 35.34645969586885172, -13.68099284068201982, -4.999999999999999112 ) ) ;
#13332 = CARTESIAN_POINT ( 'NONE',  ( 8.062736477016214209, 35.88854577675294166, 16.87380292611443267 ) ) ;
#13333 = ORIENTED_EDGE ( 'NONE', *, *, #14389, .F. ) ;
#13334 = CARTESIAN_POINT ( 'NONE',  ( -30.42670526058322267, -3.055756317512598130, -12.29337351708506532 ) ) ;
#13335 = CARTESIAN_POINT ( 'NONE',  ( -16.78686424248105524, 15.93842542257001327, 18.42518152272092991 ) ) ;
#13336 = ORIENTED_EDGE ( 'NONE', *, *, #20700, .F. ) ;
#13337 = CARTESIAN_POINT ( 'NONE',  ( 22.38472516250422473, -15.35952186208517745, 20.99999999999999645 ) ) ;
#13338 = CARTESIAN_POINT ( 'NONE',  ( -5.537946624085887670, 36.44027069998197277, 7.000000000000000000 ) ) ;
#13339 = EDGE_CURVE ( 'NONE', #19934, #24994, #17468, .T. ) ;
#13340 = EDGE_CURVE ( 'NONE', #2291, #35955, #36908, .T. ) ;
#13341 = CARTESIAN_POINT ( 'NONE',  ( 26.48686316033968779, -11.60226487929934436, -16.65552626896159083 ) ) ;
#13342 = ADVANCED_FACE ( 'NONE', ( #1360 ), #1215, .T. ) ;
#13343 = CARTESIAN_POINT ( 'NONE',  ( 37.07075634848848011, -14.79048025366225083, 12.14047268033097460 ) ) ;
#13344 = EDGE_LOOP ( 'NONE', ( #12436, #32560, #35741, #198 ) ) ;
#13345 = EDGE_LOOP ( 'NONE', ( #25330, #20796, #38435 ) ) ;
#13346 = CARTESIAN_POINT ( 'NONE',  ( -0.9819677022348329842, 30.37627742347970283, 6.000000000000000000 ) ) ;
#13347 = AXIS2_PLACEMENT_3D ( 'NONE', #3526, #31760, #34608 ) ;
#13348 = CARTESIAN_POINT ( 'NONE',  ( -22.71238962429393382, 10.21442836285774902, -4.999999999999995559 ) ) ;
#13349 = CIRCLE ( 'NONE', #27626, 6.000000000000005329 ) ;
#13350 = CIRCLE ( 'NONE', #31515, 1.000000000000000888 ) ;
#13351 = CARTESIAN_POINT ( 'NONE',  ( 7.577540944421576441, 33.15743037285414374, 13.00000000000000178 ) ) ;
#13352 = ORIENTED_EDGE ( 'NONE', *, *, #7998, .T. ) ;
#13353 = CARTESIAN_POINT ( 'NONE',  ( -1.024090966498643951, 20.73153308134275719, -27.70753136508054126 ) ) ;
#13354 = DIRECTION ( 'NONE',  ( 0.000000000000000000, 0.000000000000000000, 1.000000000000000000 ) ) ;
#13355 = CIRCLE ( 'NONE', #25682, 0.5000000000000012212 ) ;
#13356 = CYLINDRICAL_SURFACE ( 'NONE', #17576, 0.5000000000000004441 ) ;
#13357 = FACE_OUTER_BOUND ( 'NONE', #3447, .T. ) ;
#13358 = DIRECTION ( 'NONE',  ( 0.000000000000000000, 0.000000000000000000, 1.000000000000000000 ) ) ;
#13359 = EDGE_CURVE ( 'NONE', #18163, #38528, #4874, .T. ) ;
#13360 = CARTESIAN_POINT ( 'NONE',  ( 2.618397918551820247, 7.776539141412873946, 10.76099332938164110 ) ) ;
#13361 = CARTESIAN_POINT ( 'NONE',  ( 14.15549368817671372, 29.61663025949119188, -6.828959041903970295 ) ) ;
#13362 = ADVANCED_FACE ( 'NONE', ( #12250 ), #30943, .T. ) ;
#13363 = LINE ( 'NONE', #10320, #25679 ) ;
#13364 = ORIENTED_EDGE ( 'NONE', *, *, #29494, .F. ) ;
#13366 = CARTESIAN_POINT ( 'NONE',  ( -8.007761790012255076, 9.776959832083379709, 7.000000000000000000 ) ) ;
#13365 = CARTESIAN_POINT ( 'NONE',  ( -17.63781053724814640, 11.42380641143947884, -24.41185227018100434 ) ) ;
#13367 = CARTESIAN_POINT ( 'NONE',  ( 13.94482798346721175, 26.50521816028912525, 7.000000000000000000 ) ) ;
#13368 = ADVANCED_FACE ( 'NONE', ( #28083 ), #657, .F. ) ;
#13369 = CARTESIAN_POINT ( 'NONE',  ( 14.11138780488941435, -24.62265220140333355, -12.54540560345105860 ) ) ;
#13370 = CARTESIAN_POINT ( 'NONE',  ( -10.06946225350398194, 32.23940090176283491, 10.00000000000000000 ) ) ;
#13371 = CARTESIAN_POINT ( 'NONE',  ( 11.45548560297930329, 18.46219990532805966, -23.84939050765756363 ) ) ;
#13372 = CARTESIAN_POINT ( 'NONE',  ( -15.29245034862075769, 32.56469986091995850, -4.999999999999987566 ) ) ;
#13373 = CARTESIAN_POINT ( 'NONE',  ( 0.000000000000000000, 0.000000000000000000, 11.00000000000000000 ) ) ;
#13374 = CARTESIAN_POINT ( 'NONE',  ( -22.41958926254718776, -23.75709256622344512, -12.10280908274594758 ) ) ;
#13375 = CARTESIAN_POINT ( 'NONE',  ( 6.261531442577396689, -25.09448364857072633, -5.479386318545421020 ) ) ;
#13376 = CARTESIAN_POINT ( 'NONE',  ( 15.48317245491042904, 26.45281331046393092, -5.946134839014572293 ) ) ;
#13377 = CARTESIAN_POINT ( 'NONE',  ( 20.42207822710955512, -13.80760592411458454, -20.70725840310820232 ) ) ;
#13378 = DIRECTION ( 'NONE',  ( 1.000000000000000000, 0.000000000000000000, 0.000000000000000000 ) ) ;
#13379 = CARTESIAN_POINT ( 'NONE',  ( -8.935776944912362296, 22.65328985282726393, 13.00000000000000178 ) ) ;
#13380 = EDGE_LOOP ( 'NONE', ( #5099, #37129 ) ) ;
#13381 = CARTESIAN_POINT ( 'NONE',  ( -7.784904364235317509, 29.15186949039238229, -14.87099986184792222 ) ) ;
#13382 = CIRCLE ( 'NONE', #25697, 1.000000000000000888 ) ;
#13383 = AXIS2_PLACEMENT_3D ( 'NONE', #24473, #12083, #3335 ) ;
#13384 = CARTESIAN_POINT ( 'NONE',  ( 14.97009266215791889, 21.42933399866927857, 10.49999999999999822 ) ) ;
#13385 = ORIENTED_EDGE ( 'NONE', *, *, #6640, .F. ) ;
#13386 = CARTESIAN_POINT ( 'NONE',  ( 21.71688145637667233, 0.6875768534851390834, -23.84913670212286618 ) ) ;
#13387 = DIRECTION ( 'NONE',  ( 0.7431448254773863615, -0.6691306063588671194, 0.000000000000000000 ) ) ;
#13388 = VECTOR ( 'NONE', #17149, 1000.000000000000000 ) ;
#13389 = DIRECTION ( 'NONE',  ( 1.224646799147351235E-16, -1.000000000000000000, -0.000000000000000000 ) ) ;
#13390 = VERTEX_POINT ( 'NONE', #3701 ) ;
#13391 = CARTESIAN_POINT ( 'NONE',  ( -21.26491060988546167, 0.8575210262421062435, -25.02329962371140581 ) ) ;
#13392 = FACE_OUTER_BOUND ( 'NONE', #29133, .T. ) ;
#13393 = EDGE_LOOP ( 'NONE', ( #38742, #30335, #7244, #38053 ) ) ;
#13394 = CARTESIAN_POINT ( 'NONE',  ( 28.13023995446271286, -6.686838264236121709, -15.87225043224434806 ) ) ;
#13395 = EDGE_CURVE ( 'NONE', #33406, #29912, #3808, .T. ) ;
#13396 = ORIENTED_EDGE ( 'NONE', *, *, #7990, .F. ) ;
#13397 = APPLICATION_PROTOCOL_DEFINITION ( 'draft international standard', 'automotive_design', 1998, #8302 ) ;
#13398 = CARTESIAN_POINT ( 'NONE',  ( -5.746222359017751025, 39.55816310746048003, 11.55979286843935228 ) ) ;
#13399 = DIRECTION ( 'NONE',  ( 0.000000000000000000, 0.000000000000000000, -1.000000000000000000 ) ) ;
#13400 = CARTESIAN_POINT ( 'NONE',  ( -4.244684691011856081, 8.112536183716212435, 7.202682876670047918 ) ) ;
#13401 = CARTESIAN_POINT ( 'NONE',  ( -10.77668768651903619, 26.79111211459810349, 19.66345542862499940 ) ) ;
#13402 = CARTESIAN_POINT ( 'NONE',  ( 5.068835528549735514, 13.82204480395803081, 10.49999999999999822 ) ) ;
#13403 = ORIENTED_EDGE ( 'NONE', *, *, #29999, .F. ) ;
#13404 = PRESENTATION_STYLE_ASSIGNMENT (( #37993 ) ) ;
#13405 = CARTESIAN_POINT ( 'NONE',  ( -16.55039525318069593, 12.10030840459738499, -30.00000000000001066 ) ) ;
#13406 = DIRECTION ( 'NONE',  ( 1.000000000000000000, 0.000000000000000000, 0.000000000000000000 ) ) ;
#13407 = DIRECTION ( 'NONE',  ( -1.000000000000000000, 0.000000000000000000, 0.000000000000000000 ) ) ;
#13408 = CARTESIAN_POINT ( 'NONE',  ( 15.38089657270912092, 16.48686376672722531, -19.92077768951681804 ) ) ;
#13409 = AXIS2_PLACEMENT_3D ( 'NONE', #18007, #12098, #24289 ) ;
#13410 = CARTESIAN_POINT ( 'NONE',  ( 10.81548165185368404, 33.90032711218825767, -7.190669018737369633 ) ) ;
#13411 = VERTEX_POINT ( 'NONE', #25237 ) ;
#13412 = CARTESIAN_POINT ( 'NONE',  ( -10.14060191828654034, 25.26915018278948111, 10.00000000000000000 ) ) ;
#13413 = CARTESIAN_POINT ( 'NONE',  ( 6.082600654608392610, 21.41965916404854298, 6.000000000000000000 ) ) ;
#13414 = EDGE_CURVE ( 'NONE', #1290, #23669, #28621, .T. ) ;
#13415 = CARTESIAN_POINT ( 'NONE',  ( 10.24602814327722555, -18.35173801110022040, -26.18014820733107939 ) ) ;
#13416 = CARTESIAN_POINT ( 'NONE',  ( 14.98890121934609532, -28.67928442654220333, 11.00000000000000000 ) ) ;
#13417 = LINE ( 'NONE', #38604, #26328 ) ;
#13418 = EDGE_LOOP ( 'NONE', ( #14854, #6108, #6731, #37887, #29685, #20703 ) ) ;
#13419 = CARTESIAN_POINT ( 'NONE',  ( -11.02092554839851068, 17.33857933006403229, -28.70757483433319024 ) ) ;
#13420 = CARTESIAN_POINT ( 'NONE',  ( -24.08250333997145631, -26.67951267123966375, 16.30093088680225222 ) ) ;
#13421 = CARTESIAN_POINT ( 'NONE',  ( 10.89336905877927464, -20.52105068520159037, -20.57499638152730270 ) ) ;
#13422 = DIRECTION ( 'NONE',  ( 0.000000000000000000, 0.000000000000000000, 1.000000000000000000 ) ) ;
#13423 = ORIENTED_EDGE ( 'NONE', *, *, #16600, .T. ) ;
#13424 = ORIENTED_EDGE ( 'NONE', *, *, #2018, .T. ) ;
#13425 = CARTESIAN_POINT ( 'NONE',  ( -10.54481009990373330, 22.58364347488284096, -19.17416471084009189 ) ) ;
#13426 = CARTESIAN_POINT ( 'NONE',  ( -12.79957067206351162, -17.39491784009856090, -24.68155700537461072 ) ) ;
#13427 = CARTESIAN_POINT ( 'NONE',  ( -14.86556419889029534, 20.43481210330121556, 10.49999999999999822 ) ) ;
#13428 = CARTESIAN_POINT ( 'NONE',  ( -33.60037199511394590, -8.295775768378332415, -9.823597468572941693 ) ) ;
#13429 = CARTESIAN_POINT ( 'NONE',  ( 7.312035131040564906, 19.41226734497195849, 12.00000000000000000 ) ) ;
#13430 = VERTEX_POINT ( 'NONE', #7340 ) ;
#13431 = CARTESIAN_POINT ( 'NONE',  ( 21.26058458131393891, 0.8877849191941595830, -25.02650145224686895 ) ) ;
#13432 = CARTESIAN_POINT ( 'NONE',  ( 14.06932099033143757, 26.54566839026256631, 11.00000000000000355 ) ) ;
#13433 = FACE_OUTER_BOUND ( 'NONE', #32690, .T. ) ;
#13434 = VERTEX_POINT ( 'NONE', #38634 ) ;
#13435 = CARTESIAN_POINT ( 'NONE',  ( -24.56473081290029015, 0.4207215009515258841, -18.45078781038499471 ) ) ;
#13436 = CARTESIAN_POINT ( 'NONE',  ( -5.238409041734074734, 36.41108174777520645, 10.49999999999999822 ) ) ;
#13437 = ORIENTED_EDGE ( 'NONE', *, *, #5617, .T. ) ;
#13438 = CARTESIAN_POINT ( 'NONE',  ( 20.63680471757680124, -0.9487772221450848642, -27.98716435451661511 ) ) ;
#13439 = AXIS2_PLACEMENT_3D ( 'NONE', #33200, #30547, #14700 ) ;
#13440 = VECTOR ( 'NONE', #33696, 1000.000000000000000 ) ;
#13441 = LINE ( 'NONE', #4302, #6391 ) ;
#13442 = CARTESIAN_POINT ( 'NONE',  ( 32.26342856634837375, -3.257244833652103377, 17.42190598798432077 ) ) ;
#13443 = EDGE_CURVE ( 'NONE', #22657, #21143, #32140, .T. ) ;
#13444 = ORIENTED_EDGE ( 'NONE', *, *, #18952, .F. ) ;
#13445 = CARTESIAN_POINT ( 'NONE',  ( 13.95035364761274543, 31.96289125330678615, 15.13084544680214627 ) ) ;
#13446 = VECTOR ( 'NONE', #36139, 1000.000000000000000 ) ;
#13447 = DIRECTION ( 'NONE',  ( 0.000000000000000000, 0.000000000000000000, 1.000000000000000000 ) ) ;
#13448 = CARTESIAN_POINT ( 'NONE',  ( -5.143258252870523073, 25.23120525497748545, 20.99999999999999645 ) ) ;
#13449 = DIRECTION ( 'NONE',  ( 0.4156269377774580720, 0.5720614028176809196, -0.7071067811865475727 ) ) ;
#13450 = DIRECTION ( 'NONE',  ( -0.7431448254773862505, 0.6691306063588670083, 0.000000000000000000 ) ) ;
#13451 = EDGE_CURVE ( 'NONE', #39486, #6684, #6935, .T. ) ;
#13452 = CARTESIAN_POINT ( 'NONE',  ( -11.11016527260153097, 31.83082137946489354, 11.00000000000000000 ) ) ;
#13453 = CARTESIAN_POINT ( 'NONE',  ( 23.68624114772789824, 7.604278122844164045, 16.87380292611428700 ) ) ;
#13454 = CARTESIAN_POINT ( 'NONE',  ( -19.94779647907517983, 8.036049150339344749, -22.20456094153029625 ) ) ;
#13455 = CARTESIAN_POINT ( 'NONE',  ( 12.98122511323041550, -16.28336372442720403, -27.20012430218251964 ) ) ;
#13456 = CARTESIAN_POINT ( 'NONE',  ( -0.5000000000000004441, 36.00000000000000711, 9.500000000000000000 ) ) ;
#13457 = EDGE_LOOP ( 'NONE', ( #33937, #37507, #502, #31842 ) ) ;
#13458 = CARTESIAN_POINT ( 'NONE',  ( 10.84452725066743106, 17.39679239189240434, -30.00000000000000000 ) ) ;
#13459 = CIRCLE ( 'NONE', #22537, 6.000000000000013323 ) ;
#13460 = ORIENTED_EDGE ( 'NONE', *, *, #32277, .F. ) ;
#13462 = AXIS2_PLACEMENT_3D ( 'NONE', #3149, #27729, #30789 ) ;
#13461 = CARTESIAN_POINT ( 'NONE',  ( -12.07501055264735257, 16.79091931427930007, -27.52101582733411078 ) ) ;
#13463 = CARTESIAN_POINT ( 'NONE',  ( -22.79731396823270018, -22.36677566318123311, 19.66345542862559981 ) ) ;
#13464 = EDGE_CURVE ( 'NONE', #10797, #8399, #23195, .T. ) ;
#13465 = CARTESIAN_POINT ( 'NONE',  ( 8.927394655428274817, 11.06314620770945290, 11.00000000000000000 ) ) ;
#13466 = CARTESIAN_POINT ( 'NONE',  ( 13.80613653353328196, 23.31784988260643132, -14.48073358026558211 ) ) ;
#13467 = ORIENTED_EDGE ( 'NONE', *, *, #32019, .F. ) ;
#13468 = CARTESIAN_POINT ( 'NONE',  ( 20.80092188569423328, -11.47548207259838193, -21.83916146562154736 ) ) ;
#13469 = CARTESIAN_POINT ( 'NONE',  ( -5.644276917315534270, 36.40655018617698602, 10.49999999999999822 ) ) ;
#13470 = VERTEX_POINT ( 'NONE', #22782 ) ;
#13471 = AXIS2_PLACEMENT_3D ( 'NONE', #24895, #12107, #9667 ) ;
#13473 = CARTESIAN_POINT ( 'NONE',  ( -14.97009266215794021, 21.42933399866948463, 10.49999999999999822 ) ) ;
#13472 = CARTESIAN_POINT ( 'NONE',  ( -11.30680158603337482, 18.58912957429523871, -23.82584604873158085 ) ) ;
#13474 = CARTESIAN_POINT ( 'NONE',  ( -14.80989234766682472, -24.23948810107563645, -13.42031711412986539 ) ) ;
#13475 = LINE ( 'NONE', #22819, #27027 ) ;
#13476 = CIRCLE ( 'NONE', #18681, 1.000000000000000000 ) ;
#13477 = ORIENTED_EDGE ( 'NONE', *, *, #17243, .F. ) ;
#13478 = CARTESIAN_POINT ( 'NONE',  ( -22.69874938501649098, -9.396075009901352360, -20.74577302956173241 ) ) ;
#13479 = CARTESIAN_POINT ( 'NONE',  ( -13.22797251932733431, -24.88283229560302701, -11.63121411976873532 ) ) ;
#13480 = DIRECTION ( 'NONE',  ( 1.000000000000000000, 0.000000000000000000, 0.000000000000000000 ) ) ;
#13481 = CARTESIAN_POINT ( 'NONE',  ( 16.39331781465299898, 19.66495602315241698, -12.73500833637442398 ) ) ;
#13482 = ORIENTED_EDGE ( 'NONE', *, *, #31335, .F. ) ;
#13483 = CARTESIAN_POINT ( 'NONE',  ( 27.43674297377669546, 3.779828424379618301, -5.475541599305136842 ) ) ;
#13484 = FACE_OUTER_BOUND ( 'NONE', #20710, .T. ) ;
#13485 = CARTESIAN_POINT ( 'NONE',  ( -24.28032989564857047, -12.76774640304084052, 23.00000000000000000 ) ) ;
#13486 = EDGE_LOOP ( 'NONE', ( #32167, #39668, #21937, #17003 ) ) ;
#13487 = CARTESIAN_POINT ( 'NONE',  ( -31.09037572277983230, -0.2342870890902534753, -4.999999999999999112 ) ) ;
#13488 = CARTESIAN_POINT ( 'NONE',  ( 31.42341880231480644, -0.5937245782808076022, -5.000000000000000888 ) ) ;
#13489 = CARTESIAN_POINT ( 'NONE',  ( 29.47277113412613758, -17.01611234805177730, 19.66345542862528362 ) ) ;
#13490 = VERTEX_POINT ( 'NONE', #35184 ) ;
#13491 = EDGE_CURVE ( 'NONE', #26306, #18033, #31708, .T. ) ;
#13492 = CARTESIAN_POINT ( 'NONE',  ( -27.08779848459120743, 7.221796966026721165, -5.000000000000006217 ) ) ;
#13493 = DIRECTION ( 'NONE',  ( 0.000000000000000000, 0.000000000000000000, 1.000000000000000000 ) ) ;
#13494 = AXIS2_PLACEMENT_3D ( 'NONE', #7039, #3996, #16397 ) ;
#13495 = AXIS2_PLACEMENT_3D ( 'NONE', #30738, #21388, #33795 ) ;
#13496 = DIRECTION ( 'NONE',  ( 0.000000000000000000, 0.000000000000000000, -1.000000000000000000 ) ) ;
#13497 = EDGE_CURVE ( 'NONE', #13434, #23843, #16296, .T. ) ;
#13498 = DIRECTION ( 'NONE',  ( -0.000000000000000000, -0.000000000000000000, -1.000000000000000000 ) ) ;
#13499 = AXIS2_PLACEMENT_3D ( 'NONE', #35843, #2324, #1929 ) ;
#13500 = AXIS2_PLACEMENT_3D ( 'NONE', #19481, #32497, #1406 ) ;
#13501 = DIRECTION ( 'NONE',  ( 0.4067366430758009299, 0.9135454576426006446, 0.000000000000000000 ) ) ;
#13502 = PLANE ( 'NONE',  #4794 ) ;
#13503 = CARTESIAN_POINT ( 'NONE',  ( -13.32151712420406398, 20.09434385051854122, 9.500000000000000000 ) ) ;
#13504 = ORIENTED_EDGE ( 'NONE', *, *, #10388, .F. ) ;
#13505 = CARTESIAN_POINT ( 'NONE',  ( -6.354454053420247384, 35.54304081427990525, 10.99999999999999289 ) ) ;
#13506 = DIRECTION ( 'NONE',  ( 0.000000000000000000, 0.000000000000000000, 1.000000000000000000 ) ) ;
#13507 = CARTESIAN_POINT ( 'NONE',  ( 27.35186887652132626, -23.80825151756206637, -8.882026785022988591 ) ) ;
#13508 = CARTESIAN_POINT ( 'NONE',  ( -7.014595103779441843, 35.79644522156330311, 11.00000000000000000 ) ) ;
#13509 = CARTESIAN_POINT ( 'NONE',  ( 13.46929972531963848, 26.35070966310165375, 7.500000000000000000 ) ) ;
#13510 = CARTESIAN_POINT ( 'NONE',  ( 12.95942736264239947, 22.68428619808883795, -16.38842958060721244 ) ) ;
#13511 = CARTESIAN_POINT ( 'NONE',  ( -6.980762143445979895, 14.59310681135558241, 11.00000000000000000 ) ) ;
#13512 = ORIENTED_EDGE ( 'NONE', *, *, #15353, .T. ) ;
#13513 = CARTESIAN_POINT ( 'NONE',  ( -17.16260375762833590, 18.73914433653179756, -11.78407945085863062 ) ) ;
#13514 = CARTESIAN_POINT ( 'NONE',  ( -23.61737546510203600, -7.194424252576976819, 20.99999999999999645 ) ) ;
#13515 = EDGE_CURVE ( 'NONE', #15244, #22373, #13441, .T. ) ;
#13516 = CARTESIAN_POINT ( 'NONE',  ( 9.512694695443267179, -18.20982909230496816, -28.70727928411922392 ) ) ;
#13517 = EDGE_CURVE ( 'NONE', #32632, #5452, #32348, .T. ) ;
#13518 = DIRECTION ( 'NONE',  ( -1.000000000000000000, 0.000000000000000000, 0.000000000000000000 ) ) ;
#13519 = CARTESIAN_POINT ( 'NONE',  ( 15.34485063204045829, 26.59437119930156967, -6.887952992160583321 ) ) ;
#13520 = ORIENTED_EDGE ( 'NONE', *, *, #11173, .F. ) ;
#13521 = CARTESIAN_POINT ( 'NONE',  ( 14.28551598028751890, 24.48525218155484851, -12.54977972690513077 ) ) ;
#13522 = ORIENTED_EDGE ( 'NONE', *, *, #7253, .T. ) ;
#13524 = DIRECTION ( 'NONE',  ( 1.000000000000000000, 0.000000000000000000, 0.000000000000000000 ) ) ;
#13523 = CARTESIAN_POINT ( 'NONE',  ( -11.64607099366300780, 18.95003504881763590, -22.72817784514300143 ) ) ;
#13525 = CARTESIAN_POINT ( 'NONE',  ( -12.27294156613012177, -22.02301600987046371, -17.43937061174498027 ) ) ;
#13526 = CARTESIAN_POINT ( 'NONE',  ( -33.93864557197014165, -21.81860479675889053, 12.73282698324848283 ) ) ;
#13527 = AXIS2_PLACEMENT_3D ( 'NONE', #7651, #38736, #29589 ) ;
#13528 = AXIS2_PLACEMENT_3D ( 'NONE', #16420, #22704, #19460 ) ;
#13529 = CARTESIAN_POINT ( 'NONE',  ( -25.34274736433472697, -16.37843956862553085, -15.68371574493890286 ) ) ;
#13530 = CARTESIAN_POINT ( 'NONE',  ( -6.988245995732859761, -25.03642915341433905, -7.403757448750240222 ) ) ;
#13531 = CARTESIAN_POINT ( 'NONE',  ( 15.63852180243771528, 25.36448989093083384, -7.362413517827306464 ) ) ;
#13532 = ORIENTED_EDGE ( 'NONE', *, *, #4858, .T. ) ;
#13533 = CARTESIAN_POINT ( 'NONE',  ( 22.92399774901786458, 9.099773806377163154, -9.874741973018776875 ) ) ;
#13534 = CARTESIAN_POINT ( 'NONE',  ( 17.76739296776033683, 31.93461337800236777, 11.00000000000000178 ) ) ;
#13535 = CARTESIAN_POINT ( 'NONE',  ( -12.37185181069348161, 14.01743714881896530, 7.203056206335839207 ) ) ;
#13536 = CARTESIAN_POINT ( 'NONE',  ( -1.325463245115554520E-13, 37.48425883190013508, 17.42190598798392642 ) ) ;
#13537 = AXIS2_PLACEMENT_3D ( 'NONE', #14914, #17779, #39881 ) ;
#13538 = ORIENTED_EDGE ( 'NONE', *, *, #21533, .F. ) ;
#13539 = CARTESIAN_POINT ( 'NONE',  ( -32.91670029435780265, -2.547476605001916194, -5.917534263431005748 ) ) ;
#13540 = CARTESIAN_POINT ( 'NONE',  ( -14.11133924723977628, 27.61078317377193869, 10.50000000000000000 ) ) ;
#13541 = ORIENTED_EDGE ( 'NONE', *, *, #30308, .F. ) ;
#13542 = CARTESIAN_POINT ( 'NONE',  ( 23.81569860407207884, -13.75000000000005329, 20.99999999999999645 ) ) ;
#13543 = FACE_OUTER_BOUND ( 'NONE', #33439, .T. ) ;
#13544 = EDGE_CURVE ( 'NONE', #24143, #13849, #21964, .T. ) ;
#13545 = CARTESIAN_POINT ( 'NONE',  ( 32.57092086225112837, -15.43378303256681505, -10.17932366030892588 ) ) ;
#13546 = CARTESIAN_POINT ( 'NONE',  ( 28.24711154207348685, -27.09388640670305648, 11.55979286843937892 ) ) ;
#13547 = ORIENTED_EDGE ( 'NONE', *, *, #29005, .F. ) ;
#13548 = VERTEX_POINT ( 'NONE', #16910 ) ;
#13549 = FACE_OUTER_BOUND ( 'NONE', #4661, .T. ) ;
#13550 = CYLINDRICAL_SURFACE ( 'NONE', #7152, 0.5000000000000004441 ) ;
#13551 = VECTOR ( 'NONE', #39651, 1000.000000000000000 ) ;
#13552 = CIRCLE ( 'NONE', #33046, 1.000000000000004441 ) ;
#13553 = CARTESIAN_POINT ( 'NONE',  ( 0.000000000000000000, 22.50000000000000355, 7.000000000000000000 ) ) ;
#13554 = ORIENTED_EDGE ( 'NONE', *, *, #5509, .F. ) ;
#13555 = CARTESIAN_POINT ( 'NONE',  ( -1.740872439423108764, 34.41729727890611912, -11.97610320120729632 ) ) ;
#13556 = CARTESIAN_POINT ( 'NONE',  ( -13.77067693704740492, 28.44713853003868564, 7.000000000000000000 ) ) ;
#13557 = CARTESIAN_POINT ( 'NONE',  ( -10.04974741695039242, 22.44923726269184527, 10.49999999999999467 ) ) ;
#13558 = VECTOR ( 'NONE', #4312, 1000.000000000000000 ) ;
#13559 = CARTESIAN_POINT ( 'NONE',  ( -3.153820973115282644, 32.04219121950185212, 10.50000000000000533 ) ) ;
#13560 = DIRECTION ( 'NONE',  ( -0.07391278520355981652, 0.7032331762534046460, 0.7071067811865479058 ) ) ;
#13561 = CARTESIAN_POINT ( 'NONE',  ( -9.911438049898041669, 11.24107483890965575, 7.000000000000000000 ) ) ;
#13562 = CARTESIAN_POINT ( 'NONE',  ( 14.07960931274568672, 28.37400713639219418, -9.127921161272693595 ) ) ;
#13563 = DIRECTION ( 'NONE',  ( 1.000000000000000000, 0.000000000000000000, 0.000000000000000000 ) ) ;
#13564 = VERTEX_POINT ( 'NONE', #12377 ) ;
#13566 = CARTESIAN_POINT ( 'NONE',  ( -7.611215932167763043, 18.68301270189229513, 9.000000000000001776 ) ) ;
#13565 = CARTESIAN_POINT ( 'NONE',  ( -16.95965515916876498, 11.87563068946122158, -26.61073229064057699 ) ) ;
#13567 = CARTESIAN_POINT ( 'NONE',  ( -15.33540832684330724, 35.51988609203693414, 11.00000000000000000 ) ) ;
#13568 = CARTESIAN_POINT ( 'NONE',  ( 13.77482710089912210, -24.12599296267502069, -13.50787276857876229 ) ) ;
#13569 = CARTESIAN_POINT ( 'NONE',  ( 12.49038105676654276, 14.13397459621550389, 10.49999999999999822 ) ) ;
#13570 = CARTESIAN_POINT ( 'NONE',  ( 12.90549922656808413, 21.69123041792454032, -17.43238391223398764 ) ) ;
#13571 = CARTESIAN_POINT ( 'NONE',  ( -16.24796006241077961, 15.88921519459651499, -30.00000000000001421 ) ) ;
#13572 = DIRECTION ( 'NONE',  ( -1.000000000000000000, 0.000000000000000000, 0.000000000000000000 ) ) ;
#13573 = ADVANCED_FACE ( 'NONE', ( #393 ), #15827, .F. ) ;
#13574 = CARTESIAN_POINT ( 'NONE',  ( -25.65315598498527194, -24.12413061561075622, -9.790106673725071929 ) ) ;
#13575 = CARTESIAN_POINT ( 'NONE',  ( 6.952732471630988620, -22.26205726029128584, -17.83880605057320423 ) ) ;
#13576 = CARTESIAN_POINT ( 'NONE',  ( 15.46210322845357155, 26.52717532233935316, -5.946118077167572125 ) ) ;
#13577 = CARTESIAN_POINT ( 'NONE',  ( 20.20733478970500840, 13.69637775999485640, -9.885393215995732064 ) ) ;
#13578 = CARTESIAN_POINT ( 'NONE',  ( 6.348106467989403257, 35.16482219193073178, 12.00000000000000000 ) ) ;
#13579 = CARTESIAN_POINT ( 'NONE',  ( 5.092030333742720849, 36.31140934042893065, 10.49999999999999822 ) ) ;
#13580 = VERTEX_POINT ( 'NONE', #7070 ) ;
#13581 = CARTESIAN_POINT ( 'NONE',  ( -6.014539584152595708, 22.60354644530256607, -22.04821685920930463 ) ) ;
#13582 = ORIENTED_EDGE ( 'NONE', *, *, #3268, .F. ) ;
#13583 = VECTOR ( 'NONE', #7816, 1000.000000000000000 ) ;
#13584 = FACE_OUTER_BOUND ( 'NONE', #10499, .T. ) ;
#13585 = ORIENTED_EDGE ( 'NONE', *, *, #17620, .F. ) ;
#13586 = CARTESIAN_POINT ( 'NONE',  ( 28.90646526158858265, 0.08205528372900385004, -11.59832840213325866 ) ) ;
#13587 = CARTESIAN_POINT ( 'NONE',  ( -7.917741276437941345, 30.52956727630665057, 13.00000000000000178 ) ) ;
#13588 = FACE_OUTER_BOUND ( 'NONE', #9547, .T. ) ;
#13589 = VECTOR ( 'NONE', #13804, 1000.000000000000114 ) ;
#13590 = PRODUCT_DEFINITION_SHAPE ( 'NONE', 'NONE',  #17230 ) ;
#13591 = ORIENTED_EDGE ( 'NONE', *, *, #4282, .F. ) ;
#13592 = CARTESIAN_POINT ( 'NONE',  ( -20.81252836718331167, 0.8663108682335884936, -26.83334811610091464 ) ) ;
#13593 = EDGE_CURVE ( 'NONE', #29442, #12596, #28014, .T. ) ;
#13594 = ORIENTED_EDGE ( 'NONE', *, *, #17970, .F. ) ;
#13595 = CARTESIAN_POINT ( 'NONE',  ( 35.44138113946621615, -9.599287445864765900, -5.000000000000010658 ) ) ;
#13596 = EDGE_CURVE ( 'NONE', #22179, #15406, #4458, .T. ) ;
#13597 = ORIENTED_EDGE ( 'NONE', *, *, #10777, .T. ) ;
#13598 = DIRECTION ( 'NONE',  ( 0.000000000000000000, 0.000000000000000000, 1.000000000000000000 ) ) ;
#13599 = CARTESIAN_POINT ( 'NONE',  ( -3.900486991066758780, 40.17991855517993116, 11.55979286843953169 ) ) ;
#13600 = FACE_OUTER_BOUND ( 'NONE', #24152, .T. ) ;
#13601 = CARTESIAN_POINT ( 'NONE',  ( -4.475131784526824141, 8.183115020678636498, 7.000000000000000000 ) ) ;
#13602 = CARTESIAN_POINT ( 'NONE',  ( 5.983876423892909635, 32.43697950591679557, 19.66345542862528362 ) ) ;
#13603 = EDGE_CURVE ( 'NONE', #27813, #37255, #16230, .T. ) ;
#13604 = CARTESIAN_POINT ( 'NONE',  ( -0.6057027746881266106, 27.44183462127829642, 12.00000000000000000 ) ) ;
#13605 = ORIENTED_EDGE ( 'NONE', *, *, #25974, .T. ) ;
#13606 =( LENGTH_UNIT ( ) NAMED_UNIT ( * ) SI_UNIT ( .MILLI., .METRE. ) );
#13607 = CARTESIAN_POINT ( 'NONE',  ( 7.618377661053323813, 10.47536095541698486, 7.500000000000000888 ) ) ;
#13608 = LINE ( 'NONE', #38798, #13068 ) ;
#13609 = FACE_OUTER_BOUND ( 'NONE', #2905, .T. ) ;
#13610 = CARTESIAN_POINT ( 'NONE',  ( 13.76818825652920353, 15.24450382255247050, -28.80311538815760031 ) ) ;
#13612 = VECTOR ( 'NONE', #3321, 1000.000000000000114 ) ;
#13611 = CARTESIAN_POINT ( 'NONE',  ( 5.765122233821920794, 19.89527052026323517, -27.81238314162991898 ) ) ;
#13613 = ORIENTED_EDGE ( 'NONE', *, *, #33112, .T. ) ;
#13614 = DIRECTION ( 'NONE',  ( -1.000000000000000000, 0.000000000000000000, 0.000000000000000000 ) ) ;
#13615 = LINE ( 'NONE', #3123, #10372 ) ;
#13616 = CARTESIAN_POINT ( 'NONE',  ( 15.49271691873735968, -25.80169155014763405, -10.13838130885175559 ) ) ;
#13617 = DIRECTION ( 'NONE',  ( 0.000000000000000000, 0.000000000000000000, 1.000000000000000000 ) ) ;
#13618 = AXIS2_PLACEMENT_3D ( 'NONE', #33907, #16209, #22891 ) ;
#13619 = EDGE_CURVE ( 'NONE', #15223, #11176, #37565, .T. ) ;
#13620 = DIRECTION ( 'NONE',  ( 0.000000000000000000, 0.000000000000000000, 1.000000000000000000 ) ) ;
#13621 = EDGE_CURVE ( 'NONE', #5398, #16864, #20364, .T. ) ;
#13622 = ORIENTED_EDGE ( 'NONE', *, *, #14285, .T. ) ;
#13623 = CARTESIAN_POINT ( 'NONE',  ( -12.65871080218516731, 21.04530515263928336, -18.45346255153580373 ) ) ;
#13624 = CARTESIAN_POINT ( 'NONE',  ( -17.23228185427209169, -26.71557896778001862, 16.87380292611433674 ) ) ;
#13625 = CARTESIAN_POINT ( 'NONE',  ( 13.65683774811633455, -24.55498886789716551, -12.56460507296711349 ) ) ;
#13626 = CYLINDRICAL_SURFACE ( 'NONE', #28289, 0.5000000000000004441 ) ;
#13627 = VERTEX_POINT ( 'NONE', #9735 ) ;
#13628 = B_SPLINE_CURVE_WITH_KNOTS ( 'NONE', 3,
 ( #5026, #38954, #26759, #19870, #35713, #29003 ),
 .UNSPECIFIED., .F., .F.,
 ( 4, 2, 4 ),
 ( 0.3999999999265801964, 0.6999999999632900982, 1.000000000000000000 ),
 .UNSPECIFIED. ) ;
#13629 = ORIENTED_EDGE ( 'NONE', *, *, #17865, .F. ) ;
#13630 = CARTESIAN_POINT ( 'NONE',  ( -9.954087448707369390, 21.17613213146948681, -21.29198274210564534 ) ) ;
#13631 = CARTESIAN_POINT ( 'NONE',  ( -6.354454053420242943, 35.54304081427989814, 11.00000000000000000 ) ) ;
#13632 = FACE_BOUND ( 'NONE', #22168, .T. ) ;
#13633 = CARTESIAN_POINT ( 'NONE',  ( -19.98679978234304144, -4.924167105727923044, -28.51946357198569970 ) ) ;
#13634 = CARTESIAN_POINT ( 'NONE',  ( -8.927394655428429360, 11.06314620770957013, 9.000000000000001776 ) ) ;
#13635 = ORIENTED_EDGE ( 'NONE', *, *, #32717, .F. ) ;
#13636 = CARTESIAN_POINT ( 'NONE',  ( 21.67939327573176911, 0.8834818022177464147, -23.87219493357654443 ) ) ;
#13637 = DIRECTION ( 'NONE',  ( 0.5877852522924690293, -0.8090169943749503378, 0.000000000000000000 ) ) ;
#13638 = CARTESIAN_POINT ( 'NONE',  ( 14.92615392307456368, 21.72537115092769611, 10.49999999999999467 ) ) ;
#13639 = UNCERTAINTY_MEASURE_WITH_UNIT (LENGTH_MEASURE( 1.000000000000000082E-05 ), #26344, 'distance_accuracy_value', 'NONE');
#13640 = VERTEX_POINT ( 'NONE', #6866 ) ;
#13641 = CARTESIAN_POINT ( 'NONE',  ( -20.61058943125449971, 0.8469614167685917128, -28.07733840680127813 ) ) ;
#13642 = CARTESIAN_POINT ( 'NONE',  ( -5.305271391458861174, 36.43775379931907565, 10.49999999999999822 ) ) ;
#13643 = ADVANCED_FACE ( 'NONE', ( #34516 ), #23283, .T. ) ;
#13644 = ORIENTED_EDGE ( 'NONE', *, *, #14361, .T. ) ;
#13645 = CARTESIAN_POINT ( 'NONE',  ( 32.29748657415021995, -3.057573243849562861, -9.081205313942463775 ) ) ;
#13646 = DIRECTION ( 'NONE',  ( -0.5877852522924796874, -0.8090169943749426773, 0.000000000000000000 ) ) ;
#13647 = CARTESIAN_POINT ( 'NONE',  ( 34.65585262756915341, -3.900084976043348917, 15.13084544680213561 ) ) ;
#13648 = ADVANCED_FACE ( 'NONE', ( #34318 ), #9537, .F. ) ;
#13649 = VERTEX_POINT ( 'NONE', #37961 ) ;
#13650 = CARTESIAN_POINT ( 'NONE',  ( 14.63453729950972537, 30.27278626593263056, 15.72805884748936300 ) ) ;
#13651 = CARTESIAN_POINT ( 'NONE',  ( -5.304193131309156151, -23.76115801358234947, 17.42190598798392998 ) ) ;
#13652 = DIRECTION ( 'NONE',  ( -2.168404344971006896E-16, 1.000000000000000000, 0.000000000000000000 ) ) ;
#13653 = CARTESIAN_POINT ( 'NONE',  ( 1.431596709943214973, 28.99142433710780864, 20.94377226548377990 ) ) ;
#13654 = CARTESIAN_POINT ( 'NONE',  ( 11.94134295108990074, 16.18301270189217433, 9.500000000000000000 ) ) ;
#13655 = CARTESIAN_POINT ( 'NONE',  ( -3.610593701936585909, 31.83882289796395426, 10.50000000000000888 ) ) ;
#13656 = VECTOR ( 'NONE', #3115, 999.9999999999998863 ) ;
#13657 = CARTESIAN_POINT ( 'NONE',  ( -8.238488885696254371, 24.65111619403957022, 7.000000000000000000 ) ) ;
#13658 = CARTESIAN_POINT ( 'NONE',  ( 25.49469310289003232, 2.228649397472089788, 18.42518152273312637 ) ) ;
#13659 = VECTOR ( 'NONE', #25301, 1000.000000000000000 ) ;
#13660 = CARTESIAN_POINT ( 'NONE',  ( -21.05291937318205342, 8.312515282553865958, -17.97409977038949691 ) ) ;
#13661 = CARTESIAN_POINT ( 'NONE',  ( 12.82234224798668976, -16.09375609578110655, -28.57231939863815739 ) ) ;
#13662 = CARTESIAN_POINT ( 'NONE',  ( -14.45538749008468038, 26.50521816028845734, 7.489440493383480835 ) ) ;
#13663 = CARTESIAN_POINT ( 'NONE',  ( 11.80270328479468311, 19.47748869397488392, -21.59992045479478762 ) ) ;
#13664 = ORIENTED_EDGE ( 'NONE', *, *, #22736, .T. ) ;
#13665 = CARTESIAN_POINT ( 'NONE',  ( -11.79678012972095047, 16.99765053083067556, -27.50177182085873540 ) ) ;
#13666 = CARTESIAN_POINT ( 'NONE',  ( -19.07515557932271832, -22.84232221370076488, 19.66345542862558915 ) ) ;
#13667 = CARTESIAN_POINT ( 'NONE',  ( 10.81260707898150386, 32.90853150812155548, 10.49999999999999822 ) ) ;
#13668 = CARTESIAN_POINT ( 'NONE',  ( 14.31934378920023043, 24.39963677761549121, -12.55310820702660557 ) ) ;
#13669 = ORIENTED_EDGE ( 'NONE', *, *, #27618, .F. ) ;
#13670 = CARTESIAN_POINT ( 'NONE',  ( 33.16930538569719999, -19.62507065308114917, -5.435330440035552435 ) ) ;
#13671 = ADVANCED_FACE ( 'NONE', ( #784 ), #28412, .T. ) ;
#13672 = DIRECTION ( 'NONE',  ( 0.4731467892558179900, 0.5254827454987496260, -0.7071067811865524577 ) ) ;
#13673 = CIRCLE ( 'NONE', #24066, 1.000000000000004441 ) ;
#13674 = EDGE_LOOP ( 'NONE', ( #12640, #28464, #4141, #38378 ) ) ;
#13676 = DIRECTION ( 'NONE',  ( 0.000000000000000000, 0.000000000000000000, -1.000000000000000000 ) ) ;
#13675 = CARTESIAN_POINT ( 'NONE',  ( -12.51073218500047801, 21.26417290573970220, -18.42108626876654043 ) ) ;
#13677 = CARTESIAN_POINT ( 'NONE',  ( -16.20081666663972797, -26.89087236765021061, -5.938530992383368456 ) ) ;
#13678 = CARTESIAN_POINT ( 'NONE',  ( 13.58398418571186816, 16.13684478916777820, 7.102637441331451029 ) ) ;
#13679 = ORIENTED_EDGE ( 'NONE', *, *, #23257, .F. ) ;
#13680 = CARTESIAN_POINT ( 'NONE',  ( -18.93673219582609946, -7.851978407254149417, -30.00000000000000711 ) ) ;
#13681 = CARTESIAN_POINT ( 'NONE',  ( -9.018257521923398912, -18.41052938026230024, -29.35785334563086835 ) ) ;
#13682 = CARTESIAN_POINT ( 'NONE',  ( 14.36830325120613594, 20.48707633493483371, 9.000000000000001776 ) ) ;
#13683 = CARTESIAN_POINT ( 'NONE',  ( 13.48020054446795868, 16.18221087160424432, -25.26925449299266901 ) ) ;
#13684 = ORIENTED_EDGE ( 'NONE', *, *, #32693, .T. ) ;
#13685 = CARTESIAN_POINT ( 'NONE',  ( 20.70282115146825319, 3.793121191063287156, -25.28431974125459192 ) ) ;
#13686 = DIRECTION ( 'NONE',  ( -0.000000000000000000, -0.000000000000000000, -1.000000000000000000 ) ) ;
#13687 = CARTESIAN_POINT ( 'NONE',  ( -24.08646667827930443, -13.28101593840485073, 23.00000000000000000 ) ) ;
#13688 = EDGE_LOOP ( 'NONE', ( #6296, #21525, #39014, #24223, #16580, #29436, #32013, #33040, #6978, #11752, #21024, #35094, #24463, #14031, #21149, #6891, #4305, #15647, #19092, #7277, #3153, #24922, #26956, #19218, #19558, #27014, #32044, #2888, #26281, #37455, #6594, #20990, #3161, #34884, #5454, #35886, #26608, #20237, #18206, #31972, #14532, #17950, #30605, #14898, #5797, #8260, #6062, #8833, #13264, #13888, #11043, #2176, #28537, #28420, #14401, #37684, #1123, #28534, #16482, #3266, #29640, #35105 ) ) ;
#13689 = CARTESIAN_POINT ( 'NONE',  ( -20.53452984402690973, 0.6885224814544792515, -28.70101917630290345 ) ) ;
#13690 = CARTESIAN_POINT ( 'NONE',  ( 31.01929709654494260, -0.7441688249631136509, -8.261849393656827800 ) ) ;
#13691 = CIRCLE ( 'NONE', #38371, 1.000000000000000000 ) ;
#13692 = CARTESIAN_POINT ( 'NONE',  ( 27.45400382858955268, -18.53605996571758752, 19.99202127657132877 ) ) ;
#13693 = VECTOR ( 'NONE', #661, 1000.000000000000000 ) ;
#13694 = VERTEX_POINT ( 'NONE', #15428 ) ;
#13695 = CARTESIAN_POINT ( 'NONE',  ( -22.50952045769495413, 1.338071129232386802, -21.70479210668387182 ) ) ;
#13696 = CARTESIAN_POINT ( 'NONE',  ( -3.091399026088746727, 22.35909668862748134, -19.80438750953544513 ) ) ;
#13697 = LINE ( 'NONE', #32406, #16709 ) ;
#13698 = CARTESIAN_POINT ( 'NONE',  ( -14.47283171447380390, 21.48159823030330884, 7.000000000000000000 ) ) ;
#13699 = EDGE_CURVE ( 'NONE', #37009, #15678, #9361, .T. ) ;
#13700 = CIRCLE ( 'NONE', #14355, 1.000000000000000888 ) ;
#13701 = CARTESIAN_POINT ( 'NONE',  ( -11.58426073497328801, 31.66040656113770169, 10.49999999999999822 ) ) ;
#13702 = DIRECTION ( 'NONE',  ( 1.000000000000000000, 0.000000000000000000, 0.000000000000000000 ) ) ;
#13703 = DIRECTION ( 'NONE',  ( -0.9135454576426004225, 0.4067366430758009854, 0.000000000000000000 ) ) ;
#13704 = VERTEX_POINT ( 'NONE', #18680 ) ;
#13705 = DIRECTION ( 'NONE',  ( 0.8660254037844364872, -0.5000000000000038858, 0.000000000000000000 ) ) ;
#13706 = DIRECTION ( 'NONE',  ( -0.7431448254773862505, 0.6691306063588672304, -0.000000000000000000 ) ) ;
#13707 = CARTESIAN_POINT ( 'NONE',  ( 23.17521898255445834, -20.18490097291412155, -14.80311732295303351 ) ) ;
#13708 = CARTESIAN_POINT ( 'NONE',  ( 0.3582258883630317636, 11.68927977431952137, 6.000000000000000000 ) ) ;
#13709 = CARTESIAN_POINT ( 'NONE',  ( -2.317734025672945286, 9.191051544684766483, 10.50000000000000000 ) ) ;
#13710 = CARTESIAN_POINT ( 'NONE',  ( 12.90714127504553055, 22.77320297353917411, -16.37761627767333650 ) ) ;
#13711 = DIRECTION ( 'NONE',  ( 0.000000000000000000, 0.000000000000000000, 1.000000000000000000 ) ) ;
#13712 = ORIENTED_EDGE ( 'NONE', *, *, #6811, .T. ) ;
#13713 = AXIS2_PLACEMENT_3D ( 'NONE', #37943, #37350, #30861 ) ;
#13714 = CARTESIAN_POINT ( 'NONE',  ( -14.15788581485469422, 15.50092647220509612, -25.32911243468907614 ) ) ;
#13715 = CARTESIAN_POINT ( 'NONE',  ( -20.38753357181593628, -16.19769905861790349, 20.99999999999999645 ) ) ;
#13716 = CONICAL_SURFACE ( 'NONE', #27269, 0.4999999999999947264, 0.7853981633974479459 ) ;
#13717 = EDGE_CURVE ( 'NONE', #36138, #839, #15472, .T. ) ;
#13718 = CARTESIAN_POINT ( 'NONE',  ( 9.465986449187253626, -18.23380396764607525, -28.70911249201515147 ) ) ;
#13719 = LINE ( 'NONE', #19216, #18523 ) ;
#13720 = CARTESIAN_POINT ( 'NONE',  ( 14.94370345678945888, 25.77223918896596189, -9.709399778286011085 ) ) ;
#13721 = EDGE_LOOP ( 'NONE', ( #32784, #21173, #37393, #35181, #37844, #38957 ) ) ;
#13722 = CARTESIAN_POINT ( 'NONE',  ( 12.13093762266853837, 19.92385368760829323, -20.54106352598588003 ) ) ;
#13723 = ORIENTED_EDGE ( 'NONE', *, *, #16513, .T. ) ;
#13725 = CARTESIAN_POINT ( 'NONE',  ( 8.118377661053333583, 10.47536095541699197, 11.00000000000000000 ) ) ;
#13724 = CARTESIAN_POINT ( 'NONE',  ( -12.89788825750088819, 21.70392749762217122, -17.43064730788859507 ) ) ;
#13726 = CARTESIAN_POINT ( 'NONE',  ( -11.50915682881853286, -20.98128273221263029, -19.50078698021883028 ) ) ;
#13727 = CARTESIAN_POINT ( 'NONE',  ( -36.74707368630851789, -16.71203845619716333, 11.00000000000030553 ) ) ;
#13728 = CARTESIAN_POINT ( 'NONE',  ( -32.85619107660216542, -19.84207158267233595, -6.275925487822830995 ) ) ;
#13729 = CARTESIAN_POINT ( 'NONE',  ( -1.793625933065454037, -20.61433429535822626, -27.17456019479941176 ) ) ;
#13730 = CARTESIAN_POINT ( 'NONE',  ( 15.21005260476538190, 24.06451757296145999, -10.68341754272937649 ) ) ;
#13731 = EDGE_CURVE ( 'NONE', #17829, #23066, #39277, .T. ) ;
#13732 = VERTEX_POINT ( 'NONE', #28213 ) ;
#13733 = CARTESIAN_POINT ( 'NONE',  ( 23.94499769980229686, 8.291951293815612800, -6.930188724025407865 ) ) ;
#13734 = CARTESIAN_POINT ( 'NONE',  ( -17.76739296776035459, 31.93461337800233224, 11.00000000000000000 ) ) ;
#13735 = VECTOR ( 'NONE', #36980, 1000.000000000000000 ) ;
#13736 = CARTESIAN_POINT ( 'NONE',  ( 5.023663291607745940, -24.92826071495466067, -5.000000000000003553 ) ) ;
#13737 = EDGE_CURVE ( 'NONE', #34838, #36944, #32358, .T. ) ;
#13738 = CARTESIAN_POINT ( 'NONE',  ( 10.74031445979388621, 33.85370084240154398, 16.87380292611439714 ) ) ;
#13739 = ORIENTED_EDGE ( 'NONE', *, *, #7998, .F. ) ;
#13740 = CARTESIAN_POINT ( 'NONE',  ( -21.07773708785227740, -1.860215743600160287, -25.99199685066085053 ) ) ;
#13741 = FACE_OUTER_BOUND ( 'NONE', #8088, .T. ) ;
#13742 = ORIENTED_EDGE ( 'NONE', *, *, #11291, .F. ) ;
#13743 = CARTESIAN_POINT ( 'NONE',  ( 24.28032989564876232, -12.76774640304080144, 20.99999999999999645 ) ) ;
#13744 = DIRECTION ( 'NONE',  ( 1.000000000000000000, 0.000000000000000000, 0.000000000000000000 ) ) ;
#13745 = DIRECTION ( 'NONE',  ( 0.000000000000000000, 0.000000000000000000, 1.000000000000000000 ) ) ;
#13746 = CARTESIAN_POINT ( 'NONE',  ( 19.01366704504291150, -7.688495684904649963, -30.00000000000000355 ) ) ;
#13747 = CARTESIAN_POINT ( 'NONE',  ( 37.58754968649113692, -10.91577297561512339, 11.55979286843927234 ) ) ;
#13748 = EDGE_CURVE ( 'NONE', #21064, #9701, #188, .T. ) ;
#13749 = ORIENTED_EDGE ( 'NONE', *, *, #26548, .F. ) ;
#13750 = ADVANCED_FACE ( 'NONE', ( #3630 ), #588, .T. ) ;
#13751 = CYLINDRICAL_SURFACE ( 'NONE', #16502, 6.000000000000004441 ) ;
#13752 = DIRECTION ( 'NONE',  ( -1.000000000000000000, 0.000000000000000000, 0.000000000000000000 ) ) ;
#13753 = DIRECTION ( 'NONE',  ( 0.000000000000000000, 0.000000000000000000, 1.000000000000000000 ) ) ;
#13754 = EDGE_LOOP ( 'NONE', ( #6739, #32294 ) ) ;
#13755 = CARTESIAN_POINT ( 'NONE',  ( -1.059180177458202587, 21.41711868205623048, -25.58062077214095353 ) ) ;
#13756 = CARTESIAN_POINT ( 'NONE',  ( -9.221287281574669592, 10.65863771052209863, 10.50000000000000000 ) ) ;
#13757 = DIRECTION ( 'NONE',  ( 1.000000000000000000, 0.000000000000000000, 0.000000000000000000 ) ) ;
#13758 = CIRCLE ( 'NONE', #134, 0.5000000000000004441 ) ;
#13759 = LINE ( 'NONE', #26756, #30974 ) ;
#13760 = CARTESIAN_POINT ( 'NONE',  ( -15.02235689379176620, 21.92659494635362449, 10.49999999999999467 ) ) ;
#13761 = DIRECTION ( 'NONE',  ( -0.2079116908177533751, 0.9781476007338069101, 0.000000000000000000 ) ) ;
#13762 = CARTESIAN_POINT ( 'NONE',  ( 10.92821648837030679, 22.20508130926659263, -19.23066798073530848 ) ) ;
#13763 = CARTESIAN_POINT ( 'NONE',  ( -7.688306800005769048, 28.52217545723006609, 13.00000000000000178 ) ) ;
#13764 = ORIENTED_EDGE ( 'NONE', *, *, #8732, .T. ) ;
#13765 = AXIS2_PLACEMENT_3D ( 'NONE', #12289, #12483, #24877 ) ;
#13767 = DIRECTION ( 'NONE',  ( 0.6216356077939706459, 0.000000000000000000, 0.7833065626704660556 ) ) ;
#13766 = CARTESIAN_POINT ( 'NONE',  ( -19.70096002242896560, 14.23449510804272755, -10.87519445515239980 ) ) ;
#13768 = CARTESIAN_POINT ( 'NONE',  ( -4.706342468480190000, 20.64589803375067945, 13.00000000000000178 ) ) ;
#13769 = AXIS2_PLACEMENT_3D ( 'NONE', #33416, #11667, #21203 ) ;
#13770 = CARTESIAN_POINT ( 'NONE',  ( 15.34394143031894409, -26.51021667783368230, -7.357393351511376522 ) ) ;
#13771 = FACE_OUTER_BOUND ( 'NONE', #30015, .T. ) ;
#13772 = CARTESIAN_POINT ( 'NONE',  ( 15.00437511166292026, 26.01395306337788682, -9.236044269556060726 ) ) ;
#13773 = CARTESIAN_POINT ( 'NONE',  ( -37.62663912510979003, -8.659558992827880886, -5.000000000000002665 ) ) ;
#13774 = EDGE_CURVE ( 'NONE', #14341, #31871, #8347, .T. ) ;
#13775 = CARTESIAN_POINT ( 'NONE',  ( -23.74716486098165547, -8.578626677874071405, 23.00000000000000000 ) ) ;
#13776 = CARTESIAN_POINT ( 'NONE',  ( -26.34173717234437362, -23.36365984272380203, -10.22141036450111429 ) ) ;
#13777 = CONICAL_SURFACE ( 'NONE', #4027, 1.000000000000006883, 0.7853981633974549403 ) ;
#13778 = CARTESIAN_POINT ( 'NONE',  ( 5.271459200338986406, -22.64434140958651653, -16.88279759715859640 ) ) ;
#13779 = CARTESIAN_POINT ( 'NONE',  ( 15.07084970125951884, 25.38295622438022647, -9.715434860296623398 ) ) ;
#13780 = CARTESIAN_POINT ( 'NONE',  ( 16.84128903688015200, 12.06818854907147021, -26.60985204580989105 ) ) ;
#13781 = DIRECTION ( 'NONE',  ( 0.000000000000000000, 0.000000000000000000, 1.000000000000000000 ) ) ;
#13782 = CARTESIAN_POINT ( 'NONE',  ( -23.74914942275198371, -8.582573258223684221, 20.99999999999999645 ) ) ;
#13783 = ORIENTED_EDGE ( 'NONE', *, *, #34955, .T. ) ;
#13784 = CARTESIAN_POINT ( 'NONE',  ( -8.090184229333063470, 34.30791569506543226, -9.788502965324324734 ) ) ;
#13785 = ORIENTED_EDGE ( 'NONE', *, *, #12462, .T. ) ;
#13786 = CARTESIAN_POINT ( 'NONE',  ( -10.71251757019364348, -20.01999408326420493, -21.63251431787718460 ) ) ;
#13787 = CARTESIAN_POINT ( 'NONE',  ( 21.39877161664088590, 15.54711762656346075, 7.000000000000000000 ) ) ;
#13788 = ORIENTED_EDGE ( 'NONE', *, *, #5548, .T. ) ;
#13789 = LINE ( 'NONE', #26181, #36237 ) ;
#13790 = AXIS2_PLACEMENT_3D ( 'NONE', #29687, #5497, #10806 ) ;
#13791 = CARTESIAN_POINT ( 'NONE',  ( -7.309360666678539786, 9.887575703124607429, 7.000000000000000000 ) ) ;
#13792 = EDGE_LOOP ( 'NONE', ( #18991, #7159, #13783 ) ) ;
#13793 = CARTESIAN_POINT ( 'NONE',  ( -24.51383308242704118, 0.5270737306155055535, -18.46259585337534403 ) ) ;
#13794 = ORIENTED_EDGE ( 'NONE', *, *, #26745, .F. ) ;
#13795 = CARTESIAN_POINT ( 'NONE',  ( 34.31841886132467323, -8.208541541968717326, -8.495077349752200746 ) ) ;
#13796 = VECTOR ( 'NONE', #16285, 1000.000000000000000 ) ;
#13797 = ORIENTED_EDGE ( 'NONE', *, *, #35945, .T. ) ;
#13798 = DIRECTION ( 'NONE',  ( 0.000000000000000000, 0.000000000000000000, 1.000000000000000000 ) ) ;
#13799 = CARTESIAN_POINT ( 'NONE',  ( -16.82090372984274396, 29.19711159930251299, 10.99999999999915090 ) ) ;
#13800 = ADVANCED_FACE ( 'NONE', ( #4436 ), #16635, .F. ) ;
#13801 = DIRECTION ( 'NONE',  ( 0.000000000000000000, 0.000000000000000000, -1.000000000000000000 ) ) ;
#13802 = DIRECTION ( 'NONE',  ( -0.1045284632676563991, -0.9945218953682730678, 0.000000000000000000 ) ) ;
#13803 = CARTESIAN_POINT ( 'NONE',  ( 5.791386747369449139, 35.03736185296642702, 18.42518152272108622 ) ) ;
#13804 = DIRECTION ( 'NONE',  ( -0.5877852522924690293, 0.8090169943749503378, 0.000000000000000000 ) ) ;
#13805 = EDGE_LOOP ( 'NONE', ( #3574, #28919 ) ) ;
#13806 = CARTESIAN_POINT ( 'NONE',  ( -17.78456945130773192, -10.21696681478616497, -30.00000000000002487 ) ) ;
#13807 = CARTESIAN_POINT ( 'NONE',  ( 19.48557158514997667, 33.74999999999982236, 7.000000000000000000 ) ) ;
#13808 = CARTESIAN_POINT ( 'NONE',  ( 13.49038105676655164, 15.86602540378438064, 10.50000000000000178 ) ) ;
#13809 = CARTESIAN_POINT ( 'NONE',  ( 14.79081071437772010, 14.21365739191439737, -30.00000000000000711 ) ) ;
#13810 = CIRCLE ( 'NONE', #13140, 0.5000000000000000000 ) ;
#13811 = CARTESIAN_POINT ( 'NONE',  ( 7.223745109598073810, 25.00395250381602708, -18.84027392568900083 ) ) ;
#13812 = ORIENTED_EDGE ( 'NONE', *, *, #17114, .T. ) ;
#13813 = DIRECTION ( 'NONE',  ( -1.000000000000000000, 0.000000000000000000, 0.000000000000000000 ) ) ;
#13814 = CARTESIAN_POINT ( 'NONE',  ( -1.000000000000000000, 37.00000000000000711, 7.000000000000000000 ) ) ;
#13815 = CARTESIAN_POINT ( 'NONE',  ( 15.60062348926549092, -25.63540424016351338, -10.59428648563043041 ) ) ;
#13816 = CARTESIAN_POINT ( 'NONE',  ( 37.57549957648898697, 32.94422479542058824, 0.000000000000000000 ) ) ;
#13817 = LINE ( 'NONE', #14021, #406 ) ;
#13818 = ADVANCED_FACE ( 'NONE', ( #25959 ), #22711, .F. ) ;
#13819 = ORIENTED_EDGE ( 'NONE', *, *, #18917, .T. ) ;
#13820 = CARTESIAN_POINT ( 'NONE',  ( -11.18155517836364510, 17.75836668469307611, -26.22458058910422452 ) ) ;
#13821 = CARTESIAN_POINT ( 'NONE',  ( -28.49608467062484252, -24.01994641533374519, 16.87380292611445043 ) ) ;
#13822 = CARTESIAN_POINT ( 'NONE',  ( 9.315390879746241026, -18.48740755290666371, -27.46912605503104032 ) ) ;
#13823 = EDGE_CURVE ( 'NONE', #28074, #35813, #991, .T. ) ;
#13824 = EDGE_CURVE ( 'NONE', #28327, #23396, #22786, .T. ) ;
#13825 = CARTESIAN_POINT ( 'NONE',  ( -10.44103466624267185, 32.57396620494226624, 7.000000000000000000 ) ) ;
#13826 = ORIENTED_EDGE ( 'NONE', *, *, #29165, .F. ) ;
#13827 = ORIENTED_EDGE ( 'NONE', *, *, #14570, .F. ) ;
#13828 = CARTESIAN_POINT ( 'NONE',  ( -13.46828150710210892, 29.48665142929467819, -9.082731696040140079 ) ) ;
#13829 = DIRECTION ( 'NONE',  ( -1.000000000000000000, 0.000000000000000000, 0.000000000000000000 ) ) ;
#13830 = AXIS2_PLACEMENT_3D ( 'NONE', #12517, #19404, #31595 ) ;
#13831 = CARTESIAN_POINT ( 'NONE',  ( -0.2655091840902661926, 8.754836972118123839, 13.00000000000000178 ) ) ;
#13832 = EDGE_CURVE ( 'NONE', #29063, #29833, #37546, .T. ) ;
#13833 = CARTESIAN_POINT ( 'NONE',  ( -31.63542238863247036, -6.840584483190602860, -12.12705934607019209 ) ) ;
#13834 = FACE_OUTER_BOUND ( 'NONE', #1558, .T. ) ;
#13835 = VERTEX_POINT ( 'NONE', #29220 ) ;
#13836 = CARTESIAN_POINT ( 'NONE',  ( 25.11743899329887952, 0.5542468427327318370, -17.45589780009234104 ) ) ;
#13837 = PLANE ( 'NONE',  #25804 ) ;
#13838 = DIRECTION ( 'NONE',  ( 0.4067366430757889395, -0.9135454576426058626, 0.000000000000000000 ) ) ;
#13839 = DIRECTION ( 'NONE',  ( -0.9945218953682742891, -0.1045284632676437425, 0.000000000000000000 ) ) ;
#13840 = VECTOR ( 'NONE', #5955, 1000.000000000000000 ) ;
#13841 = VERTEX_POINT ( 'NONE', #4637 ) ;
#13842 = CARTESIAN_POINT ( 'NONE',  ( -30.48479298233587542, -0.01179609685226120329, -7.827771219771337385 ) ) ;
#13843 = DIRECTION ( 'NONE',  ( 1.000000000000000000, 0.000000000000000000, 0.000000000000000000 ) ) ;
#13844 = ORIENTED_EDGE ( 'NONE', *, *, #36602, .F. ) ;
#13845 = CARTESIAN_POINT ( 'NONE',  ( 23.19615353721358630, -1.261022845598870790, -21.37482308967549827 ) ) ;
#13846 = AXIS2_PLACEMENT_3D ( 'NONE', #10980, #35155, #13614 ) ;
#13847 = CARTESIAN_POINT ( 'NONE',  ( 12.11939247953937659, 16.54781379207330971, -30.00000000000001066 ) ) ;
#13848 = CARTESIAN_POINT ( 'NONE',  ( 36.20842572154669625, -9.127542156327942635, 15.13084544680213561 ) ) ;
#13849 = VERTEX_POINT ( 'NONE', #1390 ) ;
#13850 = PRESENTATION_LAYER_ASSIGNMENT (  '', '', ( #17117 ) ) ;
#13851 = CARTESIAN_POINT ( 'NONE',  ( -14.63455391419436324, 30.27276177228403853, 15.72805884748933103 ) ) ;
#13852 = ADVANCED_FACE ( 'NONE', ( #10735 ), #23120, .F. ) ;
#13853 = CARTESIAN_POINT ( 'NONE',  ( 5.257622542056514803, -24.31502561551697283, 16.87380292611441845 ) ) ;
#13854 = EDGE_CURVE ( 'NONE', #6833, #27468, #12891, .T. ) ;
#13855 = DIRECTION ( 'NONE',  ( -0.000000000000000000, 0.000000000000000000, 1.000000000000000000 ) ) ;
#13856 = ADVANCED_FACE ( 'NONE', ( #29620 ), #7878, .F. ) ;
#13857 = CARTESIAN_POINT ( 'NONE',  ( 5.702284676859227019, 27.34092580698741060, 20.82122704794079837 ) ) ;
#13858 = AXIS2_PLACEMENT_3D ( 'NONE', #26193, #4464, #38586 ) ;
#13859 = FACE_OUTER_BOUND ( 'NONE', #27057, .T. ) ;
#13860 = FACE_OUTER_BOUND ( 'NONE', #23719, .T. ) ;
#13861 = B_SPLINE_CURVE_WITH_KNOTS ( 'NONE', 3,
 ( #8871, #39345, #24503, #2581, #39937, #8673 ),
 .UNSPECIFIED., .F., .F.,
 ( 4, 2, 4 ),
 ( 0.000000000000000000, 0.5000000000000000000, 1.000000000000000000 ),
 .UNSPECIFIED. ) ;
#13862 = CARTESIAN_POINT ( 'NONE',  ( 5.000626697282971378, 37.74343557191168941, -5.437187664831800937 ) ) ;
#13863 = CARTESIAN_POINT ( 'NONE',  ( -12.80736835487442349, 15.68301270189233954, 7.000000000000000000 ) ) ;
#13864 = AXIS2_PLACEMENT_3D ( 'NONE', #13863, #11223, #7764 ) ;
#13865 = CARTESIAN_POINT ( 'NONE',  ( 11.83264664766892338, 25.78892025140200417, 19.27171037444156454 ) ) ;
#13866 = CARTESIAN_POINT ( 'NONE',  ( -20.67876391171101247, 10.11988510684650677, -15.94128652130671142 ) ) ;
#13867 = CARTESIAN_POINT ( 'NONE',  ( 13.30843957427272173, -15.68464343207989842, -28.55404288184102768 ) ) ;
#13868 = CARTESIAN_POINT ( 'NONE',  ( -13.63581098909220302, 27.45627467658446719, 11.00000000000000000 ) ) ;
#13869 = CARTESIAN_POINT ( 'NONE',  ( -13.20348688925211178, 15.99217894729804534, 10.49999999999999822 ) ) ;
#13870 = EDGE_CURVE ( 'NONE', #38519, #10872, #23309, .T. ) ;
#13871 = CARTESIAN_POINT ( 'NONE',  ( 13.98483810825139528, 24.04469065075334910, -13.50292141766080967 ) ) ;
#13872 = AXIS2_PLACEMENT_3D ( 'NONE', #32259, #35910, #10517 ) ;
#13873 = VERTEX_POINT ( 'NONE', #4025 ) ;
#13874 = CARTESIAN_POINT ( 'NONE',  ( -15.68533655378858249, 25.84264350341399208, -5.474052038806747511 ) ) ;
#13875 = CARTESIAN_POINT ( 'NONE',  ( -31.26284659378214670, -14.97710070420562367, 19.27171037444154322 ) ) ;
#13876 = EDGE_CURVE ( 'NONE', #39039, #26584, #16426, .T. ) ;
#13877 = PRODUCT_DEFINITION_FORMATION_WITH_SPECIFIED_SOURCE ( 'ANY', '', #3190, .NOT_KNOWN. ) ;
#13878 = CARTESIAN_POINT ( 'NONE',  ( 3.713592597587160871, 7.966960743906808418, 7.499999999999990230 ) ) ;
#13879 = CARTESIAN_POINT ( 'NONE',  ( 13.52166927499705018, 22.75664420946326771, -15.45479374845303866 ) ) ;
#13880 = ORIENTED_EDGE ( 'NONE', *, *, #21435, .T. ) ;
#13881 = CARTESIAN_POINT ( 'NONE',  ( 33.18780228327651827, -18.30041771095959291, -7.544762919428389836 ) ) ;
#13882 = ORIENTED_EDGE ( 'NONE', *, *, #842, .T. ) ;
#13884 = DIRECTION ( 'NONE',  ( 0.000000000000000000, 0.000000000000000000, 1.000000000000000000 ) ) ;
#13883 = CARTESIAN_POINT ( 'NONE',  ( -15.27795965409528556, 27.25395738312943195, -5.471917110302146448 ) ) ;
#13885 = CARTESIAN_POINT ( 'NONE',  ( -14.35348050961883182, -24.20068026153264640, -13.45728683335227771 ) ) ;
#13886 = DIRECTION ( 'NONE',  ( 0.000000000000000000, 0.000000000000000000, 1.000000000000000000 ) ) ;
#13887 = VECTOR ( 'NONE', #7245, 1000.000000000000000 ) ;
#13888 = ORIENTED_EDGE ( 'NONE', *, *, #26921, .F. ) ;
#13889 = CARTESIAN_POINT ( 'NONE',  ( -35.09971422896161641, -14.51120324735615874, -5.860585196400803554 ) ) ;
#13890 = CARTESIAN_POINT ( 'NONE',  ( -14.14189504131334374, -25.53275775165994332, -10.19155952056719450 ) ) ;
#13891 = CARTESIAN_POINT ( 'NONE',  ( 3.853166178176219425, 23.42705098312512746, 13.00000000000000178 ) ) ;
#13892 = CARTESIAN_POINT ( 'NONE',  ( 14.88675176583543802, 17.17549405809297269, -19.86810751864282309 ) ) ;
#13893 = ORIENTED_EDGE ( 'NONE', *, *, #34978, .T. ) ;
#13894 = CARTESIAN_POINT ( 'NONE',  ( 20.15589419559134754, 3.806103299124593775, -29.39287895154624763 ) ) ;
#13895 = DIRECTION ( 'NONE',  ( 0.5000000000000038858, 0.8660254037844363761, -0.000000000000000000 ) ) ;
#13896 = CARTESIAN_POINT ( 'NONE',  ( -13.87104230352201917, 20.53934056656885687, 7.500000000000004441 ) ) ;
#13897 = ORIENTED_EDGE ( 'NONE', *, *, #10143, .T. ) ;
#13898 = CARTESIAN_POINT ( 'NONE',  ( -20.62390181444667547, 0.5954859409029100714, -28.06474670757336654 ) ) ;
#13899 = CARTESIAN_POINT ( 'NONE',  ( 29.47994304646902108, -0.6169278861223216337, -11.53523241178914560 ) ) ;
#13900 = AXIS2_PLACEMENT_3D ( 'NONE', #16623, #19654, #19453 ) ;
#13901 = CARTESIAN_POINT ( 'NONE',  ( 32.41210168510363587, -9.609370058583692753, 18.87996532025784191 ) ) ;
#13902 = VERTEX_POINT ( 'NONE', #10330 ) ;
#13903 = CARTESIAN_POINT ( 'NONE',  ( -28.39096675370102574, 2.624765294898354195, -5.948919365530221270 ) ) ;
#13904 = CARTESIAN_POINT ( 'NONE',  ( 6.155076441694339096, 21.71698211341367468, -20.11584339644708308 ) ) ;
#13905 = VECTOR ( 'NONE', #14062, 1000.000000000000114 ) ;
#13906 = DIRECTION ( 'NONE',  ( 0.000000000000000000, 0.000000000000000000, 1.000000000000000000 ) ) ;
#13907 = PLANE ( 'NONE',  #34283 ) ;
#13908 = VECTOR ( 'NONE', #1628, 1000.000000000000000 ) ;
#13909 = LINE ( 'NONE', #1932, #19476 ) ;
#13910 = CARTESIAN_POINT ( 'NONE',  ( 6.407695755496777501, 35.66262363504857547, 11.00000000000000000 ) ) ;
#13911 = DIRECTION ( 'NONE',  ( 0.000000000000000000, 0.000000000000000000, 1.000000000000000000 ) ) ;
#13912 = ORIENTED_EDGE ( 'NONE', *, *, #1153, .T. ) ;
#13913 = DIRECTION ( 'NONE',  ( -1.000000000000000000, 0.000000000000000000, 0.000000000000000000 ) ) ;
#13914 = FACE_OUTER_BOUND ( 'NONE', #8586, .T. ) ;
#13915 = CARTESIAN_POINT ( 'NONE',  ( 26.60044679873302442, -24.57989799457884672, -8.454375987971554096 ) ) ;
#13916 = DIRECTION ( 'NONE',  ( -0.000000000000000000, -0.000000000000000000, -1.000000000000000000 ) ) ;
#13917 = DIRECTION ( 'NONE',  ( -0.7032331762534058672, -0.07391278520355742954, -0.7071067811865467956 ) ) ;
#13918 = CARTESIAN_POINT ( 'NONE',  ( 10.70408546242706826, 17.89813097114894447, -26.79091869943797377 ) ) ;
#13919 = SURFACE_STYLE_FILL_AREA ( #38706 ) ;
#13920 = ORIENTED_EDGE ( 'NONE', *, *, #18962, .T. ) ;
#13921 = CARTESIAN_POINT ( 'NONE',  ( -16.36974882123188024, 17.56213386315149805, -15.79138196246351100 ) ) ;
#13922 = CARTESIAN_POINT ( 'NONE',  ( -24.42249458671265927, -8.161411852468820172, 20.99999999999995026 ) ) ;
#13923 = CARTESIAN_POINT ( 'NONE',  ( 14.51912842374987456, -25.44048832947288474, -10.65547803431773843 ) ) ;
#13924 = DIRECTION ( 'NONE',  ( 0.000000000000000000, 0.000000000000000000, 1.000000000000000000 ) ) ;
#13925 = CARTESIAN_POINT ( 'NONE',  ( 14.94650803745857459, 25.76355683451345868, -9.709532534900402467 ) ) ;
#13926 = ORIENTED_EDGE ( 'NONE', *, *, #19107, .T. ) ;
#13927 = CARTESIAN_POINT ( 'NONE',  ( 11.06383671253727563, 17.50867094151858794, -27.44708461513057074 ) ) ;
#13928 = ORIENTED_EDGE ( 'NONE', *, *, #31238, .F. ) ;
#13929 = CARTESIAN_POINT ( 'NONE',  ( -15.38296630468078874, 26.90060637120896558, -5.000000000000001776 ) ) ;
#13930 = CARTESIAN_POINT ( 'NONE',  ( -15.47550425816466380, -26.73936689671932143, -5.474270598677144939 ) ) ;
#13931 = CARTESIAN_POINT ( 'NONE',  ( -33.69589222704896514, -0.03122585499738908532, 11.55979286843900233 ) ) ;
#13932 = AXIS2_PLACEMENT_3D ( 'NONE', #10129, #34513, #32060 ) ;
#13933 = CARTESIAN_POINT ( 'NONE',  ( -27.79669695867223211, -16.79236872055855301, -13.80438657369478683 ) ) ;
#13934 = CARTESIAN_POINT ( 'NONE',  ( -6.603877609327104103, -24.16432772825694641, -11.80673248872152037 ) ) ;
#13935 = CARTESIAN_POINT ( 'NONE',  ( 11.70877560076256962, 16.87668805158687491, -28.73501782286896855 ) ) ;
#13936 = ORIENTED_EDGE ( 'NONE', *, *, #10619, .F. ) ;
#13937 = CARTESIAN_POINT ( 'NONE',  ( 19.63124566570902019, 8.197596596637488631, -23.30003740157314951 ) ) ;
#13938 = DIRECTION ( 'NONE',  ( 1.000000000000000000, 0.000000000000000000, 0.000000000000000000 ) ) ;
#13939 = CARTESIAN_POINT ( 'NONE',  ( -10.33795143809923545, 20.40792924032147226, 10.49999999999999467 ) ) ;
#13940 = CARTESIAN_POINT ( 'NONE',  ( 2.362621116368220697, 8.178251995481296888, 10.83333333333333037 ) ) ;
#13941 = CONICAL_SURFACE ( 'NONE', #32122, 1.000000000000007772, 0.7853981633974560506 ) ;
#13942 = ORIENTED_EDGE ( 'NONE', *, *, #32878, .F. ) ;
#13943 = CARTESIAN_POINT ( 'NONE',  ( -32.13550794386147658, -2.443358523703948570, -8.649088748501414514 ) ) ;
#13944 = CIRCLE ( 'NONE', #14615, 57.00000000000006395 ) ;
#13945 = CARTESIAN_POINT ( 'NONE',  ( -16.32868373051740818, 2.489249428719812585, 20.94377226548377635 ) ) ;
#13946 = ORIENTED_EDGE ( 'NONE', *, *, #22554, .T. ) ;
#13947 = CARTESIAN_POINT ( 'NONE',  ( 23.79772124597061733, -17.36195373897592020, 20.82122704794065626 ) ) ;
#13948 = LINE ( 'NONE', #1978, #2491 ) ;
#13949 = CARTESIAN_POINT ( 'NONE',  ( 3.118671991557230516, 37.17221401100731981, 12.00000000000000000 ) ) ;
#13950 = CARTESIAN_POINT ( 'NONE',  ( 27.23312197222509923, -12.91592730962168112, -15.69032973555321853 ) ) ;
#13951 = CARTESIAN_POINT ( 'NONE',  ( 29.88800841290863630, -25.99212743943143167, 12.14047268033086624 ) ) ;
#13952 = EDGE_CURVE ( 'NONE', #3918, #32089, #38789, .T. ) ;
#13953 = ORIENTED_EDGE ( 'NONE', *, *, #25058, .T. ) ;
#13954 = DIRECTION ( 'NONE',  ( 0.000000000000000000, -0.6216356077939594327, -0.7833065626704749373 ) ) ;
#13955 = DIRECTION ( 'NONE',  ( -5.095851118916442708E-15, -0.7071067811865500152, -0.7071067811865451302 ) ) ;
#13956 = CIRCLE ( 'NONE', #22383, 6.000000000000000000 ) ;
#13957 = CARTESIAN_POINT ( 'NONE',  ( 0.000000000000000000, 22.50000000000000355, 7.000000000000000000 ) ) ;
#13958 = DIRECTION ( 'NONE',  ( 1.000000000000000000, 0.000000000000000000, 0.000000000000000000 ) ) ;
#13959 = EDGE_CURVE ( 'NONE', #17177, #12432, #12911, .T. ) ;
#13960 = CARTESIAN_POINT ( 'NONE',  ( -1.011306241801402273, 20.48440008317826511, -30.00000000000000711 ) ) ;
#13961 = FACE_OUTER_BOUND ( 'NONE', #8865, .T. ) ;
#13962 = CARTESIAN_POINT ( 'NONE',  ( 13.63581098909226519, 27.45627467658428600, 11.00000000000000000 ) ) ;
#13963 = EDGE_CURVE ( 'NONE', #2398, #6680, #38209, .T. ) ;
#13964 = AXIS2_PLACEMENT_3D ( 'NONE', #12670, #36864, #18774 ) ;
#13965 = DIRECTION ( 'NONE',  ( 1.000000000000000000, 0.000000000000000000, 0.000000000000000000 ) ) ;
#13966 = DIRECTION ( 'NONE',  ( 1.000000000000000000, 0.000000000000000000, 0.000000000000000000 ) ) ;
#13967 = DIRECTION ( 'NONE',  ( 1.000000000000000000, 0.000000000000000000, 0.000000000000000000 ) ) ;
#13968 = CARTESIAN_POINT ( 'NONE',  ( 12.42842755122037346, 24.68749237541469910, -15.24760426189488172 ) ) ;
#13969 = CARTESIAN_POINT ( 'NONE',  ( -12.30736835487443415, 14.81698729810790560, 11.00000000000000000 ) ) ;
#13970 = ORIENTED_EDGE ( 'NONE', *, *, #4916, .F. ) ;
#13973 = CARTESIAN_POINT ( 'NONE',  ( 9.677076426724163127, 26.69573495723207657, 10.50000000000000533 ) ) ;
#13972 = AXIS2_PLACEMENT_3D ( 'NONE', #5, #34527, #3443 ) ;
#13971 = CARTESIAN_POINT ( 'NONE',  ( -19.17049849529148986, 13.78076537144805513, -13.89096179552466914 ) ) ;
#13974 = LINE ( 'NONE', #32678, #21795 ) ;
#13975 = CARTESIAN_POINT ( 'NONE',  ( 15.50471485482113820, -26.74686345152265332, -5.474125567124247027 ) ) ;
#13976 = LINE ( 'NONE', #35919, #34061 ) ;
#13977 = CARTESIAN_POINT ( 'NONE',  ( 13.19104420233710506, 22.26977043259612188, -16.43980447468807782 ) ) ;
#13978 = CARTESIAN_POINT ( 'NONE',  ( -27.08779848459120743, 7.221796966026721165, -5.000000000000006217 ) ) ;
#13979 = CARTESIAN_POINT ( 'NONE',  ( 2.494936919103933448, 34.23777120880591696, 12.00000000000000000 ) ) ;
#13980 = CARTESIAN_POINT ( 'NONE',  ( -22.89426894111359090, -21.54803994364075237, -13.90284137355498828 ) ) ;
#13981 = CARTESIAN_POINT ( 'NONE',  ( 4.259257232841775043, -20.22332097882593516, -27.12113025733162530 ) ) ;
#13982 = CARTESIAN_POINT ( 'NONE',  ( 11.21461197269842636, 17.30895135427360287, -28.08770296027252655 ) ) ;
#13983 = CARTESIAN_POINT ( 'NONE',  ( 20.99822950558156620, 12.93985014994555094, -7.428410497112117206 ) ) ;
#13984 = EDGE_CURVE ( 'NONE', #36229, #31697, #30068, .T. ) ;
#13985 = LINE ( 'NONE', #4643, #18017 ) ;
#13986 = ADVANCED_FACE ( 'NONE', ( #26978 ), #5633, .F. ) ;
#13987 = ORIENTED_EDGE ( 'NONE', *, *, #24933, .T. ) ;
#13988 = CARTESIAN_POINT ( 'NONE',  ( -5.449788316150806722, 31.42540188369694931, -13.85748977810616545 ) ) ;
#13989 = ORIENTED_EDGE ( 'NONE', *, *, #3692, .F. ) ;
#13990 = CARTESIAN_POINT ( 'NONE',  ( 7.096882951594523981, 29.56287847632726695, 10.49999999999999645 ) ) ;
#13991 = ORIENTED_EDGE ( 'NONE', *, *, #32821, .T. ) ;
#13992 = CARTESIAN_POINT ( 'NONE',  ( 12.74038105676654453, 14.56698729810772264, 7.000000000000000000 ) ) ;
#13993 = LINE ( 'NONE', #17463, #23892 ) ;
#13994 = VERTEX_POINT ( 'NONE', #27574 ) ;
#13995 = VECTOR ( 'NONE', #4121, 1000.000000000000000 ) ;
#13996 = CARTESIAN_POINT ( 'NONE',  ( -30.79543237407852985, 0.06882123448304010294, -4.999999999999999112 ) ) ;
#13997 = ORIENTED_EDGE ( 'NONE', *, *, #30912, .T. ) ;
#13998 = CARTESIAN_POINT ( 'NONE',  ( 26.15862945001307338, -7.884392761838899588, -17.73711950188741682 ) ) ;
#13999 = VECTOR ( 'NONE', #16626, 1000.000000000000227 ) ;
#14000 = AXIS2_PLACEMENT_3D ( 'NONE', #9287, #37716, #6032 ) ;
#14001 = ORIENTED_EDGE ( 'NONE', *, *, #16587, .T. ) ;
#14002 = CARTESIAN_POINT ( 'NONE',  ( -10.06946225350398372, 32.23940090176283491, 7.500000000000005329 ) ) ;
#14003 = VERTEX_POINT ( 'NONE', #18241 ) ;
#14004 = CARTESIAN_POINT ( 'NONE',  ( 11.44473057578109199, 31.45924896672603310, 9.500000000000000000 ) ) ;
#14005 = LINE ( 'NONE', #19906, #16897 ) ;
#14006 = EDGE_CURVE ( 'NONE', #11050, #18136, #23930, .T. ) ;
#14007 = CARTESIAN_POINT ( 'NONE',  ( 8.686999124429359398, 33.93090424204713429, 17.92354375535250810 ) ) ;
#14008 = DIRECTION ( 'NONE',  ( -0.7431448254773846962, 0.6691306063588690067, 0.000000000000000000 ) ) ;
#14009 = VERTEX_POINT ( 'NONE', #36326 ) ;
#14010 = SURFACE_STYLE_USAGE ( .BOTH. , #28847 ) ;
#14011 = CARTESIAN_POINT ( 'NONE',  ( 3.211395437248501850, 12.61633075744433796, 12.00000000000000000 ) ) ;
#14012 = CARTESIAN_POINT ( 'NONE',  ( 3.476901250629512941, 26.36149378532653031, 13.00000000000000178 ) ) ;
#14013 = DIRECTION ( 'NONE',  ( -0.000000000000000000, -0.000000000000000000, -1.000000000000000000 ) ) ;
#14014 = CARTESIAN_POINT ( 'NONE',  ( 16.55956259488248961, 15.35177602386088402, -18.95873336413509946 ) ) ;
#14015 = CARTESIAN_POINT ( 'NONE',  ( 10.66400708477075199, 33.33867412272209663, -8.508697681493581300 ) ) ;
#14016 = VERTEX_POINT ( 'NONE', #36727 ) ;
#14017 = CARTESIAN_POINT ( 'NONE',  ( 10.44103466624280685, 32.57396620494213124, 7.499999999999997335 ) ) ;
#14018 = CYLINDRICAL_SURFACE ( 'NONE', #17524, 0.5000000000000004441 ) ;
#14019 = CARTESIAN_POINT ( 'NONE',  ( 15.84172312148188944, -26.62845490554297001, -7.344013408899289885 ) ) ;
#14020 = CARTESIAN_POINT ( 'NONE',  ( 16.80389827882015297, -21.64427909825937135, 19.99202127657103389 ) ) ;
#14021 = CARTESIAN_POINT ( 'NONE',  ( -7.559512017365658920, 19.71884705062586107, 6.000000000000000000 ) ) ;
#14022 = ORIENTED_EDGE ( 'NONE', *, *, #22281, .F. ) ;
#14023 = CARTESIAN_POINT ( 'NONE',  ( -10.98473797697927701, 17.30853926952405075, -29.99999999999999289 ) ) ;
#14024 = CONICAL_SURFACE ( 'NONE', #13383, 1.000000000000007772, 0.7853981633974554954 ) ;
#14025 = CARTESIAN_POINT ( 'NONE',  ( -28.76760616114084712, -24.40467509901190724, 16.30093088680195379 ) ) ;
#14026 = CARTESIAN_POINT ( 'NONE',  ( 14.83010314187407275, -26.50386704626997414, -6.417717416243527317 ) ) ;
#14027 = EDGE_CURVE ( 'NONE', #26803, #11791, #20889, .T. ) ;
#14028 = CARTESIAN_POINT ( 'NONE',  ( 1.265502442671760264, 36.24516302788250499, 12.00000000000000000 ) ) ;
#14029 = ADVANCED_FACE ( 'NONE', ( #8081 ), #33291, .F. ) ;
#14030 = ORIENTED_EDGE ( 'NONE', *, *, #19454, .T. ) ;
#14031 = ORIENTED_EDGE ( 'NONE', *, *, #18718, .F. ) ;
#14032 = CARTESIAN_POINT ( 'NONE',  ( -7.785723730699082523, 19.30973503573152072, -27.21076142849720370 ) ) ;
#14033 = CARTESIAN_POINT ( 'NONE',  ( 14.99905852611806267, 22.33194247983193392, 7.000000000000000000 ) ) ;
#14034 = FACE_BOUND ( 'NONE', #39026, .T. ) ;
#14035 = CARTESIAN_POINT ( 'NONE',  ( -24.35358919934762412, -5.258831719696673623, -19.92280915639523187 ) ) ;
#14036 = DIRECTION ( 'NONE',  ( 1.000000000000000000, 0.000000000000000000, 0.000000000000000000 ) ) ;
#14037 = EDGE_LOOP ( 'NONE', ( #33094, #17193, #22632, #1459, #9380 ) ) ;
#14038 = CARTESIAN_POINT ( 'NONE',  ( 22.71450242014743637, 0.6646934032305609197, -21.62413034359709485 ) ) ;
#14039 = CARTESIAN_POINT ( 'NONE',  ( -12.79957064613986084, -17.39491786099972259, -24.68155699886624177 ) ) ;
#14040 = FACE_OUTER_BOUND ( 'NONE', #38508, .T. ) ;
#14041 = DIRECTION ( 'NONE',  ( -0.4067366430757888285, 0.9135454576426059736, -0.000000000000000000 ) ) ;
#14042 = ORIENTED_EDGE ( 'NONE', *, *, #35746, .F. ) ;
#14043 = CARTESIAN_POINT ( 'NONE',  ( -30.73544637638549659, -0.04073673089017386395, -6.887548030490833639 ) ) ;
#14044 = FACE_OUTER_BOUND ( 'NONE', #16655, .T. ) ;
#14045 = VERTEX_POINT ( 'NONE', #20491 ) ;
#14046 = CARTESIAN_POINT ( 'NONE',  ( 33.03334970784698044, -3.164777106519510497, -7.267418744076269199 ) ) ;
#14047 = CARTESIAN_POINT ( 'NONE',  ( 36.66879582113919867, -12.81605961719004760, 14.53008259254017709 ) ) ;
#14048 = ORIENTED_EDGE ( 'NONE', *, *, #31159, .T. ) ;
#14049 = CARTESIAN_POINT ( 'NONE',  ( 10.19952947927959030, 35.92118758406570578, 15.13084544680213739 ) ) ;
#14050 = CARTESIAN_POINT ( 'NONE',  ( -16.41753675002347279, -23.14183271658003349, 19.27171037444156809 ) ) ;
#14051 = CARTESIAN_POINT ( 'NONE',  ( -3.835137251120299684, 29.44922644035488446, 12.00000000000000000 ) ) ;
#14052 = EDGE_CURVE ( 'NONE', #22956, #18136, #18043, .T. ) ;
#14053 = CARTESIAN_POINT ( 'NONE',  ( 0.8947151973524753998, 30.76432767446200245, 20.69868183039781329 ) ) ;
#14054 = AXIS2_PLACEMENT_3D ( 'NONE', #19778, #13676, #26064 ) ;
#14055 = CARTESIAN_POINT ( 'NONE',  ( 9.917734535019443243, 14.47043272369397116, 12.00000000000000000 ) ) ;
#14056 = VERTEX_POINT ( 'NONE', #11939 ) ;
#14057 = CYLINDRICAL_SURFACE ( 'NONE', #27328, 1.000000000000000888 ) ;
#14058 = CARTESIAN_POINT ( 'NONE',  ( 2.056640691923212305, 20.39672081104026802, -29.21734360554237497 ) ) ;
#14059 = DIRECTION ( 'NONE',  ( -0.4067366430757891060, 0.9135454576426058626, 0.000000000000000000 ) ) ;
#14060 = CARTESIAN_POINT ( 'NONE',  ( 14.01880647360106380, 20.72057097093389899, 18.87996532025600871 ) ) ;
#14061 = CARTESIAN_POINT ( 'NONE',  ( 14.01931971080170847, -19.72843696819627013, -20.19157926468732356 ) ) ;
#14062 = DIRECTION ( 'NONE',  ( -0.3090169943749448977, 0.9510565162951543083, -0.000000000000000000 ) ) ;
#14063 = CARTESIAN_POINT ( 'NONE',  ( 5.706335727061685681, 24.35410196624994583, 12.00000000000000000 ) ) ;
#14064 = DIRECTION ( 'NONE',  ( 1.000000000000000000, 0.000000000000000000, 0.000000000000000000 ) ) ;
#14065 = ORIENTED_EDGE ( 'NONE', *, *, #37203, .T. ) ;
#14066 = CARTESIAN_POINT ( 'NONE',  ( 15.05470115789045593, 26.29235278780934593, -8.760806541134785519 ) ) ;
#14067 = ORIENTED_EDGE ( 'NONE', *, *, #29147, .F. ) ;
#14068 = CARTESIAN_POINT ( 'NONE',  ( -15.51364032778053925, 26.43312886238355119, -5.000000000000002665 ) ) ;
#14069 = CARTESIAN_POINT ( 'NONE',  ( -30.28108141855295088, -11.05112898844792468, 19.99202127657160943 ) ) ;
#14070 = CARTESIAN_POINT ( 'NONE',  ( -14.38243823352021522, 26.25560849141445274, 10.49999999999999822 ) ) ;
#14071 = CARTESIAN_POINT ( 'NONE',  ( 15.45734228612143646, 26.63525802094401840, -5.474165804386270651 ) ) ;
#14072 = EDGE_LOOP ( 'NONE', ( #21933, #12005, #32209, #21489 ) ) ;
#14073 = CARTESIAN_POINT ( 'NONE',  ( 17.67655037483637415, -11.18511709101394302, -26.96765970948913349 ) ) ;
#14074 = ORIENTED_EDGE ( 'NONE', *, *, #3758, .T. ) ;
#14076 = DIRECTION ( 'NONE',  ( 0.000000000000000000, 0.000000000000000000, 1.000000000000000000 ) ) ;
#14075 = CARTESIAN_POINT ( 'NONE',  ( -13.21556436932873702, 23.35821163730123828, -15.38919888636536015 ) ) ;
#14077 = ADVANCED_FACE ( 'NONE', ( #17851 ), #32885, .T. ) ;
#14078 = CARTESIAN_POINT ( 'NONE',  ( -12.04589167603010758, -20.30227844483841437, -20.42902932149552342 ) ) ;
#14079 = CARTESIAN_POINT ( 'NONE',  ( 13.63396663385386454, 16.24580510161703728, 7.000000000000000000 ) ) ;
#14080 = EDGE_CURVE ( 'NONE', #28074, #10357, #18757, .T. ) ;
#14081 = AXIS2_PLACEMENT_3D ( 'NONE', #39917, #11703, #27337 ) ;
#14082 = VECTOR ( 'NONE', #39767, 999.9999999999998863 ) ;
#14083 = ORIENTED_EDGE ( 'NONE', *, *, #35845, .T. ) ;
#14084 = CARTESIAN_POINT ( 'NONE',  ( -34.84681707271400342, -13.17048057206591061, -7.565634217669577666 ) ) ;
#14085 = CARTESIAN_POINT ( 'NONE',  ( -14.68723827886567435, -26.16908770772800708, -8.301334212331063611 ) ) ;
#14086 = CARTESIAN_POINT ( 'NONE',  ( 39.59914439355151217, -10.88071517532262256, 22.99999999999999289 ) ) ;
#14087 = CARTESIAN_POINT ( 'NONE',  ( 17.18319281906964235, 20.94686736314969266, -7.387940685848898070 ) ) ;
#14088 = ORIENTED_EDGE ( 'NONE', *, *, #13100, .T. ) ;
#14089 = CARTESIAN_POINT ( 'NONE',  ( 20.15589419559134754, 3.806103299124593775, -30.00000000000000711 ) ) ;
#14090 = CARTESIAN_POINT ( 'NONE',  ( -8.412270287199616448, 10.07085245822954533, 10.59344459855563336 ) ) ;
#14091 = DIRECTION ( 'NONE',  ( 1.000000000000000000, 0.000000000000000000, 0.000000000000000000 ) ) ;
#14092 = AXIS2_PLACEMENT_3D ( 'NONE', #1812, #35739, #30449 ) ;
#14093 = VERTEX_POINT ( 'NONE', #24330 ) ;
#14094 = CARTESIAN_POINT ( 'NONE',  ( -30.88772949577154137, -0.1296325399160530301, -6.414922386148385058 ) ) ;
#14095 = CARTESIAN_POINT ( 'NONE',  ( 30.67843010612066834, -0.5310868340548599020, -8.737336165245711328 ) ) ;
#14096 = AXIS2_PLACEMENT_3D ( 'NONE', #19010, #15761, #36905 ) ;
#14097 = CARTESIAN_POINT ( 'NONE',  ( 30.77008022630325002, -17.76511410164234306, 18.87996532025784546 ) ) ;
#14098 = EDGE_LOOP ( 'NONE', ( #2023, #40114, #7821 ) ) ;
#14099 = CARTESIAN_POINT ( 'NONE',  ( -26.02750893215630512, 1.859127183977640652, -14.58313542125660689 ) ) ;
#14100 = CARTESIAN_POINT ( 'NONE',  ( -9.163310636333559245, 20.63632441393290762, -29.99999999999998579 ) ) ;
#14101 = EDGE_CURVE ( 'NONE', #35217, #10337, #33616, .T. ) ;
#14102 = LINE ( 'NONE', #29546, #34916 ) ;
#14103 = DIRECTION ( 'NONE',  ( 0.1045284632676569680, 0.9945218953682730678, -0.000000000000000000 ) ) ;
#14104 = ADVANCED_FACE ( 'NONE', ( #38858 ), #26661, .F. ) ;
#14105 = CIRCLE ( 'NONE', #31656, 0.9999999999999991118 ) ;
#14106 = EDGE_CURVE ( 'NONE', #17784, #3811, #15510, .T. ) ;
#14107 = DIRECTION ( 'NONE',  ( -0.000000000000000000, -0.000000000000000000, 1.000000000000000000 ) ) ;
#14108 = DIRECTION ( 'NONE',  ( -0.1045284632676437842, 0.9945218953682744001, 0.000000000000000000 ) ) ;
#14109 = DIRECTION ( 'NONE',  ( 0.000000000000000000, 1.000000000000000000, 0.000000000000000000 ) ) ;
#14110 = ORIENTED_EDGE ( 'NONE', *, *, #2715, .F. ) ;
#14111 = CARTESIAN_POINT ( 'NONE',  ( -20.93756045555672429, 5.794231368335179155, -22.09979801953191014 ) ) ;
#14112 = FACE_OUTER_BOUND ( 'NONE', #30120, .T. ) ;
#14113 = CARTESIAN_POINT ( 'NONE',  ( 2.118671991557230516, 37.17221401100731981, 13.00000000000000178 ) ) ;
#14114 = CARTESIAN_POINT ( 'NONE',  ( 15.88542612224667927, -12.95767258840383285, -30.00000000000000711 ) ) ;
#14115 = CIRCLE ( 'NONE', #35529, 1.000000000000000000 ) ;
#14116 = DIRECTION ( 'NONE',  ( -1.000000000000000000, 0.000000000000000000, 0.000000000000000000 ) ) ;
#14117 = CARTESIAN_POINT ( 'NONE',  ( -10.78894649379783388, 21.72623886970244911, 12.00000000000000000 ) ) ;
#14118 = CARTESIAN_POINT ( 'NONE',  ( 13.85193959438362121, 24.35802306960261632, -13.47368439763754289 ) ) ;
#14119 = CIRCLE ( 'NONE', #38131, 0.5000000000000000000 ) ;
#14120 = FACE_OUTER_BOUND ( 'NONE', #2738, .T. ) ;
#14121 = VERTEX_POINT ( 'NONE', #37707 ) ;
#14122 = CARTESIAN_POINT ( 'NONE',  ( -15.65588464930769597, 19.60408957237921612, -14.69554073304035668 ) ) ;
#14123 = CARTESIAN_POINT ( 'NONE',  ( -24.49951449059916442, -14.14480128616215282, 20.99999999999999645 ) ) ;
#14124 = CARTESIAN_POINT ( 'NONE',  ( 14.29363999704249366, -25.05931576210448952, -11.60082902445461706 ) ) ;
#14125 = DIRECTION ( 'NONE',  ( 1.000000000000000000, 0.000000000000000000, 0.000000000000000000 ) ) ;
#14126 = CARTESIAN_POINT ( 'NONE',  ( 13.21981074911866649, 22.21720586980774925, -16.44568224045854166 ) ) ;
#14127 = ORIENTED_EDGE ( 'NONE', *, *, #7401, .T. ) ;
#14128 = CARTESIAN_POINT ( 'NONE',  ( 11.30648189521336633, 18.04080162384153496, -25.01410076809229110 ) ) ;
#14129 = VERTEX_POINT ( 'NONE', #20379 ) ;
#14131 = DIRECTION ( 'NONE',  ( -0.000000000000000000, -0.000000000000000000, 1.000000000000000000 ) ) ;
#14130 = CARTESIAN_POINT ( 'NONE',  ( -14.80676639301200126, 25.71291667989606466, -10.17396840098144750 ) ) ;
#14132 = EDGE_CURVE ( 'NONE', #31370, #21619, #4482, .T. ) ;
#14133 = CARTESIAN_POINT ( 'NONE',  ( -13.45451633981421757, -23.63114001665184816, -14.46875807778122081 ) ) ;
#14134 = CARTESIAN_POINT ( 'NONE',  ( -37.13148535761801838, -14.80270701502662511, 11.00000000000000000 ) ) ;
#14135 = EDGE_CURVE ( 'NONE', #22373, #7177, #9044, .T. ) ;
#14136 = CARTESIAN_POINT ( 'NONE',  ( -32.28394191823594639, -20.85172211888466620, -5.435695248426204884 ) ) ;
#14137 = CARTESIAN_POINT ( 'NONE',  ( -6.849675264061505509, -24.72308982460099003, -9.348409214434667547 ) ) ;
#14138 = CARTESIAN_POINT ( 'NONE',  ( 13.01345650832474199, 19.67229149937466204, -19.60135455124983395 ) ) ;
#14139 = ORIENTED_EDGE ( 'NONE', *, *, #10855, .F. ) ;
#14140 = CARTESIAN_POINT ( 'NONE',  ( 19.09486710253168695, 8.055642014369341908, -26.60153427135273674 ) ) ;
#14141 = DIRECTION ( 'NONE',  ( 0.000000000000000000, -0.7071067811865451302, -0.7071067811865500152 ) ) ;
#14142 = CYLINDRICAL_SURFACE ( 'NONE', #25095, 1.000000000000000000 ) ;
#14143 = CARTESIAN_POINT ( 'NONE',  ( -4.591666147298613332, 15.32946292166675306, 9.000000000000001776 ) ) ;
#14144 = CIRCLE ( 'NONE', #31649, 1.000000000000000000 ) ;
#14145 = ORIENTED_EDGE ( 'NONE', *, *, #37029, .T. ) ;
#14146 = CARTESIAN_POINT ( 'NONE',  ( -20.60443745909306301, -1.795035389764878309, -27.94510193186766145 ) ) ;
#14147 = VECTOR ( 'NONE', #17310, 1000.000000000000114 ) ;
#14148 = VECTOR ( 'NONE', #23243, 1000.000000000000000 ) ;
#14149 = CARTESIAN_POINT ( 'NONE',  ( -12.58275666885741195, 13.96078236988870280, 20.50957957746030758 ) ) ;
#14150 = CARTESIAN_POINT ( 'NONE',  ( 23.78345815580435385, -15.17947280105387442, 21.00000000000004619 ) ) ;
#14151 = DIRECTION ( 'NONE',  ( 0.4156269377774486906, -0.5720614028176846944, -0.7071067811865499042 ) ) ;
#14152 = DIRECTION ( 'NONE',  ( 1.000000000000000000, 0.000000000000000000, 0.000000000000000000 ) ) ;
#14153 = B_SPLINE_CURVE_WITH_KNOTS ( 'NONE', 3,
 ( #7212, #9687, #37708, #9872, #16174, #6808, #19214, #32007, #31602, #10074, #22454, #133, #28559, #32828, #7621, #4173, #23671, #20026 ),
 .UNSPECIFIED., .F., .F.,
 ( 4, 2, 2, 2, 2, 2, 2, 2, 4 ),
 ( 0.000000000000000000, 0.1250000000000000833, 0.2500000000000001665, 0.3750000000000002220, 0.5000000000000003331, 0.6250000000000004441, 0.7500000000000002220, 0.8750000000000001110, 1.000000000000000000 ),
 .UNSPECIFIED. ) ;
#14154 = CARTESIAN_POINT ( 'NONE',  ( 30.15216583608805934, -14.28728122224699071, -12.89820425123808256 ) ) ;
#14156 = VECTOR ( 'NONE', #6881, 1000.000000000000000 ) ;
#14155 = CARTESIAN_POINT ( 'NONE',  ( 3.503793317224329851, 8.420815634768676006, 7.000000000000000000 ) ) ;
#14157 = EDGE_CURVE ( 'NONE', #8090, #24274, #31601, .T. ) ;
#14158 = ORIENTED_EDGE ( 'NONE', *, *, #11585, .F. ) ;
#14159 = DIRECTION ( 'NONE',  ( 1.000000000000000000, 0.000000000000000000, 0.000000000000000000 ) ) ;
#14160 = VERTEX_POINT ( 'NONE', #22252 ) ;
#14161 = CARTESIAN_POINT ( 'NONE',  ( 0.3248095335732383848, 30.21040829111500869, -15.67845704928061323 ) ) ;
#14162 = DIRECTION ( 'NONE',  ( 1.000000000000000000, 0.000000000000000000, 0.000000000000000000 ) ) ;
#14163 = CARTESIAN_POINT ( 'NONE',  ( 13.76030399595649811, 27.49672490655773416, 11.00000000000000178 ) ) ;
#14164 = DIRECTION ( 'NONE',  ( 0.000000000000000000, 0.000000000000000000, 1.000000000000000000 ) ) ;
#14165 = DIRECTION ( 'NONE',  ( 0.000000000000000000, 0.000000000000000000, 1.000000000000000000 ) ) ;
#14166 = CARTESIAN_POINT ( 'NONE',  ( 12.30736835487432757, 14.81698729810772441, 7.000000000000000000 ) ) ;
#14167 = VECTOR ( 'NONE', #8254, 1000.000000000000000 ) ;
#14168 = CARTESIAN_POINT ( 'NONE',  ( 14.00903526708603053, 27.25070609806927280, -10.53950710942262425 ) ) ;
#14169 = CARTESIAN_POINT ( 'NONE',  ( 6.064564986133971658, 13.54338174056915456, 12.00000000000000000 ) ) ;
#14170 = AXIS2_PLACEMENT_3D ( 'NONE', #699, #35636, #25671 ) ;
#14171 = ORIENTED_EDGE ( 'NONE', *, *, #18794, .T. ) ;
#14173 = CARTESIAN_POINT ( 'NONE',  ( -6.557822374958138134, 35.99981354310120452, 11.00000000000000000 ) ) ;
#14172 = CARTESIAN_POINT ( 'NONE',  ( -16.80464701721349385, 11.74058409121013469, -30.00000000000000000 ) ) ;
#14174 = CARTESIAN_POINT ( 'NONE',  ( -2.485571585149885632, -11.24999999999987566, 6.000000000000000000 ) ) ;
#14175 = CARTESIAN_POINT ( 'NONE',  ( 11.21665055246841725, -20.46292137171589332, -20.53731539713322007 ) ) ;
#14176 = CYLINDRICAL_SURFACE ( 'NONE', #9413, 15.99999999999999645 ) ;
#14177 = CARTESIAN_POINT ( 'NONE',  ( 12.37323903880625764, 20.51431812958072953, -19.49257168437462440 ) ) ;
#14178 = AXIS2_PLACEMENT_3D ( 'NONE', #38285, #20210, #29345 ) ;
#14179 = CARTESIAN_POINT ( 'NONE',  ( -17.34253826592568970, 27.32041144456614390, -5.000000000000000000 ) ) ;
#14180 = DIRECTION ( 'NONE',  ( -0.5000000000000039968, -0.8660254037844363761, 0.000000000000000000 ) ) ;
#14181 = CONICAL_SURFACE ( 'NONE', #15400, 1.000000000000000888, 0.7853981633974552734 ) ;
#14182 = CARTESIAN_POINT ( 'NONE',  ( -26.75556982913416704, -25.10111586528267935, -7.156957325213197940 ) ) ;
#14183 = CARTESIAN_POINT ( 'NONE',  ( 1.794506358125838696, -24.59416170551979519, -7.919342959519173775 ) ) ;
#14184 = CARTESIAN_POINT ( 'NONE',  ( 12.32508505241873031, 19.69439391497782665, -20.57495747500194483 ) ) ;
#14185 = CARTESIAN_POINT ( 'NONE',  ( 20.27016213421537572, 13.74473133855453533, -9.391409443377602528 ) ) ;
#14186 = LINE ( 'NONE', #1602, #36792 ) ;
#14187 = EDGE_CURVE ( 'NONE', #802, #10420, #20712, .T. ) ;
#14188 = ORIENTED_EDGE ( 'NONE', *, *, #12097, .T. ) ;
#14189 = CARTESIAN_POINT ( 'NONE',  ( -4.067729689095753720, 20.10162097886301780, -29.23193154362917667 ) ) ;
#14190 = ORIENTED_EDGE ( 'NONE', *, *, #21163, .T. ) ;
#14191 = CARTESIAN_POINT ( 'NONE',  ( 0.000000000000000000, 22.50000000000000355, 7.000000000000000000 ) ) ;
#14192 = ORIENTED_EDGE ( 'NONE', *, *, #27799, .T. ) ;
#14193 = DIRECTION ( 'NONE',  ( 0.000000000000000000, -1.000000000000000000, 0.000000000000000000 ) ) ;
#14194 = CARTESIAN_POINT ( 'NONE',  ( 9.331903152615751651, 11.35703883385569135, 10.49999999999999822 ) ) ;
#14195 = VERTEX_POINT ( 'NONE', #5131 ) ;
#14196 = CARTESIAN_POINT ( 'NONE',  ( -28.71628164481152368, 0.3103093194282594558, -11.60661526385460718 ) ) ;
#14197 = EDGE_LOOP ( 'NONE', ( #30339, #21513, #2706, #19642 ) ) ;
#14198 = CARTESIAN_POINT ( 'NONE',  ( 20.15225922584352958, -5.429322806097534482, -27.08385357569856922 ) ) ;
#14199 = CIRCLE ( 'NONE', #28457, 1.000000000000000000 ) ;
#14200 = AXIS2_PLACEMENT_3D ( 'NONE', #8145, #2259, #23391 ) ;
#14201 = VECTOR ( 'NONE', #2911, 1000.000000000000227 ) ;
#14202 = ORIENTED_EDGE ( 'NONE', *, *, #19053, .F. ) ;
#14203 = ITEM_DEFINED_TRANSFORMATION ( 'NONE', 'NONE', #24864,  #24238 ) ;
#14204 = CARTESIAN_POINT ( 'NONE',  ( 14.07088901726639918, 27.73527618063598510, 10.49999999999999822 ) ) ;
#14205 = ORIENTED_EDGE ( 'NONE', *, *, #17328, .T. ) ;
#14206 = VECTOR ( 'NONE', #20162, 1000.000000000000114 ) ;
#14207 = DIRECTION ( 'NONE',  ( -0.4067366430757984874, -0.9135454576426016438, 0.000000000000000000 ) ) ;
#14208 = CARTESIAN_POINT ( 'NONE',  ( 25.71480618106366833, 9.014447550976067092, 11.00000000000101785 ) ) ;
#14209 = CARTESIAN_POINT ( 'NONE',  ( -12.83067079990756909, 27.60880874002097940, 18.42518152272070964 ) ) ;
#14210 = LINE ( 'NONE', #27007, #22000 ) ;
#14211 = ORIENTED_EDGE ( 'NONE', *, *, #26548, .T. ) ;
#14212 = DIRECTION ( 'NONE',  ( 1.000000000000000000, 0.000000000000000000, 0.000000000000000000 ) ) ;
#14213 = DIRECTION ( 'NONE',  ( 1.000000000000000000, 0.000000000000000000, 0.000000000000000000 ) ) ;
#14214 = EDGE_CURVE ( 'NONE', #36487, #7885, #34656, .T. ) ;
#14215 = DIRECTION ( 'NONE',  ( 0.1470157664652005924, 0.6916548014802259559, -0.7071067811865465735 ) ) ;
#14216 = CARTESIAN_POINT ( 'NONE',  ( 18.36481394660784616, 17.66788468870112183, -8.868296049281793714 ) ) ;
#14217 = CARTESIAN_POINT ( 'NONE',  ( 11.61237692786606779, 33.10454720036470633, -7.206114420758453321 ) ) ;
#14218 = ORIENTED_EDGE ( 'NONE', *, *, #16970, .F. ) ;
#14219 = DIRECTION ( 'NONE',  ( -0.4067366430757888285, 0.9135454576426059736, -0.000000000000000000 ) ) ;
#14220 = CARTESIAN_POINT ( 'NONE',  ( 10.86866341958027249, -19.47793087445224103, -22.69139715315293770 ) ) ;
#14221 = CARTESIAN_POINT ( 'NONE',  ( 1.871201846650637046, 31.30332840660451765, 6.000000000000000000 ) ) ;
#14222 = PLANE ( 'NONE',  #10249 ) ;
#14223 = VECTOR ( 'NONE', #20579, 1000.000000000000000 ) ;
#14225 = AXIS2_PLACEMENT_3D ( 'NONE', #39950, #15174, #15972 ) ;
#14224 = CARTESIAN_POINT ( 'NONE',  ( -11.07085948108040974, 17.50394663469646517, -27.44763187279587413 ) ) ;
#14226 = CARTESIAN_POINT ( 'NONE',  ( -20.70549897995557842, -28.06280627726274801, 15.13084544680213384 ) ) ;
#14227 = CARTESIAN_POINT ( 'NONE',  ( 13.27451975403652540, -24.88833393671288619, -11.62983193108599700 ) ) ;
#14228 = EDGE_CURVE ( 'NONE', #11410, #17070, #30454, .T. ) ;
#14229 = FACE_OUTER_BOUND ( 'NONE', #30895, .T. ) ;
#14230 = EDGE_LOOP ( 'NONE', ( #4788, #14083 ) ) ;
#14231 = ORIENTED_EDGE ( 'NONE', *, *, #37797, .T. ) ;
#14232 = CIRCLE ( 'NONE', #12923, 1.000000000000000888 ) ;
#14233 = CARTESIAN_POINT ( 'NONE',  ( -7.924297901226319496, 19.68525824574059158, -25.90363148246721181 ) ) ;
#14234 = DIRECTION ( 'NONE',  ( 0.000000000000000000, 0.000000000000000000, -1.000000000000000000 ) ) ;
#14235 = EDGE_CURVE ( 'NONE', #27237, #34166, #16078, .T. ) ;
#14236 = FACE_BOUND ( 'NONE', #39887, .T. ) ;
#14237 = CARTESIAN_POINT ( 'NONE',  ( -34.47791643563932951, -6.499699467164269606, -7.206147143098082353 ) ) ;
#14238 = CARTESIAN_POINT ( 'NONE',  ( 3.853166178176219425, 23.42705098312512746, 12.00000000000000000 ) ) ;
#14239 = ORIENTED_EDGE ( 'NONE', *, *, #32466, .T. ) ;
#14240 = CARTESIAN_POINT ( 'NONE',  ( 23.90523083592902864, 0.5703977246735572049, -19.50614640947865652 ) ) ;
#14241 = EDGE_CURVE ( 'NONE', #16505, #36670, #36016, .T. ) ;
#14242 = CARTESIAN_POINT ( 'NONE',  ( -10.47540670418176312, 32.60491492691384252, 11.00000000000000000 ) ) ;
#14243 = DIRECTION ( 'NONE',  ( 0.1045284632676436176, -0.9945218953682742891, 0.000000000000000000 ) ) ;
#14244 = FACE_OUTER_BOUND ( 'NONE', #19066, .T. ) ;
#14245 = EDGE_CURVE ( 'NONE', #5502, #26852, #33707, .T. ) ;
#14246 = VERTEX_POINT ( 'NONE', #8175 ) ;
#14247 = CARTESIAN_POINT ( 'NONE',  ( -21.27552871334581397, 0.7820719158082399813, -25.01525379879122113 ) ) ;
#14248 = CARTESIAN_POINT ( 'NONE',  ( 13.64210930126480115, 24.20081211342298744, 6.000000000000000000 ) ) ;
#14249 = ORIENTED_EDGE ( 'NONE', *, *, #12493, .T. ) ;
#14250 = CARTESIAN_POINT ( 'NONE',  ( 34.31080765618935402, -5.232520982112594865, -5.452539590646297896 ) ) ;
#14251 = CARTESIAN_POINT ( 'NONE',  ( 34.99622266290977279, -18.09877784578646498, 15.13084544680216048 ) ) ;
#14252 = ORIENTED_EDGE ( 'NONE', *, *, #22114, .T. ) ;
#14253 = CARTESIAN_POINT ( 'NONE',  ( 10.55929393610962741, 36.39458846701859329, 13.92931973827808712 ) ) ;
#14254 = CARTESIAN_POINT ( 'NONE',  ( -10.43399472912671300, -25.44514827097021836, 16.30093088680841618 ) ) ;
#14255 = CYLINDRICAL_SURFACE ( 'NONE', #25375, 1.000000000000000000 ) ;
#14256 = CARTESIAN_POINT ( 'NONE',  ( 4.499574175056302749, 28.42082499242057736, 20.82122704794079837 ) ) ;
#14257 = VECTOR ( 'NONE', #4364, 1000.000000000000000 ) ;
#14258 = DIRECTION ( 'NONE',  ( 0.000000000000000000, 0.000000000000000000, -1.000000000000000000 ) ) ;
#14259 = VERTEX_POINT ( 'NONE', #32773 ) ;
#14260 = DIRECTION ( 'NONE',  ( 1.000000000000000000, 0.000000000000000000, 0.000000000000000000 ) ) ;
#14261 = EDGE_CURVE ( 'NONE', #29047, #16453, #25705, .T. ) ;
#14262 = DIRECTION ( 'NONE',  ( 0.000000000000000000, 0.000000000000000000, 1.000000000000000000 ) ) ;
#14263 = EDGE_CURVE ( 'NONE', #3290, #21446, #3770, .T. ) ;
#14264 = AXIS2_PLACEMENT_3D ( 'NONE', #28593, #32460, #19447 ) ;
#14265 = CARTESIAN_POINT ( 'NONE',  ( 5.921814423382286918, 36.05187545745704369, -8.870160957477187580 ) ) ;
#14266 = CARTESIAN_POINT ( 'NONE',  ( 18.69487370500359091, 22.45507383323641193, -4.999999999999999112 ) ) ;
#14267 = CARTESIAN_POINT ( 'NONE',  ( 11.93114467671387047, 6.888449590841193348, 20.99999999999999645 ) ) ;
#14268 = CARTESIAN_POINT ( 'NONE',  ( 18.69514969737914001, -27.26850006250750624, -5.461146079405737375 ) ) ;
#14269 = CARTESIAN_POINT ( 'NONE',  ( 13.80292604922475874, 34.21633694312841811, 11.00000000000012434 ) ) ;
#14270 = DIRECTION ( 'NONE',  ( 1.000000000000000000, 0.000000000000000000, 0.000000000000000000 ) ) ;
#14271 = DIRECTION ( 'NONE',  ( 0.000000000000000000, 0.000000000000000000, 1.000000000000000000 ) ) ;
#14272 = ORIENTED_EDGE ( 'NONE', *, *, #10012, .F. ) ;
#14273 = CARTESIAN_POINT ( 'NONE',  ( 10.91553583107620007, 17.35227997941746025, -29.34686799396787649 ) ) ;
#14274 = EDGE_LOOP ( 'NONE', ( #26322, #20497, #36017, #28334, #3681 ) ) ;
#14275 = CARTESIAN_POINT ( 'NONE',  ( -12.91493168522746693, 20.67346994317426478, -18.49686148064046876 ) ) ;
#14276 = CARTESIAN_POINT ( 'NONE',  ( -31.50169271651420644, -8.384983552476358071, 19.27171037444088597 ) ) ;
#14277 = CARTESIAN_POINT ( 'NONE',  ( -14.44923221060097696, 26.57085556310783758, 10.49999999999999822 ) ) ;
#14278 = CARTESIAN_POINT ( 'NONE',  ( 11.52208528209529348, 18.40475063778455933, -23.85969712606921078 ) ) ;
#14279 = ORIENTED_EDGE ( 'NONE', *, *, #30897, .T. ) ;
#14280 = CARTESIAN_POINT ( 'NONE',  ( 32.82868241010613275, -19.42490378352035307, -7.116715984878871915 ) ) ;
#14281 = VERTEX_POINT ( 'NONE', #4931 ) ;
#14283 = DIRECTION ( 'NONE',  ( -0.5000000000000039968, -0.8660254037844363761, 0.000000000000000000 ) ) ;
#14282 = CARTESIAN_POINT ( 'NONE',  ( -10.74681136125822256, 17.71780809595123429, -27.42243502390378396 ) ) ;
#14284 = CARTESIAN_POINT ( 'NONE',  ( -14.06110963209943421, -22.53835070925789807, -16.29745831186998117 ) ) ;
#14285 = EDGE_CURVE ( 'NONE', #35381, #21371, #25153, .T. ) ;
#14286 = LINE ( 'NONE', #35628, #16557 ) ;
#14287 = ORIENTED_EDGE ( 'NONE', *, *, #2418, .F. ) ;
#14288 = CARTESIAN_POINT ( 'NONE',  ( -19.60397279729912157, -6.775456283739323737, -27.75461981094199260 ) ) ;
#14289 = CARTESIAN_POINT ( 'NONE',  ( -14.88818106304697508, -26.46991234739331844, -6.888965760716232012 ) ) ;
#14290 = FACE_OUTER_BOUND ( 'NONE', #19139, .T. ) ;
#14291 = CARTESIAN_POINT ( 'NONE',  ( 17.26836613049929881, 21.08639604684729463, -5.952994375637418401 ) ) ;
#14292 = ORIENTED_EDGE ( 'NONE', *, *, #30537, .F. ) ;
#14293 = CARTESIAN_POINT ( 'NONE',  ( 23.85642135670279629, 2.961483799603526368, -17.67184769396539323 ) ) ;
#14294 = CARTESIAN_POINT ( 'NONE',  ( -8.336672018935676221, 10.01592710129222752, 10.49999999999999822 ) ) ;
#14295 = CARTESIAN_POINT ( 'NONE',  ( -39.05366788733155659, -6.582903524761571923, 11.00000000000000000 ) ) ;
#14296 = AXIS2_PLACEMENT_3D ( 'NONE', #29949, #1520, #11072 ) ;
#14297 = ORIENTED_EDGE ( 'NONE', *, *, #25241, .T. ) ;
#14298 = ADVANCED_FACE ( 'NONE', ( #16370 ), #34003, .T. ) ;
#14299 = CARTESIAN_POINT ( 'NONE',  ( -29.76338656478942113, -0.1358195184987218418, -10.16612580020036916 ) ) ;
#14300 = CARTESIAN_POINT ( 'NONE',  ( 22.40604002092578995, -0.1555999769332679916, -22.63024419021551381 ) ) ;
#14301 = CARTESIAN_POINT ( 'NONE',  ( 31.08318648610487855, -11.03630075675846101, 19.66345542862528006 ) ) ;
#14302 = ORIENTED_EDGE ( 'NONE', *, *, #2420, .F. ) ;
#14303 = CARTESIAN_POINT ( 'NONE',  ( -28.62628535912805461, 0.9249821381284000221, -10.67733050510392268 ) ) ;
#14304 = CARTESIAN_POINT ( 'NONE',  ( 11.31392148919590923, 36.91540483778863546, -5.000000000000002665 ) ) ;
#14305 = CARTESIAN_POINT ( 'NONE',  ( -1.871208588069141143, 13.69667159339610762, 13.00000000000000178 ) ) ;
#14306 = CIRCLE ( 'NONE', #29873, 0.5000000000000004441 ) ;
#14307 = DIRECTION ( 'NONE',  ( 1.000000000000000000, 0.000000000000000000, 0.000000000000000000 ) ) ;
#14308 = EDGE_CURVE ( 'NONE', #32913, #12698, #19967, .T. ) ;
#14309 = ADVANCED_FACE ( 'NONE', ( #24212, #9178, #23815, #8574 ), #17739, .F. ) ;
#14310 = CARTESIAN_POINT ( 'NONE',  ( -1.734965421685230824, 7.600674680189156263, 7.000000000000000000 ) ) ;
#14311 = DIRECTION ( 'NONE',  ( 1.000000000000000000, 0.000000000000000000, 0.000000000000000000 ) ) ;
#14312 = FACE_OUTER_BOUND ( 'NONE', #24364, .T. ) ;
#14313 = VERTEX_POINT ( 'NONE', #36217 ) ;
#14314 = CARTESIAN_POINT ( 'NONE',  ( -25.53096875586516390, 6.216240356532259703, -5.478322317225678084 ) ) ;
#14315 = CARTESIAN_POINT ( 'NONE',  ( 10.39021566973303656, 20.90519018800546291, 10.50000000000000000 ) ) ;
#14316 = LINE ( 'NONE', #29955, #34998 ) ;
#14317 = CARTESIAN_POINT ( 'NONE',  ( 25.19512240098035250, -24.69066459180183415, -9.356458335724495257 ) ) ;
#14318 = AXIS2_PLACEMENT_3D ( 'NONE', #28850, #22546, #10976 ) ;
#14319 = CARTESIAN_POINT ( 'NONE',  ( -0.5000000000000005551, 33.00000000000000000, 10.00000000000000000 ) ) ;
#14320 = DIRECTION ( 'NONE',  ( -0.1045284632676436176, 0.9945218953682742891, 0.000000000000000000 ) ) ;
#14321 = CARTESIAN_POINT ( 'NONE',  ( 11.36962475154139796, 19.21036919021693024, -22.68052711305023905 ) ) ;
#14322 = CARTESIAN_POINT ( 'NONE',  ( 14.98890121934613440, -28.67928442654205057, 11.00000000000000000 ) ) ;
#14323 = ORIENTED_EDGE ( 'NONE', *, *, #9034, .F. ) ;
#14324 = CARTESIAN_POINT ( 'NONE',  ( -15.64269498361865729, 21.26784539589563394, -12.67544165040647464 ) ) ;
#14325 = CARTESIAN_POINT ( 'NONE',  ( -22.79104142221948592, -15.00151558123136830, 21.00000000000000000 ) ) ;
#14326 = CARTESIAN_POINT ( 'NONE',  ( 9.564543489041190227, -18.36833051452632048, -27.45183364396559256 ) ) ;
#14327 = LINE ( 'NONE', #24073, #15909 ) ;
#14328 = CARTESIAN_POINT ( 'NONE',  ( 11.13033197888396764, 17.60926338241307576, -26.83090848175526588 ) ) ;
#14329 = ORIENTED_EDGE ( 'NONE', *, *, #24021, .F. ) ;
#14330 = CARTESIAN_POINT ( 'NONE',  ( 8.927394655428276593, 11.06314620770945290, 7.000000000000000000 ) ) ;
#14331 = ORIENTED_EDGE ( 'NONE', *, *, #8610, .F. ) ;
#14333 = CARTESIAN_POINT ( 'NONE',  ( -5.064571727552472424, 31.45661825943146894, 12.00000000000000000 ) ) ;
#14332 = CARTESIAN_POINT ( 'NONE',  ( -15.17099104544988641, 26.61370929599295820, -7.820916635083668744 ) ) ;
#14334 = CARTESIAN_POINT ( 'NONE',  ( -14.89274031364858786, -25.83765763563116025, -9.708005537497479409 ) ) ;
#14335 = EDGE_CURVE ( 'NONE', #21780, #3918, #20780, .T. ) ;
#14336 = CARTESIAN_POINT ( 'NONE',  ( -33.69589222704901488, -0.03122585499731184155, 10.99999999999963585 ) ) ;
#14337 = AXIS2_PLACEMENT_3D ( 'NONE', #39442, #5511, #39243 ) ;
#14338 = CARTESIAN_POINT ( 'NONE',  ( -30.63528468994626053, -19.80586681999809784, -9.728514707820110630 ) ) ;
#14339 = CARTESIAN_POINT ( 'NONE',  ( -4.774817478240758639, -20.11729465013693385, -27.10572799927598808 ) ) ;
#14340 = CARTESIAN_POINT ( 'NONE',  ( 11.74040845465362892, 16.94500352943240173, -28.11737847864129591 ) ) ;
#14342 = ADVANCED_FACE ( 'NONE', ( #12023 ), #21564, .T. ) ;
#14341 = VERTEX_POINT ( 'NONE', #36610 ) ;
#14343 = CARTESIAN_POINT ( 'NONE',  ( 23.26889270032514645, 6.256968188779593376, -14.81455085170663821 ) ) ;
#14344 = VECTOR ( 'NONE', #3174, 1000.000000000000000 ) ;
#14345 = DIRECTION ( 'NONE',  ( 0.000000000000000000, 0.000000000000000000, 1.000000000000000000 ) ) ;
#14346 = CARTESIAN_POINT ( 'NONE',  ( -1.587667106213708879, 35.31811204475769728, 6.000000000000000000 ) ) ;
#14347 = DIRECTION ( 'NONE',  ( 0.000000000000000000, 0.000000000000000000, 1.000000000000000000 ) ) ;
#14348 = EDGE_LOOP ( 'NONE', ( #6128, #9827, #34049, #15044 ) ) ;
#14349 = CARTESIAN_POINT ( 'NONE',  ( -30.62465793492241062, -2.263991001138987436, -11.41340153498721222 ) ) ;
#14350 = CARTESIAN_POINT ( 'NONE',  ( 30.20212831021078870, -0.007183286174248709743, -8.767436680044319530 ) ) ;
#14351 = EDGE_CURVE ( 'NONE', #9357, #26640, #21170, .T. ) ;
#14352 = CARTESIAN_POINT ( 'NONE',  ( -6.367390439426989346, 24.26983560721853195, 20.94377226548378346 ) ) ;
#14353 = CARTESIAN_POINT ( 'NONE',  ( 24.69586183797155599, -8.725643957991929156, 20.99999999999999645 ) ) ;
#14354 = FACE_OUTER_BOUND ( 'NONE', #24018, .T. ) ;
#14355 = AXIS2_PLACEMENT_3D ( 'NONE', #3619, #12958, #6460 ) ;
#14356 = DIRECTION ( 'NONE',  ( -0.8910065241883693421, -0.4539904997395438069, 0.000000000000000000 ) ) ;
#14357 = DIRECTION ( 'NONE',  ( -0.000000000000000000, -0.000000000000000000, 1.000000000000000000 ) ) ;
#14358 = EDGE_LOOP ( 'NONE', ( #36481, #25574, #10506 ) ) ;
#14359 = ADVANCED_FACE ( 'NONE', ( #33962 ), #40045, .F. ) ;
#14360 = DIRECTION ( 'NONE',  ( 0.000000000000000000, 0.000000000000000000, 1.000000000000000000 ) ) ;
#14361 = EDGE_CURVE ( 'NONE', #34828, #4212, #11633, .T. ) ;
#14362 = EDGE_CURVE ( 'NONE', #11948, #32551, #14878, .T. ) ;
#14363 = AXIS2_PLACEMENT_3D ( 'NONE', #428, #12808, #13005 ) ;
#14364 = CARTESIAN_POINT ( 'NONE',  ( 15.02235689379175732, 21.92659494635341844, 7.000000000000000000 ) ) ;
#14365 = ORIENTED_EDGE ( 'NONE', *, *, #30256, .T. ) ;
#14366 = CARTESIAN_POINT ( 'NONE',  ( 0.2333680323409619561, 22.01890222510690975, -24.21865200866544399 ) ) ;
#14367 = CIRCLE ( 'NONE', #2051, 1.000000000000000888 ) ;
#14368 = CARTESIAN_POINT ( 'NONE',  ( 0.2474667741973399226, 28.36888560440311480, 13.00000000000000178 ) ) ;
#14369 = CARTESIAN_POINT ( 'NONE',  ( 7.962467718761615743, 24.71319220551615814, 20.69868183039780973 ) ) ;
#14370 = FACE_OUTER_BOUND ( 'NONE', #31043, .T. ) ;
#14371 = DIRECTION ( 'NONE',  ( 1.000000000000000000, 0.000000000000000000, 0.000000000000000000 ) ) ;
#14372 = DIRECTION ( 'NONE',  ( 1.000000000000000000, 0.000000000000000000, 0.000000000000000000 ) ) ;
#14373 = CARTESIAN_POINT ( 'NONE',  ( 10.48996851602322344, 18.64616631778530120, -24.90364434592935083 ) ) ;
#14374 = CARTESIAN_POINT ( 'NONE',  ( -13.94482798346716201, 26.50521816028930644, 7.000000000000000000 ) ) ;
#14375 = ORIENTED_EDGE ( 'NONE', *, *, #5915, .T. ) ;
#14377 = CARTESIAN_POINT ( 'NONE',  ( -7.111215932167764819, 17.81698729810783988, 7.000000000000000000 ) ) ;
#14376 = CARTESIAN_POINT ( 'NONE',  ( -16.98576275542438196, 14.17128621410275180, -20.06049913518808125 ) ) ;
#14378 = DIRECTION ( 'NONE',  ( 0.000000000000000000, 0.000000000000000000, -1.000000000000000000 ) ) ;
#14379 = CIRCLE ( 'NONE', #3355, 1.000000000000000000 ) ;
#14380 = CARTESIAN_POINT ( 'NONE',  ( 10.56515747574125541, -19.56746311216371481, -22.73119885331434276 ) ) ;
#14381 = CARTESIAN_POINT ( 'NONE',  ( 8.927394655428276593, 11.06314620770945290, 9.000000000000001776 ) ) ;
#14382 = CARTESIAN_POINT ( 'NONE',  ( 10.98291459920649338, 17.36300444913146634, -28.70599113223154930 ) ) ;
#14383 = CARTESIAN_POINT ( 'NONE',  ( 17.34253826539385201, 27.32041144647958575, -13.70816084473008800 ) ) ;
#14384 = CARTESIAN_POINT ( 'NONE',  ( 14.36830325120613239, 20.48707633493483371, 7.000000000000000000 ) ) ;
#14385 = EDGE_CURVE ( 'NONE', #20919, #9948, #26556, .T. ) ;
#14386 = CARTESIAN_POINT ( 'NONE',  ( -15.65942272168468996, -13.82713998445992054, -27.03602420171817045 ) ) ;
#14387 = CARTESIAN_POINT ( 'NONE',  ( 3.914585310762173087, -24.47571531563621861, -9.381846448608621714 ) ) ;
#14388 = CARTESIAN_POINT ( 'NONE',  ( 15.50434170514593468, 26.37861656039416047, -5.946155412696958464 ) ) ;
#14389 = EDGE_CURVE ( 'NONE', #35442, #38427, #33378, .T. ) ;
#14390 = CARTESIAN_POINT ( 'NONE',  ( 19.21831362878624816, 14.20819548674236543, -12.87518209901260846 ) ) ;
#14391 = CARTESIAN_POINT ( 'NONE',  ( -2.525645716490712012, 8.212903943950955465, 7.499999999999997335 ) ) ;
#14392 = VERTEX_POINT ( 'NONE', #30318 ) ;
#14393 = B_SPLINE_CURVE_WITH_KNOTS ( 'NONE', 3,
 ( #2336, #5774, #30368, #11475, #39699, #39298 ),
 .UNSPECIFIED., .F., .F.,
 ( 4, 2, 4 ),
 ( 0.000000000000000000, 0.5000000000000000000, 1.000000000000000000 ),
 .UNSPECIFIED. ) ;
#14394 = CARTESIAN_POINT ( 'NONE',  ( -6.368201183702909773, 37.02352246815677717, -6.288982803245489528 ) ) ;
#14395 = ORIENTED_EDGE ( 'NONE', *, *, #29376, .F. ) ;
#14396 = VECTOR ( 'NONE', #18864, 1000.000000000000000 ) ;
#14397 = CARTESIAN_POINT ( 'NONE',  ( -14.51390269127088928, 5.102206419419879957, 7.499999999999991118 ) ) ;
#14398 = ORIENTED_EDGE ( 'NONE', *, *, #36219, .T. ) ;
#14399 = DIRECTION ( 'NONE',  ( 1.000000000000000000, 0.000000000000000000, 0.000000000000000000 ) ) ;
#14400 = DIRECTION ( 'NONE',  ( 0.000000000000000000, 0.000000000000000000, 1.000000000000000000 ) ) ;
#14401 = ORIENTED_EDGE ( 'NONE', *, *, #28856, .F. ) ;
#14402 = CARTESIAN_POINT ( 'NONE',  ( -20.51831096985980807, 1.024188904302109737, -28.71274422071960331 ) ) ;
#14403 = EDGE_LOOP ( 'NONE', ( #21842, #13021, #28699, #4606 ) ) ;
#14404 = CARTESIAN_POINT ( 'NONE',  ( 34.80199681878606555, -10.49577831786894677, -8.021756253636395328 ) ) ;
#14405 = ORIENTED_EDGE ( 'NONE', *, *, #35945, .F. ) ;
#14406 = APPLICATION_PROTOCOL_DEFINITION ( 'draft international standard', 'automotive_design', 1998, #31140 ) ;
#14407 = CIRCLE ( 'NONE', #32602, 16.00000000000000000 ) ;
#14408 = CARTESIAN_POINT ( 'NONE',  ( 11.03640989728592281, 29.14264673470096767, 12.00000000000000000 ) ) ;
#14409 = ORIENTED_EDGE ( 'NONE', *, *, #12109, .F. ) ;
#14410 = CARTESIAN_POINT ( 'NONE',  ( 3.992867117591230919, 8.524771480177550487, 7.000000000000000000 ) ) ;
#14411 = FACE_OUTER_BOUND ( 'NONE', #10657, .T. ) ;
#14412 = CARTESIAN_POINT ( 'NONE',  ( -4.003793317224517700, 8.420815634768723967, 7.499999999999997335 ) ) ;
#14413 = EDGE_LOOP ( 'NONE', ( #13364, #10462 ) ) ;
#14414 = CARTESIAN_POINT ( 'NONE',  ( 3.587660364795204782, 9.681887955242936883, 6.000000000000000000 ) ) ;
#14415 = DIRECTION ( 'NONE',  ( -0.1470157664652036733, -0.6916548014802235134, -0.7071067811865484609 ) ) ;
#14416 = CARTESIAN_POINT ( 'NONE',  ( 16.36340388119751310, 15.09553078370668366, -20.01599901236055956 ) ) ;
#14417 = CARTESIAN_POINT ( 'NONE',  ( 13.11118861972762240, 31.67446990147458052, -5.902404578990857686 ) ) ;
#14418 = EDGE_LOOP ( 'NONE', ( #7209, #24186, #22360 ) ) ;
#14419 = CARTESIAN_POINT ( 'NONE',  ( -7.419976537719776388, 10.58597682645832450, 9.500000000000000000 ) ) ;
#14420 = VECTOR ( 'NONE', #17980, 1000.000000000000000 ) ;
#14421 = CARTESIAN_POINT ( 'NONE',  ( -14.09933648065464062, 26.02968990214173317, 7.499999999999993783 ) ) ;
#14422 = CARTESIAN_POINT ( 'NONE',  ( 15.47930552936342963, -26.10041863403043649, -9.214347334491035824 ) ) ;
#14423 = DIRECTION ( 'NONE',  ( 0.000000000000000000, 0.000000000000000000, 1.000000000000000000 ) ) ;
#14424 = CARTESIAN_POINT ( 'NONE',  ( -10.39021566973305788, 20.90519018800561568, 10.00000000000000000 ) ) ;
#14425 = CARTESIAN_POINT ( 'NONE',  ( -15.41023552481722447, 26.80405844223972522, -5.474109759163972910 ) ) ;
#14426 = CARTESIAN_POINT ( 'NONE',  ( -30.62963707967903559, -23.89786472172323073, 15.13084544680214094 ) ) ;
#14427 = CARTESIAN_POINT ( 'NONE',  ( 10.09725523659168722, -20.16347431786755706, -21.70548052805963835 ) ) ;
#14428 = LINE ( 'NONE', #4689, #36104 ) ;
#14429 = ORIENTED_EDGE ( 'NONE', *, *, #22803, .T. ) ;
#14430 = VERTEX_POINT ( 'NONE', #2488 ) ;
#14431 = CARTESIAN_POINT ( 'NONE',  ( -10.34192303438924299, 26.07364305517009839, -16.01722023157933705 ) ) ;
#14432 = DIRECTION ( 'NONE',  ( -0.000000000000000000, -0.000000000000000000, -1.000000000000000000 ) ) ;
#14433 = CARTESIAN_POINT ( 'NONE',  ( 9.559505275947156377, 25.28115294937476065, 13.00000000000000178 ) ) ;
#14434 = CIRCLE ( 'NONE', #39730, 60.00000000000006395 ) ;
#14435 = DIRECTION ( 'NONE',  ( 0.000000000000000000, 0.000000000000000000, 1.000000000000000000 ) ) ;
#14436 = ORIENTED_EDGE ( 'NONE', *, *, #31491, .T. ) ;
#14437 = CARTESIAN_POINT ( 'NONE',  ( 20.96446129645448408, 0.8575792327581100993, -26.22921226360291769 ) ) ;
#14438 = CARTESIAN_POINT ( 'NONE',  ( 11.48173768534036121, 32.16538668264416145, 10.63089969389957190 ) ) ;
#14439 = DIRECTION ( 'NONE',  ( -0.5877852522924690293, 0.8090169943749503378, 0.000000000000000000 ) ) ;
#14440 = CARTESIAN_POINT ( 'NONE',  ( -28.25062263172018007, -27.03061230010028382, 11.00000000000007994 ) ) ;
#14441 = B_SPLINE_CURVE_WITH_KNOTS ( 'NONE', 3,
 ( #25346, #37942, #37746, #21899, #37349, #9917 ),
 .UNSPECIFIED., .F., .F.,
 ( 4, 2, 4 ),
 ( 0.000000000000000000, 0.5000000000000000000, 1.000000000000000000 ),
 .UNSPECIFIED. ) ;
#14442 = ORIENTED_EDGE ( 'NONE', *, *, #4509, .F. ) ;
#14443 = CARTESIAN_POINT ( 'NONE',  ( -28.32157472073443216, 0.1617651296188915844, -12.55129266915809261 ) ) ;
#14444 = CARTESIAN_POINT ( 'NONE',  ( -13.48130249190472796, 27.93180293473203690, 10.50000000000000533 ) ) ;
#14445 = ORIENTED_EDGE ( 'NONE', *, *, #14900, .T. ) ;
#14446 = CARTESIAN_POINT ( 'NONE',  ( 30.24971233770529011, -4.493041484851756806, -13.15307322356999897 ) ) ;
#14447 = CARTESIAN_POINT ( 'NONE',  ( 26.12394372346528471, -27.06777822797228694, 14.53008259254010959 ) ) ;
#14448 = EDGE_LOOP ( 'NONE', ( #16077, #24385, #38228 ) ) ;
#14449 = CARTESIAN_POINT ( 'NONE',  ( 11.85731412588707023, 35.03474529413809080, 14.53008259254007761 ) ) ;
#14450 = CARTESIAN_POINT ( 'NONE',  ( 15.60391421431025449, -26.29546805949347998, 16.87380292611441490 ) ) ;
#14451 = DIRECTION ( 'NONE',  ( -0.000000000000000000, -0.000000000000000000, -1.000000000000000000 ) ) ;
#14452 = CARTESIAN_POINT ( 'NONE',  ( 7.531283639252310813, 27.60866748444399121, 20.50957957746029692 ) ) ;
#14453 = AXIS2_PLACEMENT_3D ( 'NONE', #21409, #5964, #19714 ) ;
#14454 = CARTESIAN_POINT ( 'NONE',  ( 8.238488885696289898, 24.65111619403943877, 7.000000000000000000 ) ) ;
#14455 = ORIENTED_EDGE ( 'NONE', *, *, #26286, .F. ) ;
#14456 = EDGE_CURVE ( 'NONE', #9704, #7162, #19853, .T. ) ;
#14457 = CARTESIAN_POINT ( 'NONE',  ( -8.927394655428429360, 11.06314620770957013, 7.500000000000000888 ) ) ;
#14458 = AXIS2_PLACEMENT_3D ( 'NONE', #34154, #23, #9963 ) ;
#14459 = CARTESIAN_POINT ( 'NONE',  ( -6.935776944912362296, 22.65328985282726393, 6.000000000000000000 ) ) ;
#14460 = B_SPLINE_CURVE_WITH_KNOTS ( 'NONE', 3,
 ( #7063, #31659, #17033, #19259 ),
 .UNSPECIFIED., .F., .F.,
 ( 4, 4 ),
 ( 0.000000000000000000, 1.000000000000000000 ),
 .UNSPECIFIED. ) ;
#14461 = CARTESIAN_POINT ( 'NONE',  ( 7.119170425228222854, 36.77535074466948117, -5.866140454657438497 ) ) ;
#14462 = CIRCLE ( 'NONE', #2781, 15.00000000000000000 ) ;
#14463 = DIRECTION ( 'NONE',  ( 0.000000000000000000, 0.000000000000000000, 1.000000000000000000 ) ) ;
#14464 = EDGE_CURVE ( 'NONE', #15130, #25273, #36284, .T. ) ;
#14465 = CARTESIAN_POINT ( 'NONE',  ( 10.34254640627884214, 25.37474234121230054, 19.99202127657103389 ) ) ;
#14466 = EDGE_CURVE ( 'NONE', #3606, #20361, #6414, .T. ) ;
#14467 = CARTESIAN_POINT ( 'NONE',  ( 17.86116285895126410, -24.79026673224041843, -12.29608082019653459 ) ) ;
#14468 = DIRECTION ( 'NONE',  ( 0.000000000000000000, 0.000000000000000000, -1.000000000000000000 ) ) ;
#14469 = CARTESIAN_POINT ( 'NONE',  ( -13.30684946193824914, 15.76689913224038264, 10.49999999999999822 ) ) ;
#14470 = DIRECTION ( 'NONE',  ( -1.000000000000000000, -0.000000000000000000, -0.000000000000000000 ) ) ;
#14471 = ORIENTED_EDGE ( 'NONE', *, *, #14721, .F. ) ;
#14472 = CIRCLE ( 'NONE', #33315, 1.000000000000000888 ) ;
#14473 = CARTESIAN_POINT ( 'NONE',  ( 14.23710703006283396, 24.61411403652301644, -12.53843163329819532 ) ) ;
#14474 = VERTEX_POINT ( 'NONE', #24414 ) ;
#14475 = CARTESIAN_POINT ( 'NONE',  ( -15.51364032778053925, 26.43312886238355119, -5.474109364757008045 ) ) ;
#14476 = CARTESIAN_POINT ( 'NONE',  ( -27.04163063101245612, -21.95895612274718900, 18.87996532025785257 ) ) ;
#14477 = FACE_OUTER_BOUND ( 'NONE', #21642, .T. ) ;
#14478 = CARTESIAN_POINT ( 'NONE',  ( 14.88668315484156146, 25.46919082029659620, -10.18295691443133499 ) ) ;
#14479 = ORIENTED_EDGE ( 'NONE', *, *, #26745, .T. ) ;
#14480 = CARTESIAN_POINT ( 'NONE',  ( 21.74907656359282626, -13.77287494480177976, -19.63093583157703748 ) ) ;
#14481 = ORIENTED_EDGE ( 'NONE', *, *, #19138, .T. ) ;
#14483 = CARTESIAN_POINT ( 'NONE',  ( -19.26948696230207858, 27.85601271560029701, 11.00000000000000000 ) ) ;
#14482 = CARTESIAN_POINT ( 'NONE',  ( -10.79408003525095694, 18.03183192774827859, -26.18276724716969639 ) ) ;
#14484 = CARTESIAN_POINT ( 'NONE',  ( -10.48684353440000194, -17.61503585894356050, -29.32750364307806734 ) ) ;
#14485 = CARTESIAN_POINT ( 'NONE',  ( -13.80736835487442349, 15.68301270189233954, 7.000000000000000000 ) ) ;
#14486 = CIRCLE ( 'NONE', #19040, 16.00000000000000355 ) ;
#14487 = ORIENTED_EDGE ( 'NONE', *, *, #20329, .F. ) ;
#14488 = CARTESIAN_POINT ( 'NONE',  ( -35.13470064561631290, -12.09547139906384672, -7.143865450880896972 ) ) ;
#14489 = CARTESIAN_POINT ( 'NONE',  ( -14.35490488552378174, -25.85456304999896560, -9.246097774239588674 ) ) ;
#14490 = CARTESIAN_POINT ( 'NONE',  ( -3.399837471815634338, 8.909889435135630364, 10.00000000000000000 ) ) ;
#14491 = ORIENTED_EDGE ( 'NONE', *, *, #18373, .T. ) ;
#14492 = CARTESIAN_POINT ( 'NONE',  ( 28.61305316926027587, 1.166352659189931140, -10.20691745326966604 ) ) ;
#14493 = LINE ( 'NONE', #11453, #34908 ) ;
#14494 = ADVANCED_FACE ( 'NONE', ( #18323 ), #30719, .F. ) ;
#14495 = CARTESIAN_POINT ( 'NONE',  ( -23.09341953181405671, -31.04079623447176317, 11.00000000000000000 ) ) ;
#14496 = EDGE_CURVE ( 'NONE', #38107, #7643, #30999, .T. ) ;
#14497 = ORIENTED_EDGE ( 'NONE', *, *, #27152, .F. ) ;
#14498 = CARTESIAN_POINT ( 'NONE',  ( -27.21489488970257753, 0.1324291793181980870, -14.46509639632424360 ) ) ;
#14499 = CARTESIAN_POINT ( 'NONE',  ( 22.96275717310609110, -0.2160451777520107086, -21.50653127259290898 ) ) ;
#14500 = VECTOR ( 'NONE', #8430, 1000.000000000000000 ) ;
#14501 = CARTESIAN_POINT ( 'NONE',  ( 28.59012753013995223, -4.062670752121350759, 19.66345542862688944 ) ) ;
#14502 = ORIENTED_EDGE ( 'NONE', *, *, #29167, .F. ) ;
#14503 = CARTESIAN_POINT ( 'NONE',  ( -23.97679352225928184, 2.727602047639537730, -17.65530553011062054 ) ) ;
#14504 = DIRECTION ( 'NONE',  ( 0.000000000000000000, 0.000000000000000000, 1.000000000000000000 ) ) ;
#14505 = AXIS2_PLACEMENT_3D ( 'NONE', #4166, #17790, #26516 ) ;
#14506 = CARTESIAN_POINT ( 'NONE',  ( -12.49038105676665644, 14.13397459621567798, 7.000000000000000000 ) ) ;
#14507 = CIRCLE ( 'NONE', #17778, 17.00000000000000355 ) ;
#14508 = CARTESIAN_POINT ( 'NONE',  ( 13.26584437371809777, 27.13525491562438319, 13.00000000000000178 ) ) ;
#14509 = EDGE_CURVE ( 'NONE', #39108, #10259, #6729, .T. ) ;
#14510 = CIRCLE ( 'NONE', #33977, 1.000000000000000000 ) ;
#14511 = CARTESIAN_POINT ( 'NONE',  ( 3.000488737323008248, 30.46850471149999962, 9.000000000000001776 ) ) ;
#14512 = DIRECTION ( 'NONE',  ( 0.7431448254773953543, 0.6691306063588570163, 0.000000000000000000 ) ) ;
#14513 = LINE ( 'NONE', #12063, #6821 ) ;
#14514 = EDGE_LOOP ( 'NONE', ( #34768, #28034 ) ) ;
#14515 = CARTESIAN_POINT ( 'NONE',  ( -20.09296739951089350, 5.008361712747955607, -27.07435144307553898 ) ) ;
#14516 = DIRECTION ( 'NONE',  ( 0.6724985119639642628, -0.2185080122244146550, -0.7071067811865395791 ) ) ;
#14517 = PLANE ( 'NONE',  #17495 ) ;
#14518 = CARTESIAN_POINT ( 'NONE',  ( 15.05365685536567355, -14.74619886204681585, -26.38815432015796958 ) ) ;
#14519 = LINE ( 'NONE', #7818, #6678 ) ;
#14520 = CARTESIAN_POINT ( 'NONE',  ( -14.81881748179393199, 20.25565617689067111, 10.49999999999999822 ) ) ;
#14521 = CARTESIAN_POINT ( 'NONE',  ( 15.01939689310542825, 26.78336088948045557, -8.278624996432389693 ) ) ;
#14522 = CARTESIAN_POINT ( 'NONE',  ( 5.096756537559935296, -26.22849730612247754, 13.92931973827808712 ) ) ;
#14523 = EDGE_LOOP ( 'NONE', ( #31161, #33367, #16892, #34801 ) ) ;
#14524 = APPLICATION_CONTEXT ( 'automotive_design' ) ;
#14525 = AXIS2_PLACEMENT_3D ( 'NONE', #28191, #31641, #566 ) ;
#14526 = CARTESIAN_POINT ( 'NONE',  ( -16.10992647123930510, 22.10140223917236213, -10.24986995600674078 ) ) ;
#14527 = CARTESIAN_POINT ( 'NONE',  ( -18.52756972024271320, -17.82802275548162285, 20.94377226548378701 ) ) ;
#14528 = CARTESIAN_POINT ( 'NONE',  ( -11.22168704032801401, 31.70696390855199454, 10.83333333333332860 ) ) ;
#14529 = CARTESIAN_POINT ( 'NONE',  ( 15.43121851897235786, 26.72868093004962020, -5.474190317923420146 ) ) ;
#14530 = ORIENTED_EDGE ( 'NONE', *, *, #11860, .F. ) ;
#14531 = DIRECTION ( 'NONE',  ( 0.000000000000000000, 0.000000000000000000, -1.000000000000000000 ) ) ;
#14532 = ORIENTED_EDGE ( 'NONE', *, *, #7482, .F. ) ;
#14534 = DIRECTION ( 'NONE',  ( 0.000000000000000000, 0.000000000000000000, 1.000000000000000000 ) ) ;
#14533 = CARTESIAN_POINT ( 'NONE',  ( -10.99222416622049359, 17.55659943774363185, -27.44150676154917790 ) ) ;
#14535 = CARTESIAN_POINT ( 'NONE',  ( -14.83405348788300415, -25.67306116219898726, -10.17574755994341373 ) ) ;
#14536 = CARTESIAN_POINT ( 'NONE',  ( -35.68447701591266963, -3.401722300707785251, 11.55979286843934872 ) ) ;
#14537 = CARTESIAN_POINT ( 'NONE',  ( -33.53737908833902992, -18.88502799929946008, -5.855487158225816557 ) ) ;
#14538 = AXIS2_PLACEMENT_3D ( 'NONE', #9527, #27257, #6461 ) ;
#14539 = CARTESIAN_POINT ( 'NONE',  ( -11.57545763705510744, -25.81734924782649543, -5.474310789163009616 ) ) ;
#14540 = CARTESIAN_POINT ( 'NONE',  ( -9.697889840765284930, 31.90483559858339646, 9.500000000000000000 ) ) ;
#14541 = CARTESIAN_POINT ( 'NONE',  ( 15.84467149865224833, 25.30824157118464868, -5.000000000000000888 ) ) ;
#14542 = ORIENTED_EDGE ( 'NONE', *, *, #22530, .F. ) ;
#14543 = CARTESIAN_POINT ( 'NONE',  ( 23.06768432047073247, 7.142456518765742501, -13.83685962162048710 ) ) ;
#14544 = DIRECTION ( 'NONE',  ( 0.000000000000000000, 0.000000000000000000, 1.000000000000000000 ) ) ;
#14545 = DIRECTION ( 'NONE',  ( -0.9945218953682745111, -0.1045284632676436454, 0.000000000000000000 ) ) ;
#14546 = ADVANCED_FACE ( 'NONE', ( #24811 ), #34165, .F. ) ;
#14547 = FACE_OUTER_BOUND ( 'NONE', #27323, .T. ) ;
#14548 = ORIENTED_EDGE ( 'NONE', *, *, #21732, .T. ) ;
#14549 = CARTESIAN_POINT ( 'NONE',  ( -30.56639149896655638, -1.107291129257161444, -10.09863760926522325 ) ) ;
#14550 = VECTOR ( 'NONE', #21756, 1000.000000000000000 ) ;
#14551 = CARTESIAN_POINT ( 'NONE',  ( 30.94782199696930647, -0.1917222966042023691, -6.413581524601221773 ) ) ;
#14552 = FACE_OUTER_BOUND ( 'NONE', #7692, .T. ) ;
#14553 = CARTESIAN_POINT ( 'NONE',  ( 22.84262768307193170, -16.00844090263227315, 20.99999999999995026 ) ) ;
#14554 = DIRECTION ( 'NONE',  ( 1.000000000000000000, 0.000000000000000000, 0.000000000000000000 ) ) ;
#14555 = FACE_OUTER_BOUND ( 'NONE', #21768, .T. ) ;
#14556 = B_SPLINE_CURVE_WITH_KNOTS ( 'NONE', 3,
 ( #36740, #3399, #2805, #6634, #21882, #24343, #28183, #33702 ),
 .UNSPECIFIED., .F., .F.,
 ( 4, 2, 2, 4 ),
 ( 0.000000000000000000, 0.0002364868538934255301, 0.0004729737077868510602, 0.0009459474155737019035 ),
 .UNSPECIFIED. ) ;
#14557 = CYLINDRICAL_SURFACE ( 'NONE', #16427, 1.000000000000000888 ) ;
#14558 = CARTESIAN_POINT ( 'NONE',  ( 18.84567888139550718, -29.34375185562582899, 11.00000000000044231 ) ) ;
#14559 = VECTOR ( 'NONE', #9066, 1000.000000000000000 ) ;
#14560 = VERTEX_POINT ( 'NONE', #25603 ) ;
#14561 = CARTESIAN_POINT ( 'NONE',  ( 8.411683849014126579, 19.76687823897103868, 7.000000000000000000 ) ) ;
#14562 = EDGE_CURVE ( 'NONE', #21540, #23066, #9778, .T. ) ;
#14563 = DIRECTION ( 'NONE',  ( -0.000000000000000000, 0.000000000000000000, 1.000000000000000000 ) ) ;
#14564 = ORIENTED_EDGE ( 'NONE', *, *, #31537, .F. ) ;
#14565 = AXIS2_PLACEMENT_3D ( 'NONE', #6411, #12122, #25105 ) ;
#14566 = ADVANCED_FACE ( 'NONE', ( #28057 ), #3277, .F. ) ;
#14567 = CARTESIAN_POINT ( 'NONE',  ( -0.3972110264143906000, 20.50537081352338475, -30.00000000000000355 ) ) ;
#14568 = LINE ( 'NONE', #11919, #23076 ) ;
#14569 = CARTESIAN_POINT ( 'NONE',  ( -13.14827996435949053, 25.72067290776677950, 9.500000000000000000 ) ) ;
#14570 = EDGE_CURVE ( 'NONE', #10495, #12849, #1826, .T. ) ;
#14571 = DIRECTION ( 'NONE',  ( 0.000000000000000000, 0.000000000000000000, 1.000000000000000000 ) ) ;
#14572 = CARTESIAN_POINT ( 'NONE',  ( 1.247466774197339978, 28.36888560440311480, 13.00000000000000178 ) ) ;
#14573 = LINE ( 'NONE', #20270, #23646 ) ;
#14574 = CARTESIAN_POINT ( 'NONE',  ( 10.44103466624280685, 32.57396620494213124, 7.499999999999997335 ) ) ;
#14575 = CIRCLE ( 'NONE', #37281, 0.5000000000000004441 ) ;
#14576 = CARTESIAN_POINT ( 'NONE',  ( 14.21588428194489673, 27.70830296778597557, -9.610143119930103950 ) ) ;
#14577 = DIRECTION ( 'NONE',  ( 1.000000000000000000, 0.000000000000000000, 0.000000000000000000 ) ) ;
#14578 = ORIENTED_EDGE ( 'NONE', *, *, #17226, .F. ) ;
#14579 = EDGE_CURVE ( 'NONE', #9314, #34341, #40084, .T. ) ;
#14581 = DIRECTION ( 'NONE',  ( -0.000000000000000000, -0.000000000000000000, 1.000000000000000000 ) ) ;
#14580 = CARTESIAN_POINT ( 'NONE',  ( -17.46026703879977049, 13.44560834044810704, -20.08683738022571319 ) ) ;
#14582 = CARTESIAN_POINT ( 'NONE',  ( -0.4999999999999998890, 37.23829181892400442, 10.94387467463335462 ) ) ;
#14583 = CARTESIAN_POINT ( 'NONE',  ( 14.08258714517840637, -24.61786426002636929, -12.54774028598870395 ) ) ;
#14584 = CARTESIAN_POINT ( 'NONE',  ( -13.88403039571018560, 27.53692605078189715, 10.94611345180490503 ) ) ;
#14585 = CARTESIAN_POINT ( 'NONE',  ( 12.91504324178902152, 21.67529910927544634, -17.43456327316026844 ) ) ;
#14586 = CIRCLE ( 'NONE', #4860, 18.00000000000000000 ) ;
#14587 = PLANE ( 'NONE',  #7523 ) ;
#14588 = CARTESIAN_POINT ( 'NONE',  ( 33.75875814100317029, 2.759858869446390361, 11.00000000000000000 ) ) ;
#14589 = CONICAL_SURFACE ( 'NONE', #25590, 0.4999999999999897304, 0.7853981633974529419 ) ;
#14590 = CARTESIAN_POINT ( 'NONE',  ( -16.24747610076109439, -13.49626370421807309, -26.31547060377475944 ) ) ;
#14591 = CARTESIAN_POINT ( 'NONE',  ( 4.290221133370377693, -20.29569990938377089, -26.55723615674921945 ) ) ;
#14592 = CARTESIAN_POINT ( 'NONE',  ( 15.52046154931812261, 26.41174381453696540, -5.474116501232952459 ) ) ;
#14593 = CARTESIAN_POINT ( 'NONE',  ( 20.29313191480849099, 11.31791106737759556, -14.92333789774876607 ) ) ;
#14594 = CARTESIAN_POINT ( 'NONE',  ( -0.5000000000000005551, 33.00000000000000000, 10.50000000000000000 ) ) ;
#14595 = ORIENTED_EDGE ( 'NONE', *, *, #20302, .T. ) ;
#14596 = CARTESIAN_POINT ( 'NONE',  ( -4.675295383163502017, 19.96902330696676131, -29.23835142064850956 ) ) ;
#14597 = EDGE_CURVE ( 'NONE', #8691, #14016, #28658, .T. ) ;
#14598 = EDGE_LOOP ( 'NONE', ( #15819, #38224, #108, #4475 ) ) ;
#14599 = EDGE_CURVE ( 'NONE', #6144, #19765, #15443, .T. ) ;
#14600 = CARTESIAN_POINT ( 'NONE',  ( -22.71454497019444574, 13.11424865306021914, 13.92931973827808889 ) ) ;
#14601 = ORIENTED_EDGE ( 'NONE', *, *, #14856, .F. ) ;
#14602 = DIRECTION ( 'NONE',  ( 0.000000000000000000, 0.000000000000000000, 1.000000000000000000 ) ) ;
#14603 = LINE ( 'NONE', #20503, #38145 ) ;
#14604 = EDGE_LOOP ( 'NONE', ( #15776, #11, #34693, #1811 ) ) ;
#14605 = CARTESIAN_POINT ( 'NONE',  ( -27.59216913682209338, 0.3852774775313504430, -13.52450996651226411 ) ) ;
#14606 = EDGE_LOOP ( 'NONE', ( #36834, #31732, #13069, #26986, #25372 ) ) ;
#14607 = CARTESIAN_POINT ( 'NONE',  ( 35.47189031372824530, -10.73249152999393097, -5.870541421840872687 ) ) ;
#14608 = VECTOR ( 'NONE', #28610, 1000.000000000000000 ) ;
#14609 = ORIENTED_EDGE ( 'NONE', *, *, #29796, .F. ) ;
#14610 = LINE ( 'NONE', #14002, #21913 ) ;
#14611 = VERTEX_POINT ( 'NONE', #28456 ) ;
#14612 = CARTESIAN_POINT ( 'NONE',  ( -10.49474413300071340, 21.89971208337387765, 11.00000000000000000 ) ) ;
#14613 = DIRECTION ( 'NONE',  ( -0.000000000000000000, -0.000000000000000000, -1.000000000000000000 ) ) ;
#14614 = EDGE_CURVE ( 'NONE', #32024, #14045, #13015, .T. ) ;
#14615 = AXIS2_PLACEMENT_3D ( 'NONE', #24954, #12956, #4008 ) ;
#14616 = VECTOR ( 'NONE', #27720, 1000.000000000000000 ) ;
#14617 = CARTESIAN_POINT ( 'NONE',  ( 9.625795778761983001, 10.95253033666821274, 10.49999999999999645 ) ) ;
#14618 = ORIENTED_EDGE ( 'NONE', *, *, #1677, .F. ) ;
#14619 = EDGE_CURVE ( 'NONE', #28635, #19790, #14144, .T. ) ;
#14620 = DIRECTION ( 'NONE',  ( -0.8090169943749426773, 0.5877852522924796874, 0.000000000000000000 ) ) ;
#14621 = DIRECTION ( 'NONE',  ( 0.000000000000000000, 0.000000000000000000, 1.000000000000000000 ) ) ;
#14622 = CARTESIAN_POINT ( 'NONE',  ( -10.29511041547401717, 24.79362192464190073, 10.50000000000000000 ) ) ;
#14623 = CARTESIAN_POINT ( 'NONE',  ( 18.57748288431603712, 16.38268946942090309, -10.84922581770859296 ) ) ;
#14624 = CARTESIAN_POINT ( 'NONE',  ( 10.11190604682229299, 28.56348632143605926, -14.02879073800986909 ) ) ;
#14625 = VERTEX_POINT ( 'NONE', #22158 ) ;
#14626 = EDGE_CURVE ( 'NONE', #7898, #13849, #31706, .T. ) ;
#14627 = CARTESIAN_POINT ( 'NONE',  ( -19.38332915818774893, 8.712623186017649957, -23.31311828547350018 ) ) ;
#14628 = DIRECTION ( 'NONE',  ( 1.000000000000000000, 0.000000000000000000, 0.000000000000000000 ) ) ;
#14629 = DIRECTION ( 'NONE',  ( 1.000000000000000000, 0.000000000000000000, 0.000000000000000000 ) ) ;
#14630 = CARTESIAN_POINT ( 'NONE',  ( 12.09766887496989085, -21.47150019090766548, -18.42868602394403155 ) ) ;
#14631 = FACE_OUTER_BOUND ( 'NONE', #3722, .T. ) ;
#14632 = CARTESIAN_POINT ( 'NONE',  ( -9.221287281574667816, 10.65863771052210041, 10.63089969389957190 ) ) ;
#14633 = CARTESIAN_POINT ( 'NONE',  ( -11.29646106035690245, 18.04863004157237327, -25.01271745524739387 ) ) ;
#14634 = CARTESIAN_POINT ( 'NONE',  ( 10.63490610281069770, -21.58777382264839062, -18.57263060209788108 ) ) ;
#14635 = LINE ( 'NONE', #33539, #11455 ) ;
#14636 = ORIENTED_EDGE ( 'NONE', *, *, #2120, .T. ) ;
#14637 = ORIENTED_EDGE ( 'NONE', *, *, #19413, .F. ) ;
#14638 = CARTESIAN_POINT ( 'NONE',  ( -11.86532622451750107, 33.05761182678129728, -6.331822098149086919 ) ) ;
#14639 = AXIS2_PLACEMENT_3D ( 'NONE', #25313, #32215, #37711 ) ;
#14640 = CARTESIAN_POINT ( 'NONE',  ( -10.39021566973305788, 20.90519018800560858, 10.50000000000000000 ) ) ;
#14641 = CARTESIAN_POINT ( 'NONE',  ( -12.62480652560827110, 14.42233381811242410, 10.49999999999999822 ) ) ;
#14642 = EDGE_CURVE ( 'NONE', #21611, #16076, #6983, .T. ) ;
#14643 = VECTOR ( 'NONE', #23260, 1000.000000000000000 ) ;
#14644 = VECTOR ( 'NONE', #39667, 1000.000000000000000 ) ;
#14645 = FACE_OUTER_BOUND ( 'NONE', #847, .T. ) ;
#14646 = EDGE_LOOP ( 'NONE', ( #11814, #243, #34942, #27549 ) ) ;
#14647 = CARTESIAN_POINT ( 'NONE',  ( 29.51458379201200088, 0.1415349160452132049, -10.18257699856247278 ) ) ;
#14648 = DIRECTION ( 'NONE',  ( 0.000000000000000000, 0.000000000000000000, 1.000000000000000000 ) ) ;
#14649 = CARTESIAN_POINT ( 'NONE',  ( 10.44103466624280685, 32.57396620494213124, 7.000000000000000000 ) ) ;
#14650 = DIRECTION ( 'NONE',  ( -0.5877852522924796874, -0.8090169943749425663, 0.000000000000000000 ) ) ;
#14651 = ORIENTED_EDGE ( 'NONE', *, *, #5090, .T. ) ;
#14652 = CARTESIAN_POINT ( 'NONE',  ( -20.81523479917187203, 0.8345188516400835477, -26.83090836434666215 ) ) ;
#14653 = DIRECTION ( 'NONE',  ( 1.000000000000000000, 0.000000000000000000, 0.000000000000000000 ) ) ;
#14654 = EDGE_LOOP ( 'NONE', ( #28963, #24661, #19696, #17262 ) ) ;
#14655 = CARTESIAN_POINT ( 'NONE',  ( 29.45872667429271630, -4.364009981319033393, -14.09197514256877426 ) ) ;
#14656 = CARTESIAN_POINT ( 'NONE',  ( 24.55877074690983619, -28.27742302307296995, 13.32518128616626107 ) ) ;
#14657 = EDGE_LOOP ( 'NONE', ( #548, #29340, #37138, #29448 ) ) ;
#14658 = CARTESIAN_POINT ( 'NONE',  ( -12.92634929828533075, 33.47249571006609870, 15.13084544680222976 ) ) ;
#14659 = CARTESIAN_POINT ( 'NONE',  ( -16.80389827881347031, -21.64427909825749197, 19.99202127657103389 ) ) ;
#14660 = CARTESIAN_POINT ( 'NONE',  ( -37.49625565938783467, -14.69322820095469240, -5.000000000000008882 ) ) ;
#14661 = CARTESIAN_POINT ( 'NONE',  ( 1.971557875515494329, 31.43880600153373095, 20.50957957746028271 ) ) ;
#14662 = DIRECTION ( 'NONE',  ( -0.9781476007338070211, -0.2079116908177534029, 0.000000000000000000 ) ) ;
#14663 = ORIENTED_EDGE ( 'NONE', *, *, #20355, .F. ) ;
#14664 = EDGE_CURVE ( 'NONE', #31065, #34172, #3477, .T. ) ;
#14665 = CARTESIAN_POINT ( 'NONE',  ( -13.29616015536805662, -18.15165799370312882, -30.00000000000000711 ) ) ;
#14666 = DIRECTION ( 'NONE',  ( -0.000000000000000000, -0.000000000000000000, 1.000000000000000000 ) ) ;
#14667 = AXIS2_PLACEMENT_3D ( 'NONE', #4532, #33183, #4939 ) ;
#14668 = CIRCLE ( 'NONE', #4922, 0.5000000000000004441 ) ;
#14669 = CARTESIAN_POINT ( 'NONE',  ( 3.426279686912360400, 21.12864742734303292, -25.63660972253196846 ) ) ;
#14670 = VECTOR ( 'NONE', #20130, 1000.000000000000000 ) ;
#14671 = CARTESIAN_POINT ( 'NONE',  ( -3.476907992048017260, 18.63850621467409496, 6.000000000000000000 ) ) ;
#14672 = CARTESIAN_POINT ( 'NONE',  ( 19.36000459721918787, -2.857032334477533908, 21.00000000000168399 ) ) ;
#14673 = VECTOR ( 'NONE', #8883, 1000.000000000000114 ) ;
#14674 = CARTESIAN_POINT ( 'NONE',  ( 15.97914833959363357, -22.30600193650763785, -16.12660968148156471 ) ) ;
#14675 = CARTESIAN_POINT ( 'NONE',  ( 7.591957726969091880, 38.93640765974098628, 10.99999999999980282 ) ) ;
#14676 = CARTESIAN_POINT ( 'NONE',  ( 6.651296319737277862, 27.81603774131160023, 9.000000000000001776 ) ) ;
#14677 = DIRECTION ( 'NONE',  ( -0.000000000000000000, 0.000000000000000000, -1.000000000000000000 ) ) ;
#14678 = ORIENTED_EDGE ( 'NONE', *, *, #35669, .T. ) ;
#14679 = CARTESIAN_POINT ( 'NONE',  ( 12.59997131692024297, 21.13310654933077259, -18.44044215902303563 ) ) ;
#14680 = VERTEX_POINT ( 'NONE', #6709 ) ;
#14681 = CARTESIAN_POINT ( 'NONE',  ( -13.30230047454564968, 21.05347397263300380, -17.49821043808168852 ) ) ;
#14682 = CARTESIAN_POINT ( 'NONE',  ( -23.22759628179758096, -23.81077309376850337, 18.87996532025820429 ) ) ;
#14683 = CARTESIAN_POINT ( 'NONE',  ( 3.790080598862314076, 7.986505539068669890, 7.485646746502365723 ) ) ;
#14684 = CARTESIAN_POINT ( 'NONE',  ( 12.45581562386595031, 20.40522463409936904, -19.50774782679574670 ) ) ;
#14685 = VERTEX_POINT ( 'NONE', #3875 ) ;
#14686 = CARTESIAN_POINT ( 'NONE',  ( 32.01702270572438636, -20.29116740411223319, -7.545109314425605618 ) ) ;
#14687 = ORIENTED_EDGE ( 'NONE', *, *, #36568, .T. ) ;
#14689 = CARTESIAN_POINT ( 'NONE',  ( 12.37435565298211415, 15.93301270189216545, 9.500000000000000000 ) ) ;
#14688 = CARTESIAN_POINT ( 'NONE',  ( -12.63529647066861905, 22.12582800369916924, -17.37362551299798596 ) ) ;
#14690 = CARTESIAN_POINT ( 'NONE',  ( -17.87207185564084355, -26.59298717711743976, -8.659308747257311367 ) ) ;
#14691 = CARTESIAN_POINT ( 'NONE',  ( 13.48130249190479191, 27.93180293473185927, 10.50000000000000533 ) ) ;
#14692 = ORIENTED_EDGE ( 'NONE', *, *, #14235, .F. ) ;
#14693 = CARTESIAN_POINT ( 'NONE',  ( -19.74937082396974120, -7.498879515469185186, -26.30929424058608035 ) ) ;
#14694 = CARTESIAN_POINT ( 'NONE',  ( -14.68167628062920826, -25.79242183381518316, -9.711880916258452956 ) ) ;
#14695 = CARTESIAN_POINT ( 'NONE',  ( 23.74914942275252727, -8.582573258223957779, 23.00000000000000000 ) ) ;
#14696 = ORIENTED_EDGE ( 'NONE', *, *, #17243, .T. ) ;
#14697 = CARTESIAN_POINT ( 'NONE',  ( 25.33785701000014612, 2.122015632169762078, -15.59009891290605943 ) ) ;
#14698 = ADVANCED_FACE ( 'NONE', ( #13210 ), #8953, .T. ) ;
#14699 = DIRECTION ( 'NONE',  ( 0.3090169943749572767, 0.9510565162951503115, -0.000000000000000000 ) ) ;
#14700 = DIRECTION ( 'NONE',  ( 1.000000000000000000, 0.000000000000000000, 0.000000000000000000 ) ) ;
#14701 = EDGE_CURVE ( 'NONE', #23066, #23024, #10378, .T. ) ;
#14702 = ORIENTED_EDGE ( 'NONE', *, *, #13011, .F. ) ;
#14703 = CARTESIAN_POINT ( 'NONE',  ( -27.81571540047708879, 0.08885976736978917767, -13.50292438661861638 ) ) ;
#14704 = EDGE_LOOP ( 'NONE', ( #10303, #24453, #38788 ) ) ;
#14705 = CARTESIAN_POINT ( 'NONE',  ( 25.65762806520498529, -0.4781389605788837205, -17.32945229485775229 ) ) ;
#14706 = CIRCLE ( 'NONE', #19892, 17.00000000000000000 ) ;
#14707 = CARTESIAN_POINT ( 'NONE',  ( 27.71565130972682311, -3.171757977843712162, 19.66345542862529072 ) ) ;
#14708 = AXIS2_PLACEMENT_3D ( 'NONE', #20394, #4947, #21576 ) ;
#14709 = ORIENTED_EDGE ( 'NONE', *, *, #16486, .T. ) ;
#14710 = CARTESIAN_POINT ( 'NONE',  ( -26.91927498037264499, 4.412534205184938330, -5.476192048854705341 ) ) ;
#14711 = ADVANCED_FACE ( 'NONE', ( #26212 ), #14222, .F. ) ;
#14712 = CARTESIAN_POINT ( 'NONE',  ( -10.73859285986284640, 31.49625607628545154, 9.500000000000000000 ) ) ;
#14713 = CARTESIAN_POINT ( 'NONE',  ( 6.312035131040564906, 19.41226734497195849, 13.00000000000000178 ) ) ;
#14714 = DIRECTION ( 'NONE',  ( 1.000000000000000000, 1.224646799147353947E-16, -0.000000000000000000 ) ) ;
#14715 = DIRECTION ( 'NONE',  ( -0.3535533905932752852, -0.6123724356957909176, 0.7071067811865499042 ) ) ;
#14716 = DIRECTION ( 'NONE',  ( 1.000000000000000000, 0.000000000000000000, 0.000000000000000000 ) ) ;
#14717 = DIRECTION ( 'NONE',  ( -1.000000000000000000, 0.000000000000000000, 0.000000000000000000 ) ) ;
#14718 = ORIENTED_EDGE ( 'NONE', *, *, #20306, .T. ) ;
#14719 = CARTESIAN_POINT ( 'NONE',  ( -25.95420856792063447, 5.296653683992947670, -7.877654426414621547 ) ) ;
#14720 = CARTESIAN_POINT ( 'NONE',  ( 7.312035131040564906, 19.41226734497195849, 13.00000000000000178 ) ) ;
#14721 = EDGE_CURVE ( 'NONE', #2211, #6988, #11183, .T. ) ;
#14722 = DIRECTION ( 'NONE',  ( -0.2926062055178280108, -0.7622652262560040137, 0.5773502691896330585 ) ) ;
#14723 = CARTESIAN_POINT ( 'NONE',  ( 22.30282066329013446, -21.88865312665271290, -13.92261583855099438 ) ) ;
#14724 = CARTESIAN_POINT ( 'NONE',  ( -8.559512017365658920, 19.71884705062586107, 13.00000000000000178 ) ) ;
#14725 = CARTESIAN_POINT ( 'NONE',  ( -8.910254037844422825, 17.93301270189230223, 10.49999999999999822 ) ) ;
#14726 = CARTESIAN_POINT ( 'NONE',  ( 10.65067361986881700, 17.57180219728759241, -28.69216590317797611 ) ) ;
#14727 = CARTESIAN_POINT ( 'NONE',  ( 4.242543333974329262E-14, -25.63390596715193936, 15.13084544680213739 ) ) ;
#14728 = VERTEX_POINT ( 'NONE', #26615 ) ;
#14730 = AXIS2_PLACEMENT_3D ( 'NONE', #38264, #19571, #10433 ) ;
#14729 = CARTESIAN_POINT ( 'NONE',  ( -13.37529537539570867, 15.55228444284129097, -29.39288029773726052 ) ) ;
#14731 = CARTESIAN_POINT ( 'NONE',  ( -27.57147631791836062, -9.321847555863021384, 20.69868183039745091 ) ) ;
#14732 = CARTESIAN_POINT ( 'NONE',  ( 11.16520467992603294, 20.33931832809677331, 12.00000000000000000 ) ) ;
#14733 = CARTESIAN_POINT ( 'NONE',  ( 12.15072974113908089, 19.90049516934647045, -20.54455445324533258 ) ) ;
#14734 = VERTEX_POINT ( 'NONE', #4878 ) ;
#14735 = CARTESIAN_POINT ( 'NONE',  ( -14.66026487122501543, 21.46189821169957312, 10.96580508970284384 ) ) ;
#14736 = EDGE_LOOP ( 'NONE', ( #17909, #1763, #36937, #16322 ) ) ;
#14738 = CARTESIAN_POINT ( 'NONE',  ( -1.265509184090266137, 8.754836972118123839, 12.00000000000000000 ) ) ;
#14737 = CARTESIAN_POINT ( 'NONE',  ( -14.48563613516329873, 25.10382544214007083, -11.58903774489672500 ) ) ;
#14739 = CARTESIAN_POINT ( 'NONE',  ( -11.60472954253665456, -20.96974312390484130, -19.48931687713154304 ) ) ;
#14740 = LINE ( 'NONE', #21623, #26945 ) ;
#14741 = CIRCLE ( 'NONE', #32929, 1.000000000000000000 ) ;
#14742 = CARTESIAN_POINT ( 'NONE',  ( -28.30349747650313930, -15.93428203292501522, -13.80390666543416955 ) ) ;
#14743 = CARTESIAN_POINT ( 'NONE',  ( -9.169147237707843345, -25.20086482100098024, -7.872094350184594802 ) ) ;
#14744 = CARTESIAN_POINT ( 'NONE',  ( -23.05386822411323422, -7.747535282638357224, 20.99999999999999645 ) ) ;
#14745 = CARTESIAN_POINT ( 'NONE',  ( 12.74585289761866136, 17.86932441180232090, -22.89739794729497646 ) ) ;
#14746 = ORIENTED_EDGE ( 'NONE', *, *, #21554, .T. ) ;
#14747 = CARTESIAN_POINT ( 'NONE',  ( 23.92111322297680687, 6.328116427676794054, -12.80316392715411133 ) ) ;
#14748 = EDGE_CURVE ( 'NONE', #9203, #29069, #10781, .T. ) ;
#14749 = LINE ( 'NONE', #11702, #8960 ) ;
#14750 = CARTESIAN_POINT ( 'NONE',  ( 13.94482798346721175, 26.50521816028912525, 7.500000000000000888 ) ) ;
#14751 = CARTESIAN_POINT ( 'NONE',  ( -2.317734025672944842, 9.191051544684764707, 9.500000000000000000 ) ) ;
#14752 = EDGE_LOOP ( 'NONE', ( #37940, #12995, #31293, #19081 ) ) ;
#14753 = CARTESIAN_POINT ( 'NONE',  ( -20.88471566866979146, -0.5118096901872604132, -26.72609791841199822 ) ) ;
#14754 = CARTESIAN_POINT ( 'NONE',  ( 31.05798941631825727, -0.2002603227334578129, -5.473151826744909521 ) ) ;
#14755 = CARTESIAN_POINT ( 'NONE',  ( -1.500000000000000888, 37.00000000000000711, 7.000000000000000000 ) ) ;
#14756 = ADVANCED_FACE ( 'NONE', ( #17292 ), #29265, .T. ) ;
#14757 = CARTESIAN_POINT ( 'NONE',  ( 23.85459647502799285, -16.20858856896905209, 20.94377226548378346 ) ) ;
#14758 = EDGE_CURVE ( 'NONE', #761, #36183, #13817, .T. ) ;
#14759 = CARTESIAN_POINT ( 'NONE',  ( 22.45323650136968396, -2.382502413133517738, -29.99999999999998934 ) ) ;
#14760 = CARTESIAN_POINT ( 'NONE',  ( 8.410254037844358876, 17.06698729810774395, 10.49999999999999822 ) ) ;
#14761 = AXIS2_PLACEMENT_3D ( 'NONE', #27680, #28077, #18939 ) ;
#14762 = CONICAL_SURFACE ( 'NONE', #23832, 0.5000000000000039968, 0.7853981633974498333 ) ;
#14763 = ORIENTED_EDGE ( 'NONE', *, *, #8892, .F. ) ;
#14764 = CARTESIAN_POINT ( 'NONE',  ( 6.953805871968278929, 30.22298757065274444, 6.000000000000000000 ) ) ;
#14765 = CIRCLE ( 'NONE', #11519, 16.00000000000000000 ) ;
#14766 = AXIS2_PLACEMENT_3D ( 'NONE', #2385, #36507, #24705 ) ;
#14767 = CARTESIAN_POINT ( 'NONE',  ( 4.440829913680675034, 10.60893893836775348, 12.00000000000000000 ) ) ;
#14768 = ORIENTED_EDGE ( 'NONE', *, *, #3242, .T. ) ;
#14769 = CARTESIAN_POINT ( 'NONE',  ( 0.3500065460287011265, 32.44603839567150061, -13.80550477351713390 ) ) ;
#14770 = CARTESIAN_POINT ( 'NONE',  ( -13.48130249190472796, 27.93180293473203690, 10.50000000000000533 ) ) ;
#14771 = EDGE_CURVE ( 'NONE', #30975, #20195, #7923, .T. ) ;
#14772 = CARTESIAN_POINT ( 'NONE',  ( -12.80736835487441816, 15.68301270189233243, 11.00000000000000000 ) ) ;
#14773 = EDGE_CURVE ( 'NONE', #14611, #37418, #38403, .T. ) ;
#14774 = CARTESIAN_POINT ( 'NONE',  ( -16.72075857324140102, 7.444561356925720297, 11.00000000000000000 ) ) ;
#14775 = CARTESIAN_POINT ( 'NONE',  ( 14.36830325120613594, 20.48707633493483371, 7.000000000000000000 ) ) ;
#14776 = DIRECTION ( 'NONE',  ( 0.000000000000000000, 0.000000000000000000, 1.000000000000000000 ) ) ;
#14777 = CARTESIAN_POINT ( 'NONE',  ( 14.48927117870126757, -30.61587158504672246, 22.99999999999999645 ) ) ;
#14778 = CARTESIAN_POINT ( 'NONE',  ( 14.70740557672079518, 28.82247346305062408, -5.465036479938481406 ) ) ;
#14779 = CARTESIAN_POINT ( 'NONE',  ( -7.142883826790117574, 35.69074677139154517, 7.203056206335835654 ) ) ;
#14780 = ORIENTED_EDGE ( 'NONE', *, *, #27135, .F. ) ;
#14782 = DIRECTION ( 'NONE',  ( 0.8153776007405468818, 0.04273212933193557689, 0.5773502691896386096 ) ) ;
#14781 = CARTESIAN_POINT ( 'NONE',  ( -16.44708297367234451, 13.55940066003513955, -23.27598954255405417 ) ) ;
#14783 = CARTESIAN_POINT ( 'NONE',  ( 14.48927117870123027, -30.61587158504688233, 11.00000000000000000 ) ) ;
#14784 = CARTESIAN_POINT ( 'NONE',  ( 9.495448100151719473, -18.16828483302926145, -30.00000000000000000 ) ) ;
#14785 = CARTESIAN_POINT ( 'NONE',  ( 14.28858787313285994, 24.47746469342009235, -12.55008231428945997 ) ) ;
#14786 = CARTESIAN_POINT ( 'NONE',  ( 11.67120187369582851, 18.92585590138232732, -22.73257522065779668 ) ) ;
#14787 = ORIENTED_EDGE ( 'NONE', *, *, #7426, .T. ) ;
#14788 = DIRECTION ( 'NONE',  ( -0.9781476007338069101, -0.2079116908177532641, 0.000000000000000000 ) ) ;
#14789 = CARTESIAN_POINT ( 'NONE',  ( -2.256323172317922232, 14.28970123917155277, 9.000000000000001776 ) ) ;
#14790 = VECTOR ( 'NONE', #33936, 1000.000000000000000 ) ;
#14791 = CARTESIAN_POINT ( 'NONE',  ( -17.48025379037459714, -14.52550820055553160, -23.07137230154036800 ) ) ;
#14792 = CARTESIAN_POINT ( 'NONE',  ( 4.646166367048098600, -21.13261100285546945, -22.14179161734661605 ) ) ;
#14793 = CARTESIAN_POINT ( 'NONE',  ( 15.07117766819621885, 24.92558405637350560, -10.19323716522371726 ) ) ;
#14794 = CARTESIAN_POINT ( 'NONE',  ( 19.35936484833087690, 11.87520330856569650, -16.98394864372990654 ) ) ;
#14795 = DIRECTION ( 'NONE',  ( 0.000000000000000000, 0.000000000000000000, 1.000000000000000000 ) ) ;
#14796 = CARTESIAN_POINT ( 'NONE',  ( -4.200723223758354052, 37.83089482203977383, -6.281056964556750444 ) ) ;
#14797 = CIRCLE ( 'NONE', #2473, 0.5000000000000001110 ) ;
#14798 = ORIENTED_EDGE ( 'NONE', *, *, #11042, .F. ) ;
#14799 = EDGE_CURVE ( 'NONE', #6629, #39920, #6846, .T. ) ;
#14800 = AXIS2_PLACEMENT_3D ( 'NONE', #5802, #15342, #5600 ) ;
#14801 = CARTESIAN_POINT ( 'NONE',  ( -24.45776404695687489, 8.140618660888312874, 15.72805884749016414 ) ) ;
#14802 = ORIENTED_EDGE ( 'NONE', *, *, #30259, .T. ) ;
#14803 = DIRECTION ( 'NONE',  ( 0.000000000000000000, 0.000000000000000000, 1.000000000000000000 ) ) ;
#14804 = CARTESIAN_POINT ( 'NONE',  ( -8.118377661053486349, 10.47536095541708967, 11.00000000000000000 ) ) ;
#14805 = CARTESIAN_POINT ( 'NONE',  ( -30.65045886600562852, 0.1824153768363431516, -5.946136105496247382 ) ) ;
#14806 = CARTESIAN_POINT ( 'NONE',  ( 22.47955544282887530, -6.794619135805436194, -22.00045867376432795 ) ) ;
#14807 = EDGE_LOOP ( 'NONE', ( #38772, #16196, #37952 ) ) ;
#14808 = FACE_OUTER_BOUND ( 'NONE', #30554, .T. ) ;
#14809 = ORIENTED_EDGE ( 'NONE', *, *, #1682, .F. ) ;
#14810 = CARTESIAN_POINT ( 'NONE',  ( -2.421689871081829537, 8.701977744317861863, 7.000000000000000000 ) ) ;
#14811 = CARTESIAN_POINT ( 'NONE',  ( 11.78893975237933134, 23.27376113029817617, 6.000000000000000000 ) ) ;
#14812 = AXIS2_PLACEMENT_3D ( 'NONE', #6635, #34886, #31435 ) ;
#14813 = CIRCLE ( 'NONE', #27168, 1.000000000000000888 ) ;
#14814 = CARTESIAN_POINT ( 'NONE',  ( 9.697889840765411051, 31.90483559858327212, 9.500000000000000000 ) ) ;
#14815 = ORIENTED_EDGE ( 'NONE', *, *, #15702, .T. ) ;
#14816 =( LENGTH_UNIT ( ) NAMED_UNIT ( * ) SI_UNIT ( .MILLI., .METRE. ) );
#14817 = CYLINDRICAL_SURFACE ( 'NONE', #23044, 17.00000000000000000 ) ;
#14818 = LINE ( 'NONE', #27207, #35125 ) ;
#14819 = AXIS2_PLACEMENT_3D ( 'NONE', #30849, #12352, #21697 ) ;
#14820 = CARTESIAN_POINT ( 'NONE',  ( 8.412270287199559604, 10.07085245822950981, 7.000000000000000000 ) ) ;
#14821 = CARTESIAN_POINT ( 'NONE',  ( 18.98065206215026990, -15.49966443493606327, -20.77364446795738218 ) ) ;
#14822 = EDGE_CURVE ( 'NONE', #30937, #6233, #32110, .T. ) ;
#14823 = CARTESIAN_POINT ( 'NONE',  ( 19.37072484188776400, 15.75976958111966297, -8.396351507073255505 ) ) ;
#14824 = AXIS2_PLACEMENT_3D ( 'NONE', #39622, #39022, #5299 ) ;
#14825 = CARTESIAN_POINT ( 'NONE',  ( 7.999721452599430016, 22.53002257771371220, -21.05289303791193234 ) ) ;
#14826 = ORIENTED_EDGE ( 'NONE', *, *, #38694, .F. ) ;
#14827 = CARTESIAN_POINT ( 'NONE',  ( -22.33890996451869171, 10.80501728358744984, -6.452941623317727249 ) ) ;
#14828 = DIRECTION ( 'NONE',  ( -0.000000000000000000, -0.000000000000000000, -1.000000000000000000 ) ) ;
#14829 = CARTESIAN_POINT ( 'NONE',  ( -14.81908441805110854, 20.17630175058580022, 7.455686640544910482 ) ) ;
#14830 = CARTESIAN_POINT ( 'NONE',  ( 15.58441477488922366, -26.56835683918586710, -7.350884426725713183 ) ) ;
#14831 = CARTESIAN_POINT ( 'NONE',  ( -10.44103466624267185, 32.57396620494226624, 7.500000000000004441 ) ) ;
#14832 = CARTESIAN_POINT ( 'NONE',  ( 7.111215932167702647, 17.81698729810774751, 7.000000000000000000 ) ) ;
#14833 = CARTESIAN_POINT ( 'NONE',  ( -11.09393661379458074, 17.63453714546405848, -26.82748596485767933 ) ) ;
#14834 = CARTESIAN_POINT ( 'NONE',  ( -23.72113249276927505, -26.46856040302326463, -6.759642254155505903 ) ) ;
#14835 = CARTESIAN_POINT ( 'NONE',  ( 12.99674836092793839, -24.46215500157558864, -12.58877913748062127 ) ) ;
#14836 = DIRECTION ( 'NONE',  ( -0.9135454576426059736, -0.4067366430757889395, 0.000000000000000000 ) ) ;
#14837 = ORIENTED_EDGE ( 'NONE', *, *, #11269, .F. ) ;
#14838 = ORIENTED_EDGE ( 'NONE', *, *, #3566, .T. ) ;
#14839 = CARTESIAN_POINT ( 'NONE',  ( -9.393194761908011614, 23.60535835710769703, -19.02674971333937037 ) ) ;
#14840 = CYLINDRICAL_SURFACE ( 'NONE', #32245, 1.000000000000000888 ) ;
#14841 = EDGE_CURVE ( 'NONE', #29462, #3976, #36719, .T. ) ;
#14842 = AXIS2_PLACEMENT_3D ( 'NONE', #32482, #4233, #7267 ) ;
#14843 = AXIS2_PLACEMENT_3D ( 'NONE', #28808, #19875, #10323 ) ;
#14844 = DIRECTION ( 'NONE',  ( 0.9510565162951541973, 0.3090169943749456194, 6.938893903907225222E-15 ) ) ;
#14845 = ORIENTED_EDGE ( 'NONE', *, *, #27631, .F. ) ;
#14846 = CARTESIAN_POINT ( 'NONE',  ( 29.93839244934208921, 0.08748910287391382934, -9.239377091290068122 ) ) ;
#14847 = EDGE_CURVE ( 'NONE', #29442, #7930, #15949, .T. ) ;
#14848 = CARTESIAN_POINT ( 'NONE',  ( -14.47283171447380390, 21.48159823030330884, 7.000000000000000000 ) ) ;
#14849 = DIRECTION ( 'NONE',  ( 0.000000000000000000, 0.000000000000000000, -1.000000000000000000 ) ) ;
#14850 = AXIS2_PLACEMENT_3D ( 'NONE', #39439, #36400, #5507 ) ;
#14851 = ORIENTED_EDGE ( 'NONE', *, *, #8912, .F. ) ;
#14852 = CARTESIAN_POINT ( 'NONE',  ( -30.76822878952619433, -0.006411674588949102180, -6.417027793339856068 ) ) ;
#14853 = CARTESIAN_POINT ( 'NONE',  ( 12.30736835487432579, 14.81698729810772619, 9.000000000000001776 ) ) ;
#14854 = ORIENTED_EDGE ( 'NONE', *, *, #9008, .F. ) ;
#14855 = CARTESIAN_POINT ( 'NONE',  ( 20.30048362414427743, -2.857582090605152558, -29.99999999999998579 ) ) ;
#14856 = EDGE_CURVE ( 'NONE', #22181, #36614, #9199, .T. ) ;
#14857 = CARTESIAN_POINT ( 'NONE',  ( 28.08361064019556963, -26.79812557672064344, 13.32518128616591113 ) ) ;
#14858 = VERTEX_POINT ( 'NONE', #19513 ) ;
#14859 = CARTESIAN_POINT ( 'NONE',  ( -7.360725290689154932, 38.43561981343043499, 13.92931973827797165 ) ) ;
#14860 = CARTESIAN_POINT ( 'NONE',  ( 17.42101839920520590, -19.25229542401946148, 20.69868183039781329 ) ) ;
#14861 = FACE_OUTER_BOUND ( 'NONE', #29110, .T. ) ;
#14862 = CARTESIAN_POINT ( 'NONE',  ( 9.555312204552503630, 25.15592819202958808, 20.25080042701566541 ) ) ;
#14863 = CARTESIAN_POINT ( 'NONE',  ( 3.992867117591230919, 8.524771480177550487, 10.49999999999999289 ) ) ;
#14864 = ORIENTED_EDGE ( 'NONE', *, *, #12704, .F. ) ;
#14865 = CARTESIAN_POINT ( 'NONE',  ( -12.55429062395158901, 25.98950339719647573, 18.87996532025784191 ) ) ;
#14866 = DIRECTION ( 'NONE',  ( -0.9945218953682727347, 0.1045284632676597436, 0.000000000000000000 ) ) ;
#14867 = EDGE_CURVE ( 'NONE', #18426, #34264, #26006, .T. ) ;
#14868 = EDGE_CURVE ( 'NONE', #4736, #25935, #13350, .T. ) ;
#14869 = AXIS2_PLACEMENT_3D ( 'NONE', #8490, #33088, #36126 ) ;
#14871 = VECTOR ( 'NONE', #9073, 1000.000000000000000 ) ;
#14870 = CARTESIAN_POINT ( 'NONE',  ( 3.279674764711695722, 20.24540435116753301, -29.22490024661859920 ) ) ;
#14872 = DIRECTION ( 'NONE',  ( -1.000000000000000000, 0.000000000000000000, 0.000000000000000000 ) ) ;
#14873 = CARTESIAN_POINT ( 'NONE',  ( 9.534329713526908279, 19.05805734587007549, 20.69868183039784881 ) ) ;
#14874 = CARTESIAN_POINT ( 'NONE',  ( 13.35105216789999716, -17.76889701558443591, -23.46262091258972049 ) ) ;
#14875 = DIRECTION ( 'NONE',  ( 0.2079116908177663092, 0.9781476007338041345, 0.000000000000000000 ) ) ;
#14876 = AXIS2_PLACEMENT_3D ( 'NONE', #15010, #11372, #29648 ) ;
#14877 = LINE ( 'NONE', #24413, #17071 ) ;
#14878 = LINE ( 'NONE', #24015, #21362 ) ;
#14879 = ORIENTED_EDGE ( 'NONE', *, *, #37893, .F. ) ;
#14880 = CARTESIAN_POINT ( 'NONE',  ( 12.35228433879287380, 20.54234309038960049, -19.48813501896534817 ) ) ;
#14881 = ORIENTED_EDGE ( 'NONE', *, *, #13491, .F. ) ;
#14882 = CARTESIAN_POINT ( 'NONE',  ( -11.45248459189543588, 17.05290680873532239, -28.72504823342588409 ) ) ;
#14883 = CARTESIAN_POINT ( 'NONE',  ( -33.10646761238943014, -9.521241417581261857, 18.42518152272108978 ) ) ;
#14884 = CARTESIAN_POINT ( 'NONE',  ( -14.42035624161473883, 26.65972665747678150, 10.63089969389956835 ) ) ;
#14885 = CARTESIAN_POINT ( 'NONE',  ( 13.00369382996352563, 21.53152199447597326, -17.45016979600528018 ) ) ;
#14886 = ORIENTED_EDGE ( 'NONE', *, *, #3441, .T. ) ;
#14887 = CARTESIAN_POINT ( 'NONE',  ( 18.96300721855776317, -11.21761247941028650, -24.21598040740967406 ) ) ;
#14888 = ORIENTED_EDGE ( 'NONE', *, *, #19803, .F. ) ;
#14890 = CARTESIAN_POINT ( 'NONE',  ( 8.172817770806538817, 10.40043057260416504, 10.99387789255783510 ) ) ;
#14889 = CARTESIAN_POINT ( 'NONE',  ( -10.67640217097355482, 17.76288147141041662, -27.41698759738607194 ) ) ;
#14891 = CARTESIAN_POINT ( 'NONE',  ( -17.17635872890215509, -26.93998231148862743, -6.852558094669841893 ) ) ;
#14892 = EDGE_CURVE ( 'NONE', #36134, #13548, #13417, .T. ) ;
#14893 = CARTESIAN_POINT ( 'NONE',  ( 13.64210930126480115, 24.20081211342298744, 13.00000000000000178 ) ) ;
#14894 = EDGE_LOOP ( 'NONE', ( #16204, #31901, #1862, #5655, #39619 ) ) ;
#14895 = CARTESIAN_POINT ( 'NONE',  ( -35.43763548776691863, -11.07137260576668147, -5.869669228994635723 ) ) ;
#14896 = CARTESIAN_POINT ( 'NONE',  ( -9.345945910616261898, -18.29489296895642880, -28.71376903915567880 ) ) ;
#14897 = DIRECTION ( 'NONE',  ( 1.000000000000000000, 0.000000000000000000, 0.000000000000000000 ) ) ;
#14898 = ORIENTED_EDGE ( 'NONE', *, *, #9288, .T. ) ;
#14899 = CARTESIAN_POINT ( 'NONE',  ( 29.75447456610766750, 1.108193808558314508, -5.946487029707098415 ) ) ;
#14900 = EDGE_CURVE ( 'NONE', #22179, #18984, #4481, .T. ) ;
#14901 = CARTESIAN_POINT ( 'NONE',  ( -8.258442077957658611, 10.28257882428884606, 10.94387467463491248 ) ) ;
#14902 = DIRECTION ( 'NONE',  ( -0.000000000000000000, -0.000000000000000000, 1.000000000000000000 ) ) ;
#14903 = ORIENTED_EDGE ( 'NONE', *, *, #38076, .T. ) ;
#14904 = CARTESIAN_POINT ( 'NONE',  ( -21.72248880293610185, 0.6579594075278962784, -23.84550374915839654 ) ) ;
#14905 = EDGE_LOOP ( 'NONE', ( #22587, #14, #6879 ) ) ;
#14906 = CARTESIAN_POINT ( 'NONE',  ( 31.51816681948337617, -1.356210769490176160, -8.235438873524525860 ) ) ;
#14907 = CIRCLE ( 'NONE', #20739, 1.000000000000000888 ) ;
#14908 = CARTESIAN_POINT ( 'NONE',  ( 29.67744882843222243, -20.56940131916748626, 18.42518152272146637 ) ) ;
#14909 = EDGE_LOOP ( 'NONE', ( #12793, #30282, #32727 ) ) ;
#14910 = CARTESIAN_POINT ( 'NONE',  ( -26.55795656307421027, 3.516599515638362927, -10.75008132255575433 ) ) ;
#14911 = VECTOR ( 'NONE', #39985, 1000.000000000000000 ) ;
#14912 = DIRECTION ( 'NONE',  ( -0.000000000000000000, -0.000000000000000000, -1.000000000000000000 ) ) ;
#14913 = DIRECTION ( 'NONE',  ( -1.000000000000000000, 0.000000000000000000, 0.000000000000000000 ) ) ;
#14914 = CARTESIAN_POINT ( 'NONE',  ( -14.26585111513660031, 17.86474508437623143, 12.00000000000000000 ) ) ;
#14915 = DIRECTION ( 'NONE',  ( -0.000000000000000000, -0.000000000000000000, -1.000000000000000000 ) ) ;
#14916 = CARTESIAN_POINT ( 'NONE',  ( -11.39464589777670867, 26.66807349098043289, 12.00000000000000000 ) ) ;
#14917 = PLANE ( 'NONE',  #39924 ) ;
#14918 = VERTEX_POINT ( 'NONE', #10985 ) ;
#14919 = CARTESIAN_POINT ( 'NONE',  ( -23.41974574084031246, 6.012251731081178718, -14.80241686762865605 ) ) ;
#14920 = CYLINDRICAL_SURFACE ( 'NONE', #6007, 1.000000000000000000 ) ;
#14921 = DIRECTION ( 'NONE',  ( 0.000000000000000000, 0.000000000000000000, 1.000000000000000000 ) ) ;
#14922 = CARTESIAN_POINT ( 'NONE',  ( 25.29206606878849328, -26.20377346906149185, -5.444282035157826272 ) ) ;
#14923 = EDGE_CURVE ( 'NONE', #659, #34496, #29862, .T. ) ;
#14924 = CARTESIAN_POINT ( 'NONE',  ( -12.05736835487443237, 14.38397459621567442, 7.499999999999993783 ) ) ;
#14925 = CARTESIAN_POINT ( 'NONE',  ( 15.05907480041244639, 26.65905605469517781, -8.283340056487517700 ) ) ;
#14926 = CARTESIAN_POINT ( 'NONE',  ( -5.121747905603520223, -25.93120163663720845, 14.53008259254011136 ) ) ;
#14927 = AXIS2_PLACEMENT_3D ( 'NONE', #23162, #7722, #32525 ) ;
#14928 = ORIENTED_EDGE ( 'NONE', *, *, #13593, .T. ) ;
#14929 = CARTESIAN_POINT ( 'NONE',  ( -15.20187259911379662, 18.82279879278276269, -16.71752878418681476 ) ) ;
#14930 = CARTESIAN_POINT ( 'NONE',  ( -25.92581632124343471, -14.96827703203019766, 20.82122704794079482 ) ) ;
#14931 = LINE ( 'NONE', #21419, #22389 ) ;
#14932 = CARTESIAN_POINT ( 'NONE',  ( 11.70759707017889362, 18.89087562079335569, -22.73869321768459173 ) ) ;
#14933 = ORIENTED_EDGE ( 'NONE', *, *, #38872, .F. ) ;
#14934 = DIRECTION ( 'NONE',  ( 0.5877852522924689183, -0.8090169943749505599, -0.000000000000000000 ) ) ;
#14935 = VECTOR ( 'NONE', #24500, 999.9999999999998863 ) ;
#14936 = ORIENTED_EDGE ( 'NONE', *, *, #1445, .T. ) ;
#14938 = DIRECTION ( 'NONE',  ( 1.000000000000000000, 0.000000000000000000, 0.000000000000000000 ) ) ;
#14937 = CARTESIAN_POINT ( 'NONE',  ( -15.33869540756803751, 26.96259011824205487, -5.943855708106864810 ) ) ;
#14939 = CARTESIAN_POINT ( 'NONE',  ( -9.506566060136700358, -18.16246691004805314, -29.34816978379683050 ) ) ;
#14940 = CARTESIAN_POINT ( 'NONE',  ( -33.75875814100324845, 2.759858869446484064, 11.00000000000000000 ) ) ;
#14941 = CARTESIAN_POINT ( 'NONE',  ( -33.15301329781156170, -17.35959640044362473, -8.406341442035538236 ) ) ;
#14942 = CARTESIAN_POINT ( 'NONE',  ( -10.12595346383139017, -23.38316831488110026, -14.65118248118756306 ) ) ;
#14943 = CARTESIAN_POINT ( 'NONE',  ( 5.034171952702014785, 35.03623199971300295, 7.000000000000000000 ) ) ;
#14944 = CARTESIAN_POINT ( 'NONE',  ( 12.67361812497431295, 18.54269888232404995, -21.74640883014503245 ) ) ;
#14945 = ORIENTED_EDGE ( 'NONE', *, *, #4112, .F. ) ;
#14946 = CARTESIAN_POINT ( 'NONE',  ( 20.30257773999915116, 5.964623025713435389, -24.29955355791028992 ) ) ;
#14947 = DIRECTION ( 'NONE',  ( 1.000000000000000000, 0.000000000000000000, 0.000000000000000000 ) ) ;
#14948 = DIRECTION ( 'NONE',  ( -0.000000000000000000, -0.000000000000000000, -1.000000000000000000 ) ) ;
#14949 = CARTESIAN_POINT ( 'NONE',  ( 0.000000000000000000, 22.50000000000000355, 6.000000000000000000 ) ) ;
#14950 = VERTEX_POINT ( 'NONE', #39805 ) ;
#14951 = CARTESIAN_POINT ( 'NONE',  ( -30.48098785803534483, -0.7257077854517125504, -9.657254528547552397 ) ) ;
#14952 = CARTESIAN_POINT ( 'NONE',  ( 30.87575086445591666, -0.1861898454035852968, -6.883314186587743855 ) ) ;
#14953 = CIRCLE ( 'NONE', #11786, 0.9999999999999994449 ) ;
#14954 = DIRECTION ( 'NONE',  ( 0.000000000000000000, 0.000000000000000000, 1.000000000000000000 ) ) ;
#14955 = CARTESIAN_POINT ( 'NONE',  ( 27.24589233318962656, -6.395442063035704727, 20.50957957746052429 ) ) ;
#14956 = CARTESIAN_POINT ( 'NONE',  ( 37.62663912510992503, -8.659558992827971480, -14.26382729546509687 ) ) ;
#14957 = CARTESIAN_POINT ( 'NONE',  ( 26.45121176803954910, -27.84758587393107021, 10.99999999999999822 ) ) ;
#14958 = ORIENTED_EDGE ( 'NONE', *, *, #13959, .T. ) ;
#14959 = AXIS2_PLACEMENT_3D ( 'NONE', #9967, #230, #16061 ) ;
#14960 = CARTESIAN_POINT ( 'NONE',  ( -7.645071344821658954, 9.594463043616254794, 7.000000000000000000 ) ) ;
#14961 = CARTESIAN_POINT ( 'NONE',  ( 2.229431105722923245, 20.49260818092372460, 12.00000000000000000 ) ) ;
#14962 = DIRECTION ( 'NONE',  ( -0.9135454576426059736, -0.4067366430757888285, 0.000000000000000000 ) ) ;
#14963 = CARTESIAN_POINT ( 'NONE',  ( 2.741814962476898376, 38.30556977738701363, -5.435872072964093249 ) ) ;
#14964 = LINE ( 'NONE', #17635, #30830 ) ;
#14965 = EDGE_CURVE ( 'NONE', #8131, #19420, #3612, .T. ) ;
#14966 = CARTESIAN_POINT ( 'NONE',  ( 14.86556419889026159, 20.43481210330100950, 10.49999999999999822 ) ) ;
#14967 = DIRECTION ( 'NONE',  ( 0.000000000000000000, -0.000000000000000000, -1.000000000000000000 ) ) ;
#14968 = DIRECTION ( 'NONE',  ( -0.000000000000000000, -0.000000000000000000, -1.000000000000000000 ) ) ;
#14969 = CARTESIAN_POINT ( 'NONE',  ( 9.183240348400453001, 28.21559575157615996, 13.00000000000000178 ) ) ;
#14970 = SURFACE_STYLE_FILL_AREA ( #2587 ) ;
#14971 = CARTESIAN_POINT ( 'NONE',  ( 14.85673200164996643, 28.20965467857394771, -6.393760900654135604 ) ) ;
#14972 = DIRECTION ( 'NONE',  ( 0.000000000000000000, 0.000000000000000000, 1.000000000000000000 ) ) ;
#14973 = ORIENTED_EDGE ( 'NONE', *, *, #30221, .F. ) ;
#14974 = CIRCLE ( 'NONE', #23385, 6.000000000000003553 ) ;
#14976 = CARTESIAN_POINT ( 'NONE',  ( -3.503793317224520365, 8.420815634768723967, 11.00000000000000000 ) ) ;
#14975 = CARTESIAN_POINT ( 'NONE',  ( -15.91172688669051283, 12.94523012445180399, -30.00000000000000711 ) ) ;
#14977 = EDGE_CURVE ( 'NONE', #1404, #5091, #35694, .T. ) ;
#14978 = DIRECTION ( 'NONE',  ( 0.000000000000000000, 0.000000000000000000, 1.000000000000000000 ) ) ;
#14979 = AXIS2_PLACEMENT_3D ( 'NONE', #6215, #22051, #18620 ) ;
#14980 = CARTESIAN_POINT ( 'NONE',  ( 9.531353544348123208, -18.20021061595370782, -28.70654323991336909 ) ) ;
#14981 = EDGE_CURVE ( 'NONE', #27240, #35073, #8337, .T. ) ;
#14982 = CARTESIAN_POINT ( 'NONE',  ( 25.98021325959672723, -4.875178728621328617, 20.50957957746028981 ) ) ;
#14983 = CARTESIAN_POINT ( 'NONE',  ( 12.63673072935002573, 21.07828628784659131, -18.44856727879870206 ) ) ;
#14984 = ORIENTED_EDGE ( 'NONE', *, *, #1529, .F. ) ;
#14985 = CARTESIAN_POINT ( 'NONE',  ( 3.100636323082810009, 29.29593658752792962, 13.00000000000000178 ) ) ;
#14986 = CARTESIAN_POINT ( 'NONE',  ( 29.22254796326513926, -28.85350741969417854, 11.00000000000000000 ) ) ;
#14987 = CARTESIAN_POINT ( 'NONE',  ( -22.68080910437082309, -17.76831930014195393, -16.67414630805707887 ) ) ;
#14988 = CARTESIAN_POINT ( 'NONE',  ( 1.539264792407522231, -22.70516402096868092, -16.98615508874380353 ) ) ;
#14989 = CARTESIAN_POINT ( 'NONE',  ( 11.39136839498931408, 17.60508876921546317, -26.24673842913259136 ) ) ;
#14990 = CARTESIAN_POINT ( 'NONE',  ( 17.89753197511066674, 10.02670602479014228, -29.42980511128735444 ) ) ;
#14991 = DIRECTION ( 'NONE',  ( 0.000000000000000000, 0.000000000000000000, 1.000000000000000000 ) ) ;
#14992 = CARTESIAN_POINT ( 'NONE',  ( -2.883099083560371589, 20.54810638744049811, -27.73126374019785345 ) ) ;
#14993 = ORIENTED_EDGE ( 'NONE', *, *, #1200, .T. ) ;
#14994 = CARTESIAN_POINT ( 'NONE',  ( -33.67692147928062241, -6.312519796522384041, -8.978852421033355569 ) ) ;
#14995 = CARTESIAN_POINT ( 'NONE',  ( -22.89849980942928553, 13.22045502901142200, 13.32518128616608699 ) ) ;
#14996 = VERTEX_POINT ( 'NONE', #2445 ) ;
#14997 = CARTESIAN_POINT ( 'NONE',  ( 2.568190708544436873, 12.82247983807080871, 10.50000000000000000 ) ) ;
#14998 = ADVANCED_FACE ( 'NONE', ( #8736 ), #11781, .F. ) ;
#14999 = DIRECTION ( 'NONE',  ( 0.2079116908177663092, 0.9781476007338041345, 0.000000000000000000 ) ) ;
#15000 = EDGE_CURVE ( 'NONE', #7701, #12819, #33131, .T. ) ;
#15001 = CARTESIAN_POINT ( 'NONE',  ( -22.17658030202064978, 0.8441110128694983006, -22.75671850330635237 ) ) ;
#15002 = CARTESIAN_POINT ( 'NONE',  ( 19.45830134839955505, -7.192962728667438022, -27.74412373246262220 ) ) ;
#15003 = AXIS2_PLACEMENT_3D ( 'NONE', #5121, #14262, #4518 ) ;
#15004 = VECTOR ( 'NONE', #18903, 1000.000000000000000 ) ;
#15005 = ORIENTED_EDGE ( 'NONE', *, *, #26901, .T. ) ;
#15006 = CARTESIAN_POINT ( 'NONE',  ( 6.654030453887980201, 35.94335816374507431, 7.500000000000000888 ) ) ;
#15007 = ORIENTED_EDGE ( 'NONE', *, *, #33226, .T. ) ;
#15008 = FACE_OUTER_BOUND ( 'NONE', #3741, .T. ) ;
#15009 = DIRECTION ( 'NONE',  ( -0.8660254037844432595, -0.4999999999999920619, 0.000000000000000000 ) ) ;
#15010 = CARTESIAN_POINT ( 'NONE',  ( -4.458872323573595864, 26.51478363815348160, 12.00000000000000000 ) ) ;
#15011 = EDGE_LOOP ( 'NONE', ( #12225, #26376 ) ) ;
#15012 = CARTESIAN_POINT ( 'NONE',  ( 7.935100905948330841, 11.57827057593817344, 7.000000000000000000 ) ) ;
#15013 = CARTESIAN_POINT ( 'NONE',  ( -14.47283171447380390, 21.48159823030330884, 11.00000000000000000 ) ) ;
#15014 = FACE_OUTER_BOUND ( 'NONE', #2276, .T. ) ;
#15015 = EDGE_CURVE ( 'NONE', #15686, #32385, #2245, .T. ) ;
#15016 = CARTESIAN_POINT ( 'NONE',  ( 30.18422347142476880, -23.20414393450525736, -5.437200421920011628 ) ) ;
#15017 = CARTESIAN_POINT ( 'NONE',  ( 18.14119866732840336, 14.50330093467433556, -15.90978874977256829 ) ) ;
#15018 = CARTESIAN_POINT ( 'NONE',  ( 7.898168204405470405, 20.17838150051020207, -24.60177268676963536 ) ) ;
#15019 = EDGE_LOOP ( 'NONE', ( #25085, #34662, #36468, #27252 ) ) ;
#15020 = CARTESIAN_POINT ( 'NONE',  ( -21.87593696763935824, 10.61463320033040247, -10.38310781559205687 ) ) ;
#15021 = CARTESIAN_POINT ( 'NONE',  ( 0.01803229776516698107, 30.37627742347970283, 12.00000000000000000 ) ) ;
#15022 = LINE ( 'NONE', #24366, #16231 ) ;
#15023 = CARTESIAN_POINT ( 'NONE',  ( 14.74460831617895806, -25.48601742449350738, -10.64559727961380631 ) ) ;
#15024 = CYLINDRICAL_SURFACE ( 'NONE', #39879, 0.4999999999999999445 ) ;
#15025 = CARTESIAN_POINT ( 'NONE',  ( 30.41237130417911771, 3.314011747244134387, -4.999999999999999112 ) ) ;
#15026 = CARTESIAN_POINT ( 'NONE',  ( -11.27968654789714797, 18.06170250143723877, -25.01040361136536561 ) ) ;
#15027 = AXIS2_PLACEMENT_3D ( 'NONE', #8722, #2232, #18272 ) ;
#15028 = CARTESIAN_POINT ( 'NONE',  ( -22.66017947715816661, -25.37253451465284115, -9.858107741291926018 ) ) ;
#15029 = CARTESIAN_POINT ( 'NONE',  ( 10.61360125799510179, -25.41145544430514747, -7.858495472244451996 ) ) ;
#15030 = AXIS2_PLACEMENT_3D ( 'NONE', #12355, #9910, #24553 ) ;
#15031 = DIRECTION ( 'NONE',  ( 0.2079116908177533474, -0.9781476007338067991, 0.000000000000000000 ) ) ;
#15032 = ORIENTED_EDGE ( 'NONE', *, *, #29796, .T. ) ;
#15033 = ORIENTED_EDGE ( 'NONE', *, *, #38895, .T. ) ;
#15034 = CARTESIAN_POINT ( 'NONE',  ( -11.15150138062039709, 34.02824952835918992, -5.000000000000002665 ) ) ;
#15035 = CARTESIAN_POINT ( 'NONE',  ( 0.9438746746263467768, 37.23829181893392359, 10.49999999999999822 ) ) ;
#15036 = DIRECTION ( 'NONE',  ( -0.7431448254773962425, -0.6691306063588561281, -0.000000000000000000 ) ) ;
#15037 = CARTESIAN_POINT ( 'NONE',  ( -9.221287281574667816, 10.65863771052210041, 10.49999999999999822 ) ) ;
#15038 = ORIENTED_EDGE ( 'NONE', *, *, #31617, .T. ) ;
#15039 = CARTESIAN_POINT ( 'NONE',  ( 28.88427010664839045, 0.1085951546874318191, -11.59929086114978247 ) ) ;
#15040 = DIRECTION ( 'NONE',  ( -0.000000000000000000, -0.000000000000000000, -1.000000000000000000 ) ) ;
#15041 = CIRCLE ( 'NONE', #2720, 0.4999999999999995559 ) ;
#15042 = DIRECTION ( 'NONE',  ( -1.000000000000000000, 0.000000000000000000, 0.000000000000000000 ) ) ;
#15043 = EDGE_CURVE ( 'NONE', #257, #14093, #12058, .T. ) ;
#15044 = ORIENTED_EDGE ( 'NONE', *, *, #30204, .T. ) ;
#15045 = CARTESIAN_POINT ( 'NONE',  ( -29.98580443888884162, 0.03576373324625783945, -9.238541745588479515 ) ) ;
#15046 = DIRECTION ( 'NONE',  ( 0.7431448254773954654, 0.6691306063588569053, -0.000000000000000000 ) ) ;
#15047 = VERTEX_POINT ( 'NONE', #24169 ) ;
#15048 = CARTESIAN_POINT ( 'NONE',  ( 33.79624156833973103, -5.123317329496374306, -7.674098321924684107 ) ) ;
#15049 = CARTESIAN_POINT ( 'NONE',  ( 34.92340065173399921, -3.770459477547956517, 14.53008259254010959 ) ) ;
#15050 = ORIENTED_EDGE ( 'NONE', *, *, #29626, .T. ) ;
#15051 = CARTESIAN_POINT ( 'NONE',  ( 1.856244906471662182, 39.65430245495501538, 14.53008259254011314 ) ) ;
#15052 = CARTESIAN_POINT ( 'NONE',  ( 17.00801676780080385, -20.85310720624926262, 20.25080042701566541 ) ) ;
#15053 = CARTESIAN_POINT ( 'NONE',  ( -20.71630303010418572, -29.20803740758281464, -4.999999999999997335 ) ) ;
#15054 = B_SPLINE_CURVE_WITH_KNOTS ( 'NONE', 3,
 ( #12741, #32034, #19044, #7444 ),
 .UNSPECIFIED., .F., .F.,
 ( 4, 4 ),
 ( 0.000000000000000000, 1.000000000000000000 ),
 .UNSPECIFIED. ) ;
#15055 = CARTESIAN_POINT ( 'NONE',  ( 2.325696902088659090, 33.04389473401325006, 19.99202127657102679 ) ) ;
#15056 = APPLICATION_CONTEXT ( 'automotive_design' ) ;
#15057 = DIRECTION ( 'NONE',  ( 0.6691306063588570163, -0.7431448254773952433, 0.000000000000000000 ) ) ;
#15058 = EDGE_LOOP ( 'NONE', ( #8517, #28573, #18553, #19740 ) ) ;
#15059 = CARTESIAN_POINT ( 'NONE',  ( 7.953805871968279817, 30.22298757065274444, 12.00000000000000000 ) ) ;
#15060 = DIRECTION ( 'NONE',  ( 0.000000000000000000, -0.000000000000000000, 1.000000000000000000 ) ) ;
#15061 = ADVANCED_FACE ( 'NONE', ( #8938 ), #28493, .T. ) ;
#15062 = CARTESIAN_POINT ( 'NONE',  ( 3.904167649330699152, 20.20748209445285681, -28.48006849494148796 ) ) ;
#15063 = DIRECTION ( 'NONE',  ( 0.000000000000000000, 0.000000000000000000, 1.000000000000000000 ) ) ;
#15064 = ADVANCED_FACE ( 'NONE', ( #26977 ), #14587, .T. ) ;
#15065 = CARTESIAN_POINT ( 'NONE',  ( 14.06669941890381104, 14.65883224166404730, 19.99202127657115469 ) ) ;
#15066 = VECTOR ( 'NONE', #15151, 1000.000000000000000 ) ;
#15067 = CARTESIAN_POINT ( 'NONE',  ( 10.80806213842329200, -17.72408045989398673, -27.36067723112840255 ) ) ;
#15068 = LINE ( 'NONE', #5922, #15185 ) ;
#15069 = CARTESIAN_POINT ( 'NONE',  ( 13.39463915635820790, 18.33192650902018883, 6.000000000000000000 ) ) ;
#15070 = DIRECTION ( 'NONE',  ( 0.000000000000000000, 0.000000000000000000, 1.000000000000000000 ) ) ;
#15071 = ORIENTED_EDGE ( 'NONE', *, *, #5903, .T. ) ;
#15072 = ORIENTED_EDGE ( 'NONE', *, *, #7809, .T. ) ;
#15073 = CARTESIAN_POINT ( 'NONE',  ( -11.01126394183691737, 17.29167595606526575, -29.99999999999999645 ) ) ;
#15074 = EDGE_CURVE ( 'NONE', #9989, #481, #24534, .T. ) ;
#15075 = VECTOR ( 'NONE', #30785, 1000.000000000000000 ) ;
#15076 = CARTESIAN_POINT ( 'NONE',  ( -21.70015648973560118, -23.40282454538633772, 19.27171037444124480 ) ) ;
#15077 = CARTESIAN_POINT ( 'NONE',  ( 10.18847001889738557, -19.17713045604790167, -23.85841820396901269 ) ) ;
#15078 = CARTESIAN_POINT ( 'NONE',  ( 6.654030453887979313, 35.94335816374508141, 7.000000000000000000 ) ) ;
#15079 = ORIENTED_EDGE ( 'NONE', *, *, #12500, .F. ) ;
#15080 = EDGE_LOOP ( 'NONE', ( #25035, #13034, #27044, #28546, #26798 ) ) ;
#15082 = DIRECTION ( 'NONE',  ( 1.000000000000000000, 0.000000000000000000, 0.000000000000000000 ) ) ;
#15081 = CARTESIAN_POINT ( 'NONE',  ( -14.09379978727693050, 28.77806074224476163, -8.659515015975241425 ) ) ;
#15083 = CARTESIAN_POINT ( 'NONE',  ( -16.21692691291975663, -23.02287499300812357, -15.16141334603994473 ) ) ;
#15084 = CARTESIAN_POINT ( 'NONE',  ( -17.34253826592568970, 27.32041144456614390, -5.000000000000000000 ) ) ;
#15085 = VERTEX_POINT ( 'NONE', #14985 ) ;
#15086 = CARTESIAN_POINT ( 'NONE',  ( -33.27136418661606854, -12.54424548814919937, -10.20349738210835078 ) ) ;
#15087 = CARTESIAN_POINT ( 'NONE',  ( -14.43538540834600603, -25.42431206739405525, -10.65726991915511768 ) ) ;
#15088 = VECTOR ( 'NONE', #30957, 1000.000000000000114 ) ;
#15089 = CARTESIAN_POINT ( 'NONE',  ( 0.5000000000000000000, 37.26099332938166242, 10.94611345180491035 ) ) ;
#15090 = ORIENTED_EDGE ( 'NONE', *, *, #6313, .F. ) ;
#15091 = CARTESIAN_POINT ( 'NONE',  ( 21.37456834929076166, 2.344506045348980994, -24.03039016388560256 ) ) ;
#15092 = FACE_OUTER_BOUND ( 'NONE', #27874, .T. ) ;
#15093 = CARTESIAN_POINT ( 'NONE',  ( -38.66460482714451530, -17.32098561216439947, 11.00000000000000000 ) ) ;
#15094 = EDGE_CURVE ( 'NONE', #2814, #34302, #39363, .T. ) ;
#15095 = EDGE_LOOP ( 'NONE', ( #13997, #16119, #35139, #9561 ) ) ;
#15096 = ADVANCED_FACE ( 'NONE', ( #1795 ), #27627, .T. ) ;
#15097 = CARTESIAN_POINT ( 'NONE',  ( -25.90181000411780943, 0.2561891300705002594, -16.43557158720686573 ) ) ;
#15099 = ADVANCED_FACE ( 'NONE', ( #30230 ), #21279, .T. ) ;
#15098 = ORIENTED_EDGE ( 'NONE', *, *, #39557, .T. ) ;
#15100 = CARTESIAN_POINT ( 'NONE',  ( 26.25999556400573098, -0.3564369614627482807, -16.35972333294595060 ) ) ;
#15101 = VECTOR ( 'NONE', #17179, 1000.000000000000000 ) ;
#15102 = CARTESIAN_POINT ( 'NONE',  ( 32.48981136421910776, -6.600762235922772447, 18.42518152272070608 ) ) ;
#15103 = ORIENTED_EDGE ( 'NONE', *, *, #15043, .F. ) ;
#15104 = CIRCLE ( 'NONE', #13143, 0.5000000000000004441 ) ;
#15105 = CARTESIAN_POINT ( 'NONE',  ( -27.56582635568890183, 2.642126925834923146, -9.763091250748670902 ) ) ;
#15106 = LINE ( 'NONE', #33213, #17754 ) ;
#15107 = CARTESIAN_POINT ( 'NONE',  ( 5.644276917315719899, 36.40655018617690786, 10.49999999999999822 ) ) ;
#15108 = CIRCLE ( 'NONE', #20305, 1.000000000000000000 ) ;
#15109 = CARTESIAN_POINT ( 'NONE',  ( -17.83459896181207682, -17.64923967996745446, 20.94377226548377990 ) ) ;
#15110 = DIRECTION ( 'NONE',  ( 0.9945218953682745111, 0.1045284632676437703, -0.000000000000000000 ) ) ;
#15111 = EDGE_CURVE ( 'NONE', #35073, #25278, #8286, .T. ) ;
#15112 = FACE_BOUND ( 'NONE', #9039, .T. ) ;
#15113 = EDGE_CURVE ( 'NONE', #29585, #34227, #26471, .T. ) ;
#15114 = DIRECTION ( 'NONE',  ( 0.000000000000000000, -0.000000000000000000, 1.000000000000000000 ) ) ;
#15115 = ORIENTED_EDGE ( 'NONE', *, *, #21290, .F. ) ;
#15116 = CARTESIAN_POINT ( 'NONE',  ( -20.87835934725191933, 7.397986125119080825, -20.05141113204322423 ) ) ;
#15117 = LINE ( 'NONE', #12662, #1496 ) ;
#15118 = CARTESIAN_POINT ( 'NONE',  ( 8.410254037844358876, 17.06698729810774395, 10.00000000000000000 ) ) ;
#15119 = CARTESIAN_POINT ( 'NONE',  ( 25.18615822904968837, -26.10665374189652255, -6.311177740306681549 ) ) ;
#15120 = CARTESIAN_POINT ( 'NONE',  ( 12.41267482483262796, 26.20820393249957192, 6.000000000000000000 ) ) ;
#15121 = CARTESIAN_POINT ( 'NONE',  ( 12.80245792270091343, 21.86072822920704439, -17.40930403903157853 ) ) ;
#15122 = CARTESIAN_POINT ( 'NONE',  ( -5.055868909835983693, -26.71495157282352650, 12.14047268033097460 ) ) ;
#15123 = ORIENTED_EDGE ( 'NONE', *, *, #24599, .T. ) ;
#15124 = CARTESIAN_POINT ( 'NONE',  ( -13.52125812691403084, 19.79767817946104813, -18.59499618884840189 ) ) ;
#15125 = CARTESIAN_POINT ( 'NONE',  ( -26.52907865026647016, -8.732139513722060542, 20.82122704794093693 ) ) ;
#15126 = AXIS2_PLACEMENT_3D ( 'NONE', #15927, #489, #28309 ) ;
#15127 = CARTESIAN_POINT ( 'NONE',  ( 13.94482798346721353, 26.50521816028912525, 7.000000000000000000 ) ) ;
#15128 = CARTESIAN_POINT ( 'NONE',  ( 13.22685551685943750, 22.20468417799810368, -16.44677199118808630 ) ) ;
#15129 = B_SPLINE_CURVE_WITH_KNOTS ( 'NONE', 3,
 ( #29789, #1969, #13940, #32647 ),
 .UNSPECIFIED., .F., .F.,
 ( 4, 4 ),
 ( 0.000000000000000000, 1.000000000000000000 ),
 .UNSPECIFIED. ) ;
#15130 = VERTEX_POINT ( 'NONE', #36325 ) ;
#15131 = DIRECTION ( 'NONE',  ( -1.000000000000000000, 0.000000000000000000, 0.000000000000000000 ) ) ;
#15132 = ORIENTED_EDGE ( 'NONE', *, *, #2563, .T. ) ;
#15134 = DIRECTION ( 'NONE',  ( 1.000000000000000000, 0.000000000000000000, 0.000000000000000000 ) ) ;
#15133 = CARTESIAN_POINT ( 'NONE',  ( -14.22044113856730085, 24.65775004622394562, -12.53473158459295433 ) ) ;
#15135 = CARTESIAN_POINT ( 'NONE',  ( -13.90384679662962064, -24.14306550353441239, -13.49653236846003601 ) ) ;
#15136 = CARTESIAN_POINT ( 'NONE',  ( 7.713869163865849643, 10.18146832927074996, 10.49999999999999822 ) ) ;
#15137 = AXIS2_PLACEMENT_3D ( 'NONE', #13508, #25897, #38296 ) ;
#15138 = CARTESIAN_POINT ( 'NONE',  ( -18.43138823906292245, -10.38250042718520838, -26.25437023946332360 ) ) ;
#15139 = CARTESIAN_POINT ( 'NONE',  ( -11.13925371099489858, -22.06373630501061811, -17.53492604603244231 ) ) ;
#15140 = CARTESIAN_POINT ( 'NONE',  ( -12.03571151536224271, 31.45218678977246896, 7.000000000000000000 ) ) ;
#15141 = CARTESIAN_POINT ( 'NONE',  ( 13.15222192828749748, 18.70752044091742761, -20.71114827470474040 ) ) ;
#15142 = ORIENTED_EDGE ( 'NONE', *, *, #31621, .F. ) ;
#15143 = CARTESIAN_POINT ( 'NONE',  ( 24.64205719296993280, 7.386444343913908028, -5.960736307629980857 ) ) ;
#15144 = CARTESIAN_POINT ( 'NONE',  ( -0.9819677022348329842, 30.37627742347970283, 12.00000000000000000 ) ) ;
#15145 = DIRECTION ( 'NONE',  ( -0.000000000000000000, -0.000000000000000000, -1.000000000000000000 ) ) ;
#15146 = CARTESIAN_POINT ( 'NONE',  ( -8.183247089818959097, 16.78440424842446532, 13.00000000000000178 ) ) ;
#15147 = ORIENTED_EDGE ( 'NONE', *, *, #7350, .F. ) ;
#15148 = CARTESIAN_POINT ( 'NONE',  ( -31.78846064705475527, -1.224209755121473675, -6.856355146768160047 ) ) ;
#15149 = VECTOR ( 'NONE', #13917, 1000.000000000000000 ) ;
#15150 = CARTESIAN_POINT ( 'NONE',  ( 22.77334587319110071, 0.4700357585246903724, -21.59816853818721327 ) ) ;
#15151 = DIRECTION ( 'NONE',  ( -0.4067366430758009299, -0.9135454576426005335, -0.000000000000000000 ) ) ;
#15152 = VECTOR ( 'NONE', #2769, 1000.000000000000000 ) ;
#15153 = CARTESIAN_POINT ( 'NONE',  ( 20.08365402398579391, -19.49265790308171731, 20.69868183039781684 ) ) ;
#15154 = DIRECTION ( 'NONE',  ( 0.000000000000000000, 0.000000000000000000, -1.000000000000000000 ) ) ;
#15155 = CARTESIAN_POINT ( 'NONE',  ( -13.94482798346716201, 26.50521816028930644, 7.000000000000000000 ) ) ;
#15156 = PRESENTATION_LAYER_ASSIGNMENT (  '', '', ( #5414 ) ) ;
#15157 = ORIENTED_EDGE ( 'NONE', *, *, #8197, .T. ) ;
#15158 = CARTESIAN_POINT ( 'NONE',  ( -13.63581098909220479, 27.45627467658446008, 9.500000000000000000 ) ) ;
#15159 = B_SPLINE_CURVE_WITH_KNOTS ( 'NONE', 3,
 ( #2439, #11778, #30474, #28009, #30271, #14829, #17888, #24759 ),
 .UNSPECIFIED., .F., .F.,
 ( 4, 2, 2, 4 ),
 ( 0.000000000000000000, 0.0004726692273637240907, 0.0007090038410455856482, 0.0009453384547274473141 ),
 .UNSPECIFIED. ) ;
#15160 = AXIS2_PLACEMENT_3D ( 'NONE', #24744, #37142, #22097 ) ;
#15161 = DIRECTION ( 'NONE',  ( -0.2079116908177533474, 0.9781476007338067991, 0.000000000000000000 ) ) ;
#15162 = DIRECTION ( 'NONE',  ( 0.8090169943749504489, 0.5877852522924690293, -0.000000000000000000 ) ) ;
#15163 = CARTESIAN_POINT ( 'NONE',  ( 3.179194328277191506, 30.99994159145660078, -14.75100848146118970 ) ) ;
#15164 = DIRECTION ( 'NONE',  ( 0.8064441531181091305, 0.1277282058446026769, 0.5773502691896269523 ) ) ;
#15165 = CARTESIAN_POINT ( 'NONE',  ( -13.19371393710743412, 15.45995597598988880, 10.76099332938164288 ) ) ;
#15166 = CARTESIAN_POINT ( 'NONE',  ( -4.082607396026893376, 23.58034083595207875, 12.00000000000000000 ) ) ;
#15167 = CYLINDRICAL_SURFACE ( 'NONE', #19278, 1.000000000000000000 ) ;
#15168 = CARTESIAN_POINT ( 'NONE',  ( -11.77091082532341204, 29.60251629318183575, 6.000000000000000000 ) ) ;
#15169 = CARTESIAN_POINT ( 'NONE',  ( 14.42035624161478857, 26.65972665747660031, 10.49999999999999822 ) ) ;
#15170 = CARTESIAN_POINT ( 'NONE',  ( 10.81914528518449892, 18.98893231873664078, -23.75032747527389887 ) ) ;
#15171 = CARTESIAN_POINT ( 'NONE',  ( 10.72918489117954088, 32.98258515686300996, 7.000000000000000000 ) ) ;
#15172 = ORIENTED_EDGE ( 'NONE', *, *, #1692, .F. ) ;
#15174 = DIRECTION ( 'NONE',  ( 0.000000000000000000, 0.000000000000000000, 1.000000000000000000 ) ) ;
#15173 = CARTESIAN_POINT ( 'NONE',  ( -17.26255069659608310, 13.24883950376971598, -21.14449336137800373 ) ) ;
#15175 = AXIS2_PLACEMENT_3D ( 'NONE', #8010, #17380, #9420 ) ;
#15176 = DIRECTION ( 'NONE',  ( 1.000000000000000000, 0.000000000000000000, 0.000000000000000000 ) ) ;
#15177 = CARTESIAN_POINT ( 'NONE',  ( 14.73715625254732231, -25.65210853834342686, -10.18073480337578829 ) ) ;
#15178 = CARTESIAN_POINT ( 'NONE',  ( -21.42170977900226703, -25.44073649801487491, -10.34015057612328370 ) ) ;
#15179 = DIRECTION ( 'NONE',  ( 1.000000000000000000, 0.000000000000000000, 0.000000000000000000 ) ) ;
#15180 = CARTESIAN_POINT ( 'NONE',  ( 11.66727136869983283, 18.92964083422280552, -22.73188705715889313 ) ) ;
#15181 = ORIENTED_EDGE ( 'NONE', *, *, #14748, .F. ) ;
#15182 = CARTESIAN_POINT ( 'NONE',  ( 6.935770203493858865, 22.34671014717335780, 6.000000000000000000 ) ) ;
#15183 = CARTESIAN_POINT ( 'NONE',  ( 39.05366788551321378, -6.582903510435600403, 11.00000000000000000 ) ) ;
#15184 = CARTESIAN_POINT ( 'NONE',  ( -29.43343111547412150, -25.34807889869424358, 14.53008259254020551 ) ) ;
#15185 = VECTOR ( 'NONE', #234, 1000.000000000000000 ) ;
#15186 = CARTESIAN_POINT ( 'NONE',  ( -27.78070527026259740, -23.17491891568929674, -9.313639814683513762 ) ) ;
#15187 = CARTESIAN_POINT ( 'NONE',  ( 1.264170519848298424, -20.71387444820763335, -26.62396510143870287 ) ) ;
#15188 = CARTESIAN_POINT ( 'NONE',  ( 15.62693799746092971, 26.04132429419060557, -4.999999999999999112 ) ) ;
#15189 = CARTESIAN_POINT ( 'NONE',  ( 20.92218733704004663, 11.65753682693518911, -11.88398976070928015 ) ) ;
#15190 = PRODUCT_DEFINITION_FORMATION_WITH_SPECIFIED_SOURCE ( 'ANY', '', #7087, .NOT_KNOWN. ) ;
#15191 = CARTESIAN_POINT ( 'NONE',  ( 9.697889840765411051, 31.90483559858327212, 9.500000000000000000 ) ) ;
#15192 = CARTESIAN_POINT ( 'NONE',  ( -5.321426344574297751, 37.58193452263969903, -5.861036830693866051 ) ) ;
#15193 = VERTEX_POINT ( 'NONE', #33492 ) ;
#15194 = CARTESIAN_POINT ( 'NONE',  ( -31.89401778038308777, -5.009461060679962330, -11.27517601632434996 ) ) ;
#15195 = AXIS2_PLACEMENT_3D ( 'NONE', #18217, #8866, #27550 ) ;
#15196 = CARTESIAN_POINT ( 'NONE',  ( -18.63686013482982773, 22.43247111565169405, 12.14047268035308136 ) ) ;
#15197 = ORIENTED_EDGE ( 'NONE', *, *, #10260, .T. ) ;
#15198 = DIRECTION ( 'NONE',  ( 0.000000000000000000, 0.000000000000000000, 1.000000000000000000 ) ) ;
#15199 = ADVANCED_FACE ( 'NONE', ( #8489 ), #5441, .T. ) ;
#15200 = CARTESIAN_POINT ( 'NONE',  ( -3.370709253380788084E-06, 22.50000000000031264, 6.000000000000000000 ) ) ;
#15201 = CARTESIAN_POINT ( 'NONE',  ( -29.03964460488705868, 0.9025844493971224569, -9.726429368847238521 ) ) ;
#15202 = CARTESIAN_POINT ( 'NONE',  ( 35.25372542428971201, -14.20602460021386193, -4.999999999999997335 ) ) ;
#15203 = CIRCLE ( 'NONE', #269, 1.000000000000000000 ) ;
#15204 = EDGE_CURVE ( 'NONE', #22179, #34387, #24125, .T. ) ;
#15205 = EDGE_LOOP ( 'NONE', ( #20300, #8195, #21684, #26751 ) ) ;
#15206 = DIRECTION ( 'NONE',  ( 1.000000000000000000, 0.000000000000000000, 0.000000000000000000 ) ) ;
#15207 = ORIENTED_EDGE ( 'NONE', *, *, #25365, .F. ) ;
#15208 = ADVANCED_FACE ( 'NONE', ( #27178 ), #30882, .T. ) ;
#15209 = DIRECTION ( 'NONE',  ( 0.7032331762534027586, -0.07391278520357077997, -0.7071067811865484609 ) ) ;
#15210 = CYLINDRICAL_SURFACE ( 'NONE', #28569, 0.5000000000000004441 ) ;
#15211 = B_SPLINE_CURVE_WITH_KNOTS ( 'NONE', 3,
 ( #11863, #24253, #36257, #18168, #33809, #5957, #18361, #27692, #23655, #17575 ),
 .UNSPECIFIED., .F., .F.,
 ( 4, 2, 2, 2, 4 ),
 ( 0.7014259083631586567, 0.7760694312723689370, 0.8507129541815793283, 0.9253564770907896087, 1.000000000000000000 ),
 .UNSPECIFIED. ) ;
#15212 = CIRCLE ( 'NONE', #37913, 1.000000000000000000 ) ;
#15213 = CARTESIAN_POINT ( 'NONE',  ( -11.44473057578096764, 31.45924896672619298, 7.000000000000000000 ) ) ;
#15214 = ORIENTED_EDGE ( 'NONE', *, *, #28400, .F. ) ;
#15215 = CARTESIAN_POINT ( 'NONE',  ( -2.236895112781585482, 20.38702974553298830, -29.99999999999999289 ) ) ;
#15216 = LINE ( 'NONE', #15012, #19130 ) ;
#15217 = FACE_OUTER_BOUND ( 'NONE', #38282, .T. ) ;
#15218 = FACE_OUTER_BOUND ( 'NONE', #30850, .T. ) ;
#15219 = CARTESIAN_POINT ( 'NONE',  ( 16.34286479496965327, -12.53075802742931266, -28.46040907605739534 ) ) ;
#15220 = CARTESIAN_POINT ( 'NONE',  ( 16.27893284296826337, 12.57309314609360129, -28.28617463803444210 ) ) ;
#15221 = CARTESIAN_POINT ( 'NONE',  ( 10.45177150771196040, 27.06930753712435589, -15.02913264056041243 ) ) ;
#15222 = CIRCLE ( 'NONE', #20416, 21.00000000000002842 ) ;
#15223 = VERTEX_POINT ( 'NONE', #8890 ) ;
#15224 = CARTESIAN_POINT ( 'NONE',  ( -21.61538879608044894, 11.66913484622351938, -8.407920237374057137 ) ) ;
#15225 = EDGE_CURVE ( 'NONE', #15233, #16758, #33690, .T. ) ;
#15226 = CARTESIAN_POINT ( 'NONE',  ( 14.80517497283435979, -25.49818430814198322, -10.64180685166133600 ) ) ;
#15227 = CARTESIAN_POINT ( 'NONE',  ( 11.11016527260166775, 31.83082137946472656, 11.00000000000000000 ) ) ;
#15228 = CARTESIAN_POINT ( 'NONE',  ( 21.88444403592371756, 6.126538576424477966, -30.00000000000001066 ) ) ;
#15229 = CARTESIAN_POINT ( 'NONE',  ( -12.37885040140798765, 20.50679986589284098, -19.49376219608895866 ) ) ;
#15230 = CARTESIAN_POINT ( 'NONE',  ( -17.04124340972882834, -20.30949825123198949, -17.92891331059860249 ) ) ;
#15231 = CARTESIAN_POINT ( 'NONE',  ( 10.05098765505323222, -24.42915519467451091, -11.72241341964282491 ) ) ;
#15232 = CARTESIAN_POINT ( 'NONE',  ( 2.140527761532493134, 7.619874298175136396, 11.00000000000000000 ) ) ;
#15233 = VERTEX_POINT ( 'NONE', #34666 ) ;
#15234 = VERTEX_POINT ( 'NONE', #30827 ) ;
#15235 = CARTESIAN_POINT ( 'NONE',  ( -6.485893174894165725, 19.45725460019876252, -29.26213642569760864 ) ) ;
#15236 = CARTESIAN_POINT ( 'NONE',  ( 0.5934445985557578185, 37.50000000000000711, 10.49999999999999822 ) ) ;
#15237 = DIRECTION ( 'NONE',  ( 0.000000000000000000, 0.000000000000000000, -1.000000000000000000 ) ) ;
#15238 = CIRCLE ( 'NONE', #10068, 0.9999999999999986677 ) ;
#15239 = CARTESIAN_POINT ( 'NONE',  ( 13.48130249190479191, 27.93180293473185927, 7.000000000000000000 ) ) ;
#15240 = VERTEX_POINT ( 'NONE', #40160 ) ;
#15241 = CARTESIAN_POINT ( 'NONE',  ( 20.96888093453203794, 0.8149526723977724707, -26.22550878230689619 ) ) ;
#15242 = PLANE ( 'NONE',  #7656 ) ;
#15243 = LINE ( 'NONE', #34140, #10910 ) ;
#15244 = VERTEX_POINT ( 'NONE', #3384 ) ;
#15245 = CIRCLE ( 'NONE', #37286, 0.5000000000000005551 ) ;
#15246 = CARTESIAN_POINT ( 'NONE',  ( -25.83226977945856362, 0.3709960288796101402, -16.44840538093085414 ) ) ;
#15247 = EDGE_CURVE ( 'NONE', #6531, #5452, #33485, .T. ) ;
#15248 = DIRECTION ( 'NONE',  ( -0.6691306063588560171, 0.7431448254773962425, 0.000000000000000000 ) ) ;
#15249 = ORIENTED_EDGE ( 'NONE', *, *, #8377, .F. ) ;
#15250 = CARTESIAN_POINT ( 'NONE',  ( 30.76698505935834405, -6.362076114912868618, -13.06728835035745462 ) ) ;
#15251 = VECTOR ( 'NONE', #174, 1000.000000000000000 ) ;
#15252 = ORIENTED_EDGE ( 'NONE', *, *, #11067, .F. ) ;
#15253 = CARTESIAN_POINT ( 'NONE',  ( -12.30427675147431010, 35.50736440028104823, 12.73282698324895534 ) ) ;
#15254 = ADVANCED_FACE ( 'NONE', ( #142 ), #28362, .F. ) ;
#15255 = CARTESIAN_POINT ( 'NONE',  ( 17.21213525677581657, -20.06193531423786780, 20.50957957746029336 ) ) ;
#15256 = DIRECTION ( 'NONE',  ( 0.8090169943749505599, 0.5877852522924689183, 0.000000000000000000 ) ) ;
#15257 = CARTESIAN_POINT ( 'NONE',  ( -5.506351411279842623, 29.74560631396580490, 20.50957957746029336 ) ) ;
#15258 = DIRECTION ( 'NONE',  ( 0.6691306063588671194, 0.7431448254773862505, 0.000000000000000000 ) ) ;
#15259 = ORIENTED_EDGE ( 'NONE', *, *, #28970, .F. ) ;
#15260 = CARTESIAN_POINT ( 'NONE',  ( 3.607749162633208329, 7.931741834401763391, 10.49999999999999822 ) ) ;
#15261 = CARTESIAN_POINT ( 'NONE',  ( -11.11100267139600639, 25.58833710557283680, 19.66345542862528717 ) ) ;
#15262 = FACE_OUTER_BOUND ( 'NONE', #26843, .T. ) ;
#15263 = DIRECTION ( 'NONE',  ( -0.9135454576426006446, 0.4067366430758009299, 0.000000000000000000 ) ) ;
#15264 = VECTOR ( 'NONE', #37562, 1000.000000000000114 ) ;
#15265 = CARTESIAN_POINT ( 'NONE',  ( 8.135523341600167768, 36.16613191329250299, -6.297504617459584786 ) ) ;
#15266 = CARTESIAN_POINT ( 'NONE',  ( 2.871201846650637268, 31.30332840660451765, 13.00000000000000178 ) ) ;
#15267 = EDGE_CURVE ( 'NONE', #25818, #26036, #12926, .T. ) ;
#15268 = ADVANCED_FACE ( 'NONE', ( #25119 ), #32841, .T. ) ;
#15269 = CARTESIAN_POINT ( 'NONE',  ( 11.21453531681511784, -17.17359087135386631, -29.99999999999999645 ) ) ;
#15270 = CIRCLE ( 'NONE', #8776, 1.000000000000002665 ) ;
#15271 = DIRECTION ( 'NONE',  ( -0.000000000000000000, -0.000000000000000000, -1.000000000000000000 ) ) ;
#15272 = CARTESIAN_POINT ( 'NONE',  ( 10.44103466624280507, 32.57396620494213124, 11.00000000000000000 ) ) ;
#15273 = ORIENTED_EDGE ( 'NONE', *, *, #9017, .T. ) ;
#15274 = AXIS2_PLACEMENT_3D ( 'NONE', #27503, #8822, #17579 ) ;
#15275 = CARTESIAN_POINT ( 'NONE',  ( -13.89045959741800296, 23.13722222314543941, -14.49167495132802763 ) ) ;
#15276 = CIRCLE ( 'NONE', #1654, 1.000000000000000000 ) ;
#15277 = CARTESIAN_POINT ( 'NONE',  ( -27.60461630348678241, -20.46464247653241841, 19.27171037444157164 ) ) ;
#15278 = CARTESIAN_POINT ( 'NONE',  ( 11.44353187076013434, -20.98966551814972803, -19.50774576217023792 ) ) ;
#15279 = CARTESIAN_POINT ( 'NONE',  ( -3.503793317224517700, 8.420815634768723967, 10.99999999999999289 ) ) ;
#15280 = EDGE_LOOP ( 'NONE', ( #940, #30045, #28393, #36338 ) ) ;
#15281 = ORIENTED_EDGE ( 'NONE', *, *, #2222, .F. ) ;
#15282 = CARTESIAN_POINT ( 'NONE',  ( -9.499396656360119096, 18.35689620915350417, -27.98656568115667653 ) ) ;
#15283 = CARTESIAN_POINT ( 'NONE',  ( -11.59581746604265184, -16.91849113041673647, -30.00000000000000355 ) ) ;
#15284 = DIRECTION ( 'NONE',  ( 1.000000000000000000, 1.387778780781439522E-14, 0.000000000000000000 ) ) ;
#15285 = ORIENTED_EDGE ( 'NONE', *, *, #18685, .F. ) ;
#15286 = CARTESIAN_POINT ( 'NONE',  ( -21.60667917395808502, -6.743361281366732740, -23.13545725626142513 ) ) ;
#15287 = CARTESIAN_POINT ( 'NONE',  ( -13.54564564923477477, -24.09781583726222465, -13.52072601590651679 ) ) ;
#15288 = CARTESIAN_POINT ( 'NONE',  ( 35.27625572565175815, 1.213838575767484107, 23.00000000000469669 ) ) ;
#15289 = EDGE_LOOP ( 'NONE', ( #21393, #8512, #12047, #8577 ) ) ;
#15290 = CARTESIAN_POINT ( 'NONE',  ( 25.09144846651838634, 0.6029723664216483092, -17.46064374251114160 ) ) ;
#15291 = CARTESIAN_POINT ( 'NONE',  ( 18.23649648353767461, -16.09146789626181118, 20.99999999999999645 ) ) ;
#15292 = CARTESIAN_POINT ( 'NONE',  ( -6.440836655099179353, 34.39106106163288246, 13.00000000000000178 ) ) ;
#15293 = EDGE_LOOP ( 'NONE', ( #18350, #19141, #18742, #30036 ) ) ;
#15294 = CARTESIAN_POINT ( 'NONE',  ( -28.95213599401768434, 0.02960606682219414990, -11.59245046285586156 ) ) ;
#15295 = EDGE_CURVE ( 'NONE', #28327, #8296, #22364, .T. ) ;
#15296 = ORIENTED_EDGE ( 'NONE', *, *, #31497, .F. ) ;
#15297 = CARTESIAN_POINT ( 'NONE',  ( 20.50115022911059270, -0.2752137519716084113, -30.00000000000000000 ) ) ;
#15298 = CARTESIAN_POINT ( 'NONE',  ( 9.908215252718470367, -17.95959716121500449, -30.00000000000000711 ) ) ;
#15299 = CARTESIAN_POINT ( 'NONE',  ( 33.56035593554180707, -14.08372035823031077, 17.92354375535250810 ) ) ;
#15300 = ORIENTED_EDGE ( 'NONE', *, *, #2466, .F. ) ;
#15301 = CARTESIAN_POINT ( 'NONE',  ( -21.05269208634015854, 3.574702288414596474, -24.13667089053400971 ) ) ;
#15302 = CIRCLE ( 'NONE', #17900, 1.000000000000000000 ) ;
#15303 = CARTESIAN_POINT ( 'NONE',  ( -10.47589056713771249, 33.23591321793828257, 7.338691926023217071 ) ) ;
#15304 = CARTESIAN_POINT ( 'NONE',  ( 75.15099915297797395, 43.38844959084117647, 23.00000000000000000 ) ) ;
#15305 = CIRCLE ( 'NONE', #19860, 1.000000000000000000 ) ;
#15306 = CYLINDRICAL_SURFACE ( 'NONE', #18733, 1.000000000000000000 ) ;
#15307 = AXIS2_PLACEMENT_3D ( 'NONE', #31067, #21122, #33729 ) ;
#15308 = CARTESIAN_POINT ( 'NONE',  ( 12.49038105676653743, 14.13397459621550745, 10.49999999999999822 ) ) ;
#15309 = FACE_BOUND ( 'NONE', #38879, .T. ) ;
#15310 = CARTESIAN_POINT ( 'NONE',  ( 28.63966609528962337, 4.835996017632539612, 12.73282698324585560 ) ) ;
#15311 = ORIENTED_EDGE ( 'NONE', *, *, #35900, .T. ) ;
#15312 = CARTESIAN_POINT ( 'NONE',  ( -24.20609638677606412, 8.035638068618503382, -5.000000000000000888 ) ) ;
#15313 = LINE ( 'NONE', #13412, #8630 ) ;
#15314 = FACE_OUTER_BOUND ( 'NONE', #22562, .T. ) ;
#15315 = CARTESIAN_POINT ( 'NONE',  ( 16.13585048104015840, -17.81699276545519339, -20.99261974159198729 ) ) ;
#15316 = CARTESIAN_POINT ( 'NONE',  ( 14.01837422881150452, 21.26636931122159169, 12.00000000000000000 ) ) ;
#15317 = EDGE_CURVE ( 'NONE', #12819, #31457, #18560, .T. ) ;
#15318 = CARTESIAN_POINT ( 'NONE',  ( 15.26288695882580093, 26.87683090409402098, -6.882367006327409165 ) ) ;
#15319 = ORIENTED_EDGE ( 'NONE', *, *, #1055, .T. ) ;
#15320 = CARTESIAN_POINT ( 'NONE',  ( -12.94450195943344717, 16.22636800668987078, -26.98281085777279742 ) ) ;
#15321 = CARTESIAN_POINT ( 'NONE',  ( -27.68412949013605839, -10.20944236610018940, 20.69868183039781329 ) ) ;
#15322 = DIRECTION ( 'NONE',  ( 0.6724985119639617093, -0.2185080122244195122, -0.7071067811865406894 ) ) ;
#15323 = CARTESIAN_POINT ( 'NONE',  ( 13.78307072732043537, 23.36720680302070363, -14.47774454319189452 ) ) ;
#15324 = ORIENTED_EDGE ( 'NONE', *, *, #35287, .F. ) ;
#15325 = FACE_OUTER_BOUND ( 'NONE', #21581, .T. ) ;
#15326 = EDGE_LOOP ( 'NONE', ( #38541, #32086, #6617, #39135 ) ) ;
#15327 = AXIS2_PLACEMENT_3D ( 'NONE', #16033, #24975, #3636 ) ;
#15329 = LINE ( 'NONE', #9236, #36745 ) ;
#15328 = CARTESIAN_POINT ( 'NONE',  ( -15.31676148297655615, 27.12555199532522110, -5.000000000000000888 ) ) ;
#15330 = CARTESIAN_POINT ( 'NONE',  ( -14.55700941178259633, -25.10763777908611871, -11.58478221798611507 ) ) ;
#15331 = CARTESIAN_POINT ( 'NONE',  ( -30.33933116650765527, 6.243556997736136260, 10.99999999999999822 ) ) ;
#15332 = CONICAL_SURFACE ( 'NONE', #36105, 1.000000000000002665, 0.7853981633974509435 ) ;
#15333 = CARTESIAN_POINT ( 'NONE',  ( -33.06715563149963089, -18.61836429930299985, -7.543782265277601873 ) ) ;
#15334 = CARTESIAN_POINT ( 'NONE',  ( -11.36118072446144645, -25.45899015601136028, -8.329040007300676507 ) ) ;
#15335 = CARTESIAN_POINT ( 'NONE',  ( 8.927394655428276593, 11.06314620770945290, 7.000000000000000000 ) ) ;
#15336 = CARTESIAN_POINT ( 'NONE',  ( 16.22988331200706469, 23.74208035757151691, -6.896498610208569247 ) ) ;
#15337 = EDGE_LOOP ( 'NONE', ( #4719, #25193, #39002 ) ) ;
#15338 = CARTESIAN_POINT ( 'NONE',  ( 25.99279172464974508, 5.576676355531687612, -5.956011220400047712 ) ) ;
#15339 = VECTOR ( 'NONE', #3140, 1000.000000000000227 ) ;
#15340 = DIRECTION ( 'NONE',  ( 1.000000000000000000, 0.000000000000000000, 0.000000000000000000 ) ) ;
#15341 = CARTESIAN_POINT ( 'NONE',  ( 0.000000000000000000, 22.50000000000000355, 12.00000000000000000 ) ) ;
#15342 = DIRECTION ( 'NONE',  ( -0.8660254037844432595, -0.4999999999999920064, 0.000000000000000000 ) ) ;
#15343 = ORIENTED_EDGE ( 'NONE', *, *, #3206, .T. ) ;
#15344 = CARTESIAN_POINT ( 'NONE',  ( -31.52181932710565349, -0.8163613484490098715, -6.400955463894867137 ) ) ;
#15345 = EDGE_CURVE ( 'NONE', #9569, #12475, #1039, .T. ) ;
#15346 = CARTESIAN_POINT ( 'NONE',  ( 30.49808096523472756, -0.1579847061273154385, -8.289727916065702473 ) ) ;
#15347 = CARTESIAN_POINT ( 'NONE',  ( -4.678013043399448456, 44.50832101651065642, 11.00000000000000000 ) ) ;
#15348 = EDGE_CURVE ( 'NONE', #5069, #16796, #6226, .T. ) ;
#15349 = CARTESIAN_POINT ( 'NONE',  ( 26.24102572422061996, -17.42682220599409604, 20.50957957746051719 ) ) ;
#15350 = VERTEX_POINT ( 'NONE', #3584 ) ;
#15351 = CARTESIAN_POINT ( 'NONE',  ( 22.40982762235196901, 2.618079236896951656, -21.24786896499729139 ) ) ;
#15352 = CARTESIAN_POINT ( 'NONE',  ( -8.559512017365658920, 19.71884705062586107, 6.000000000000000000 ) ) ;
#15353 = EDGE_CURVE ( 'NONE', #11532, #19973, #15981, .T. ) ;
#15354 = ORIENTED_EDGE ( 'NONE', *, *, #12997, .T. ) ;
#15355 = DIRECTION ( 'NONE',  ( 1.000000000000000000, 0.000000000000000000, 0.000000000000000000 ) ) ;
#15356 = AXIS2_PLACEMENT_3D ( 'NONE', #305, #3544, #6582 ) ;
#15357 = AXIS2_PLACEMENT_3D ( 'NONE', #26876, #39466, #39265 ) ;
#15358 = CARTESIAN_POINT ( 'NONE',  ( -23.05386822411323422, -7.747535282638357224, 23.00000000000000000 ) ) ;
#15359 = FACE_OUTER_BOUND ( 'NONE', #19257, .T. ) ;
#15360 = CARTESIAN_POINT ( 'NONE',  ( 2.942419129403968547, 28.79255951157002613, -16.65093014769575674 ) ) ;
#15361 = CARTESIAN_POINT ( 'NONE',  ( 2.317734025672766318, 9.191051544684729180, 9.500000000000000000 ) ) ;
#15362 = DIRECTION ( 'NONE',  ( 1.000000000000000000, 0.000000000000000000, 0.000000000000000000 ) ) ;
#15363 = CARTESIAN_POINT ( 'NONE',  ( 10.16520467992603294, 20.33931832809677331, 12.00000000000000000 ) ) ;
#15364 = EDGE_CURVE ( 'NONE', #12341, #17253, #25680, .T. ) ;
#15365 = DIRECTION ( 'NONE',  ( -1.000000000000000000, 0.000000000000000000, 0.000000000000000000 ) ) ;
#15366 = DIRECTION ( 'NONE',  ( 1.000000000000000000, 0.000000000000000000, 0.000000000000000000 ) ) ;
#15367 = LINE ( 'NONE', #27559, #22275 ) ;
#15368 = ADVANCED_FACE ( 'NONE', ( #27770 ), #30633, .F. ) ;
#15369 = CARTESIAN_POINT ( 'NONE',  ( 10.36933582218109429, 17.95643907423222885, -27.39330729671292630 ) ) ;
#15370 = DIRECTION ( 'NONE',  ( -0.000000000000000000, -0.000000000000000000, -1.000000000000000000 ) ) ;
#15371 = ORIENTED_EDGE ( 'NONE', *, *, #22285, .T. ) ;
#15373 = CARTESIAN_POINT ( 'NONE',  ( 9.625795778761983001, 10.95253033666821274, 11.00000000000000000 ) ) ;
#15372 = CARTESIAN_POINT ( 'NONE',  ( -16.69924863411024418, 15.13135123064752996, -18.96634367901145524 ) ) ;
#15374 = LINE ( 'NONE', #34067, #19866 ) ;
#15375 = CARTESIAN_POINT ( 'NONE',  ( 10.83685788847059506, -19.99059525684932481, -21.61737879950500840 ) ) ;
#15376 = CARTESIAN_POINT ( 'NONE',  ( -16.85113020441335507, -21.30447706854098300, -16.99219159709304705 ) ) ;
#15377 = CARTESIAN_POINT ( 'NONE',  ( -19.48557158514998022, -11.24999999999982414, 0.000000000000000000 ) ) ;
#15378 = B_SPLINE_CURVE_WITH_KNOTS ( 'NONE', 3,
 ( #20266, #23104, #1373, #20068, #25943, #17225, #29402, #38343 ),
 .UNSPECIFIED., .F., .F.,
 ( 4, 2, 2, 4 ),
 ( 0.000000000000000000, 0.0002364868538934304361, 0.0004729737077868608722, 0.0009459474155737300927 ),
 .UNSPECIFIED. ) ;
#15379 = CARTESIAN_POINT ( 'NONE',  ( 13.48181092597923936, 22.83514489210295650, -15.44851730194768535 ) ) ;
#15380 = ORIENTED_EDGE ( 'NONE', *, *, #31044, .F. ) ;
#15381 = CARTESIAN_POINT ( 'NONE',  ( 14.42035624161478857, 26.65972665747660031, 11.00000000000000000 ) ) ;
#15382 = SHAPE_REPRESENTATION ( 'BR-834', ( #22921, #24864, #22279, #37847, #20362, #1526, #2834, #25528, #7343 ), #228 ) ;
#15383 = CARTESIAN_POINT ( 'NONE',  ( -15.43577743098633981, -26.72909887300547283, -5.474191126876100988 ) ) ;
#15384 = CARTESIAN_POINT ( 'NONE',  ( -32.21892379115398342, -22.89377427927484021, 14.53008259254002610 ) ) ;
#15385 = CARTESIAN_POINT ( 'NONE',  ( -28.90526601420243935, -24.05987742975590749, -6.288601596644300962 ) ) ;
#15386 = CARTESIAN_POINT ( 'NONE',  ( -2.597410653098545463, -24.79173595445318767, -5.000000000000000000 ) ) ;
#15387 = CARTESIAN_POINT ( 'NONE',  ( 11.26908400546618871, 17.12495040990986794, -29.35441016993270580 ) ) ;
#15388 = CARTESIAN_POINT ( 'NONE',  ( 21.64434010710703404, 12.04703973602239842, -4.999999999999996447 ) ) ;
#15389 = FACE_OUTER_BOUND ( 'NONE', #34482, .T. ) ;
#15390 = CARTESIAN_POINT ( 'NONE',  ( -4.537929203215356644, 31.78147521891694893, -13.83853917308986148 ) ) ;
#15391 = VERTEX_POINT ( 'NONE', #34273 ) ;
#15392 = CARTESIAN_POINT ( 'NONE',  ( -31.16281537880387731, -4.882152567110715324, -12.19897026441750931 ) ) ;
#15393 = EDGE_CURVE ( 'NONE', #27469, #38623, #22081, .T. ) ;
#15394 = VECTOR ( 'NONE', #3694, 1000.000000000000000 ) ;
#15395 = CARTESIAN_POINT ( 'NONE',  ( -18.17912400190525801, 22.26280294339773036, 13.92931973829419690 ) ) ;
#15396 = ORIENTED_EDGE ( 'NONE', *, *, #17261, .F. ) ;
#15397 = ADVANCED_FACE ( 'NONE', ( #36924 ), #18437, .F. ) ;
#15398 = CARTESIAN_POINT ( 'NONE',  ( 21.61735397326475905, 13.43626163844561994, 10.00000000000000000 ) ) ;
#15399 = CARTESIAN_POINT ( 'NONE',  ( 12.39463915635820612, 18.33192650902018883, 12.00000000000000000 ) ) ;
#15400 = AXIS2_PLACEMENT_3D ( 'NONE', #11753, #39378, #2019 ) ;
#15401 = CARTESIAN_POINT ( 'NONE',  ( -27.28629896358888374, 0.7998108622630019093, -13.54774279276146665 ) ) ;
#15402 = CARTESIAN_POINT ( 'NONE',  ( 23.93184905822953468, -8.822957309754631439, -19.71412903833790509 ) ) ;
#15403 = CIRCLE ( 'NONE', #3706, 0.9999999999999985567 ) ;
#15404 = ORIENTED_EDGE ( 'NONE', *, *, #29900, .F. ) ;
#15405 = CARTESIAN_POINT ( 'NONE',  ( -4.503793317224517700, 8.420815634768723967, 7.000000000000000000 ) ) ;
#15406 = VERTEX_POINT ( 'NONE', #21673 ) ;
#15407 = CARTESIAN_POINT ( 'NONE',  ( -10.72918489117943963, 32.98258515686311654, 7.000000000000000000 ) ) ;
#15408 = CARTESIAN_POINT ( 'NONE',  ( -19.48557158514998022, -11.24999999999982414, 23.00000000000000000 ) ) ;
#15409 = CARTESIAN_POINT ( 'NONE',  ( -5.187504188494229673, 36.60991850771488743, 11.00000000000000000 ) ) ;
#15410 = VERTEX_POINT ( 'NONE', #18636 ) ;
#15411 = CARTESIAN_POINT ( 'NONE',  ( -1.923949180127531244, 38.42603324025853340, -5.000000000000000000 ) ) ;
#15412 = CARTESIAN_POINT ( 'NONE',  ( -5.547064146435500831, 36.18820672788730519, 10.94611345180491035 ) ) ;
#15413 = FACE_OUTER_BOUND ( 'NONE', #27321, .T. ) ;
#15414 = CARTESIAN_POINT ( 'NONE',  ( -7.983541495324330661, 10.37739674670167389, 10.83333333333333215 ) ) ;
#15415 = CARTESIAN_POINT ( 'NONE',  ( 16.46668505474601929, -12.62653714806953609, -27.72794644683495591 ) ) ;
#15416 = CARTESIAN_POINT ( 'NONE',  ( 19.31863883839061558, 15.70629445910060440, -8.886768639220122168 ) ) ;
#15417 = AXIS2_PLACEMENT_3D ( 'NONE', #33751, #412, #27835 ) ;
#15418 = CARTESIAN_POINT ( 'NONE',  ( 13.68675864763349281, 30.66322818530211691, -6.360680230841967209 ) ) ;
#15419 = VECTOR ( 'NONE', #39525, 1000.000000000000114 ) ;
#15420 = EDGE_LOOP ( 'NONE', ( #14651, #4453, #35372 ) ) ;
#15421 = CARTESIAN_POINT ( 'NONE',  ( -21.10979132117194368, 12.63226555665139728, -7.918966435008256255 ) ) ;
#15422 = CARTESIAN_POINT ( 'NONE',  ( -2.594149110900646260, 26.80855565015090747, 23.00000000000000000 ) ) ;
#15423 = CARTESIAN_POINT ( 'NONE',  ( 15.44356999697831334, -26.44085754146421507, -7.821532254917190841 ) ) ;
#15424 = FACE_OUTER_BOUND ( 'NONE', #24773, .T. ) ;
#15425 = EDGE_CURVE ( 'NONE', #11093, #39968, #6234, .T. ) ;
#15426 = CIRCLE ( 'NONE', #31001, 16.00000000000000355 ) ;
#15427 = CARTESIAN_POINT ( 'NONE',  ( -5.636483973512888213, -22.01575377102104270, -21.50719306941231679 ) ) ;
#15428 = CARTESIAN_POINT ( 'NONE',  ( 10.39021566973302946, 20.90519018800545581, 11.00000000000000000 ) ) ;
#15429 = AXIS2_PLACEMENT_3D ( 'NONE', #33254, #20453, #2163 ) ;
#15430 = CARTESIAN_POINT ( 'NONE',  ( -10.98560485883561455, 17.36128174412877456, -28.70610319738578298 ) ) ;
#15431 = CARTESIAN_POINT ( 'NONE',  ( -23.21950482537012661, -25.96020083042891713, -8.516380179814060369 ) ) ;
#15432 = CARTESIAN_POINT ( 'NONE',  ( 9.916190783591865454, -21.18337445448872813, -19.66014789460458090 ) ) ;
#15433 = CARTESIAN_POINT ( 'NONE',  ( -14.36830325120616081, 20.48707633493503977, 11.00000000000000000 ) ) ;
#15434 = VERTEX_POINT ( 'NONE', #28168 ) ;
#15435 = CARTESIAN_POINT ( 'NONE',  ( -9.608178598149136107, 29.00351644723056665, -13.99953411183117069 ) ) ;
#15436 = CARTESIAN_POINT ( 'NONE',  ( 0.5000000000000000000, 37.47223625998415741, 10.68306085400100081 ) ) ;
#15437 = CARTESIAN_POINT ( 'NONE',  ( -12.80736835487441816, 15.68301270189233243, 11.00000000000000000 ) ) ;
#15438 = CARTESIAN_POINT ( 'NONE',  ( -13.53057405073934838, 22.08338764125509002, 9.500000000000000000 ) ) ;
#15439 = EDGE_LOOP ( 'NONE', ( #29701, #13504 ) ) ;
#15440 = CARTESIAN_POINT ( 'NONE',  ( 20.69356520073354133, 0.8462078722227619476, -27.44831186004264367 ) ) ;
#15441 = DIRECTION ( 'NONE',  ( 1.000000000000000000, 0.000000000000000000, 0.000000000000000000 ) ) ;
#15442 = DIRECTION ( 'NONE',  ( 0.9945218953682730678, -0.1045284632676569819, 0.000000000000000000 ) ) ;
#15443 = CIRCLE ( 'NONE', #12195, 1.000000000000000000 ) ;
#15444 = ORIENTED_EDGE ( 'NONE', *, *, #18989, .T. ) ;
#15445 = CARTESIAN_POINT ( 'NONE',  ( -23.30142641249946678, 0.5956563822689483478, -20.54734181390668724 ) ) ;
#15446 = CARTESIAN_POINT ( 'NONE',  ( -9.427394655416351910, 11.16786596286767441, 10.49999999999999822 ) ) ;
#15447 = ORIENTED_EDGE ( 'NONE', *, *, #33004, .F. ) ;
#15448 = CARTESIAN_POINT ( 'NONE',  ( 20.27907779278287492, -3.502347089416769865, -28.55884872021393051 ) ) ;
#15449 = CIRCLE ( 'NONE', #22569, 17.00000000000000000 ) ;
#15450 = EDGE_LOOP ( 'NONE', ( #13970, #17065, #34634, #3110 ) ) ;
#15451 = CARTESIAN_POINT ( 'NONE',  ( -16.50691157469147896, 29.07214648649221900, 13.32518128616527164 ) ) ;
#15452 = EDGE_CURVE ( 'NONE', #36540, #29047, #4279, .T. ) ;
#15453 = AXIS2_PLACEMENT_3D ( 'NONE', #27100, #5362, #2125 ) ;
#15454 = CARTESIAN_POINT ( 'NONE',  ( -12.01634099001141287, -16.14815750352196844, 20.94377226548377990 ) ) ;
#15455 = CARTESIAN_POINT ( 'NONE',  ( 6.868154521567912951, 35.60001939699333917, 10.49999999999999467 ) ) ;
#15456 = CARTESIAN_POINT ( 'NONE',  ( 10.77668768651791886, 26.79111211459907338, 19.66345542862663720 ) ) ;
#15457 = AXIS2_PLACEMENT_3D ( 'NONE', #31678, #1209, #4651 ) ;
#15458 = LINE ( 'NONE', #21548, #16180 ) ;
#15459 = ORIENTED_EDGE ( 'NONE', *, *, #18694, .T. ) ;
#15460 = CARTESIAN_POINT ( 'NONE',  ( 3.998603647807975392, 8.333314792924149117, 10.49999999999999822 ) ) ;
#15461 = DIRECTION ( 'NONE',  ( 1.000000000000000000, 0.000000000000000000, 0.000000000000000000 ) ) ;
#15462 = DIRECTION ( 'NONE',  ( 1.000000000000000000, 0.000000000000000000, 0.000000000000000000 ) ) ;
#15463 = DIRECTION ( 'NONE',  ( -0.000000000000000000, -0.000000000000000000, -1.000000000000000000 ) ) ;
#15464 = CARTESIAN_POINT ( 'NONE',  ( 9.105319387809036158, 35.54444977581241005, -6.303818603030153511 ) ) ;
#15465 = CARTESIAN_POINT ( 'NONE',  ( -2.256323172317922232, 14.28970123917155277, 9.000000000000001776 ) ) ;
#15466 = EDGE_CURVE ( 'NONE', #15880, #14560, #6818, .T. ) ;
#15467 = CARTESIAN_POINT ( 'NONE',  ( 13.02764125108839366, -20.75515974360676452, -19.31289340529147580 ) ) ;
#15468 = DIRECTION ( 'NONE',  ( 0.5000000000000041078, 0.8660254037844362651, 0.000000000000000000 ) ) ;
#15469 = CARTESIAN_POINT ( 'NONE',  ( -5.982165713378355676, 28.55918256678905820, 9.000000000000001776 ) ) ;
#15470 = CARTESIAN_POINT ( 'NONE',  ( -12.05736835487443237, 14.38397459621567442, 10.50000000000000000 ) ) ;
#15471 = EDGE_CURVE ( 'NONE', #34387, #15406, #37910, .T. ) ;
#15472 = CIRCLE ( 'NONE', #39490, 1.000000000000000888 ) ;
#15473 = ORIENTED_EDGE ( 'NONE', *, *, #31640, .F. ) ;
#15475 = VECTOR ( 'NONE', #23114, 1000.000000000000000 ) ;
#15474 = CARTESIAN_POINT ( 'NONE',  ( -15.11124835272140388, 26.10590699377372559, -8.767955561639961815 ) ) ;
#15476 = CARTESIAN_POINT ( 'NONE',  ( -34.14640338304366196, -7.754617911608441716, 17.42190598798312706 ) ) ;
#15477 = CARTESIAN_POINT ( 'NONE',  ( 15.18788860438108124, -26.66571922823320051, -5.000000000000000888 ) ) ;
#15478 = EDGE_CURVE ( 'NONE', #36997, #11661, #37400, .T. ) ;
#15479 = CARTESIAN_POINT ( 'NONE',  ( -3.542977516905746249, 8.236468469132606884, 10.96580508970282075 ) ) ;
#15480 = EDGE_CURVE ( 'NONE', #36412, #24952, #22452, .T. ) ;
#15481 = B_SPLINE_CURVE_WITH_KNOTS ( 'NONE', 3,
 ( #28937, #1115, #35237, #32195 ),
 .UNSPECIFIED., .F., .F.,
 ( 4, 4 ),
 ( 0.000000000000000000, 1.000000000000000000 ),
 .UNSPECIFIED. ) ;
#15482 = ORIENTED_EDGE ( 'NONE', *, *, #35193, .T. ) ;
#15483 = ORIENTED_EDGE ( 'NONE', *, *, #2944, .T. ) ;
#15484 = CIRCLE ( 'NONE', #7032, 6.000000000000015987 ) ;
#15485 = CARTESIAN_POINT ( 'NONE',  ( -11.89628958333163311, 22.12938455673445404, -18.29461116250375596 ) ) ;
#15486 = CARTESIAN_POINT ( 'NONE',  ( -12.57245947831582811, -18.18636306848776130, -23.55555282489862279 ) ) ;
#15487 = FACE_BOUND ( 'NONE', #921, .T. ) ;
#15488 = AXIS2_PLACEMENT_3D ( 'NONE', #37927, #34885, #16807 ) ;
#15489 = ORIENTED_EDGE ( 'NONE', *, *, #20360, .F. ) ;
#15490 = CARTESIAN_POINT ( 'NONE',  ( -33.38568604116227334, -10.36665845154829491, -10.23472671421048652 ) ) ;
#15491 = CARTESIAN_POINT ( 'NONE',  ( -14.78550315123711556, -25.94740016304241337, -9.240703662871906587 ) ) ;
#15492 = CARTESIAN_POINT ( 'NONE',  ( 39.05366788733157080, -6.582903524762554248, 11.00000000000000000 ) ) ;
#15493 = VERTEX_POINT ( 'NONE', #16183 ) ;
#15494 = CARTESIAN_POINT ( 'NONE',  ( 29.14303797557771958, 0.3180640978246742079, -10.66026172746647482 ) ) ;
#15495 = FACE_OUTER_BOUND ( 'NONE', #19830, .T. ) ;
#15496 = LINE ( 'NONE', #2902, #23831 ) ;
#15497 = ORIENTED_EDGE ( 'NONE', *, *, #27179, .T. ) ;
#15498 = CARTESIAN_POINT ( 'NONE',  ( -30.53010055481989937, -0.05901878607395646265, -7.825680868720071182 ) ) ;
#15499 = ORIENTED_EDGE ( 'NONE', *, *, #5073, .F. ) ;
#15500 = CARTESIAN_POINT ( 'NONE',  ( 31.22701752701838274, -1.717445521449697976, -9.600932008253289851 ) ) ;
#15501 = CARTESIAN_POINT ( 'NONE',  ( 2.113389199311633604, -20.40176566834144012, -30.00000000000001776 ) ) ;
#15502 = ADVANCED_FACE ( 'NONE', ( #38311 ), #19422, .F. ) ;
#15503 = CARTESIAN_POINT ( 'NONE',  ( 30.32526513703937709, -2.692717509694302791, 18.42518152272298693 ) ) ;
#15504 = EDGE_CURVE ( 'NONE', #7759, #11613, #7221, .T. ) ;
#15505 = ORIENTED_EDGE ( 'NONE', *, *, #17867, .T. ) ;
#15506 = CARTESIAN_POINT ( 'NONE',  ( -20.57159149025624245, 4.298814444492946585, -25.31853320033998855 ) ) ;
#15507 = EDGE_CURVE ( 'NONE', #11960, #39304, #25073, .T. ) ;
#15508 = CARTESIAN_POINT ( 'NONE',  ( -4.984135866956331817, 36.15314577889358105, 11.00000000000000000 ) ) ;
#15509 = DIRECTION ( 'NONE',  ( 1.000000000000000000, 0.000000000000000000, 0.000000000000000000 ) ) ;
#15510 = CIRCLE ( 'NONE', #28488, 1.000000000000000888 ) ;
#15511 = AXIS2_PLACEMENT_3D ( 'NONE', #33073, #39939, #39350 ) ;
#15512 = DIRECTION ( 'NONE',  ( 1.000000000000000000, 0.000000000000000000, 0.000000000000000000 ) ) ;
#15513 = CARTESIAN_POINT ( 'NONE',  ( -3.326590493086956091, 6.849639119454676184, 12.00000000000000000 ) ) ;
#15514 = VECTOR ( 'NONE', #6549, 999.9999999999998863 ) ;
#15515 = B_SPLINE_SURFACE_WITH_KNOTS ( 'NONE', 3, 3, ( 
 ( #6686, #25189, #32085, #22729, #804, #37589, #28236, #13185, #415, #4045, #19094, #16448, #10154, #34937, #31485, #3652, #16045, #37312, #18432, #24518, #34466, #6230, #21864, #9689, #33876, #31413, #30823, #27964, #36918, #37116, #6423, #39756, #36722, #40155 ),
 ( #18235, #12328, #9487, #31021, #9086, #18828, #21668, #8886, #27368, #22066, #21274, #6614, #2990, #12723, #21471, #6028, #11934, #33685, #3380, #15376, #27568, #31216, #27766, #19021, #24716, #24324, #9283, #3187, #15773, #3579, #34069, #39955, #12131, #18632 ),
 ( #15577, #137, #5835, #12527, #37512, #24918, #30629, #34269, #2786, #28163, #339, #25115, #15178, #34122, #27223, #31074, #9340, #24575, #11981, #24171, #15230, #18483, #30277, #24373, #21522, #2840, #8738, #30875, #33738, #8535, #39407, #6279, #20928, #18683 ),
 ( #30480, #21720, #12182, #3239, #14834, #36566, #33337, #2641, #15431, #2449, #30677, #15028, #3038, #33925, #15631, #23975, #27418, #24770, #27821, #5882, #8940, #39807, #18092, #36769, #11587, #33537, #36370, #27616, #5480, #21329, #17894, #36970, #40004, #39609 ),
 ( #9137, #18286, #11784, #12379, #6080, #21127, #4809, #37165, #5681, #25170, #28214, #19268, #37763, #31863, #13374, #31667, #9934, #28615, #10133, #16232, #19075, #22316, #31269, #16428, #34715, #18878, #6868, #22510, #9540, #32065, #28414, #3631, #993, #34518 ),
 ( #21918, #38161, #3832, #4026, #589, #12579, #785, #3432, #25763, #13168, #28818, #25361, #15830, #192, #6668, #25563, #31467, #7268, #12775, #37962, #10331, #4234, #16028, #7071, #34920, #22712, #19469, #35116, #19671, #28017, #24971, #37364, #34320, #6474 ),
 ( #394, #37566, #9736, #22119, #12972, #14182, #39163, #20285, #38563, #26773, #38361, #13574, #16840, #11346, #29621, #22916, #13980, #23332, #4839, #29222, #17248, #32886, #32483, #20492, #33089, #4639, #23728, #7475, #26577, #1598, #35728, #7686, #35925, #23121 ),
 ( #19882, #5040, #38766, #32274, #26371, #11142, #10532, #20695, #17041, #29422, #29822, #35522, #13776, #36127, #26169, #17451, #32684, #20087, #35317, #8290, #10947, #4438, #25960, #16637, #8083, #10736, #1391, #2007, #7879, #14386, #1799, #38968, #23527, #29020 ),
 ( #1194, #24529, #30636, #15385, #36927, #27777, #33884, #27577, #2794, #11941, #15186, #11544, #23931, #33292, #37123, #40164, #39962, #18046, #30232, #21283, #9093, #36327, #30439, #12139, #8893, #14791, #21478, #39762, #14590, #5242, #12335, #26979, #24723, #8695 ),
 ( #9292, #18243, #21677, #20890, #2401, #39365, #36523, #6036, #8491, #36729, #21087, #18441, #30831, #17654, #30027, #33495, #2997, #2204, #24332, #14987, #5634, #33692, #2601, #5445, #17853, #27181, #39566, #27374, #11742, #24127, #5841, #3589, #25122, #12730 ),
 ( #3197, #16186, #28570, #31614, #16385, #37719, #15781, #3983, #15586, #31030, #34278, #28770, #6823, #146, #31422, #545, #22265, #6432, #34670, #10087, #9698, #37915, #10284, #22074, #946, #24927, #3784, #19029, #12929, #37521, #13122, #349, #15984, #34078 ),
 ( #37322, #28365, #744, #27971, #38112, #34474, #6622, #7023, #25320, #31224, #13326, #3388, #22467, #9885, #19224, #12535, #25718, #25513, #9495, #21871, #6237, #34872, #28172, #18836, #19425, #31818, #18639, #32435, #20242, #4594, #16589, #10486, #16994, #11098 ),
 ( #32842, #14136, #4995, #23481, #4793, #7834, #29373, #32640, #28971, #1146, #22868, #14338, #17406, #17200, #35477, #7428, #38723, #1755, #13529, #7633, #29577, #26329, #32225, #26534, #1549, #32020, #22666, #29782, #4186, #1962, #26120, #8036, #4388, #16793 ),
 ( #38314, #19837, #25917, #13728, #38922, #35271, #10899, #29179, #26730, #1345, #19625, #38515, #39116, #35680, #10691, #20040, #13933, #23285, #23078, #35878, #20444, #35070, #7224, #27722, #27131, #18391, #2155, #8847, #36477, #18000, #2358, #30588, #17807, #21038 ),
 ( #39910, #33447, #14537, #5589, #5793, #33047, #15333, #11696, #39519, #24477, #30183, #8448, #30782, #20846, #12088, #27329, #14742, #29975, #2946, #24083, #26932, #8240, #5983, #2745, #33245, #20646, #36873, #8645, #15138, #30387, #21233, #2554, #5197, #39319 ),
 ( #27528, #36677, #21429, #9046, #33835, #11301, #33644, #18195, #14941, #23682, #17606, #11496, #23881, #36080, #36286, #5394, #39717, #11893, #24281, #19172, #30976, #12680, #22214, #3536, #9444, #31566, #34424, #9239, #40110, #34817, #21626, #19373, #3339, #25461 ),
 ( #12878, #31772, #15538, #37269, #34030, #31174, #16134, #3142, #31371, #15731, #3732, #34618, #16335, #24676, #28120, #37861, #28518, #6574, #9647, #298, #18786, #37471, #6969, #34228, #10034, #28317, #12287, #18980, #25274, #6187, #18592, #27922, #3934, #22413 ),
 ( #99, #25075, #6771, #21823, #37070, #12481, #15934, #693, #22025, #498, #37667, #13070, #9836, #24875, #6379, #11051, #22822, #19782, #23435, #1498, #20397, #4133, #25866, #22619, #32177, #4746, #19576, #19990, #4339, #20191, #23237, #4949, #13273, #16744 ),
 ( #28920, #26068, #13889, #7788, #35026, #7178, #38063, #10845, #35630, #26277, #35827, #32386, #10437, #38875, #10233, #25665, #1098, #7984, #38672, #31968, #38469, #35425, #16944, #13478, #29328, #17153, #29125, #32587, #28717, #1297, #32791, #16538, #29529, #13680 ),
 ( #1704, #35218, #10642, #896, #38269, #23025, #14084, #26481, #7379, #7585, #4543, #39269, #15086, #18150, #27477, #33398, #32997, #11247, #39863, #11652, #21187, #30134, #1910, #5540, #5148, #30540, #27084, #33592, #14693, #17554, #29731, #23834, #24033, #8400 ),
 ( #39473, #23636, #29928, #36429, #5744, #14488, #27284, #20797, #26881, #24430, #8592, #11843, #12040, #24232, #39068, #21383, #17759, #33194, #2699, #36240, #11448, #36823, #5345, #8996, #17951, #2307, #36033, #33790, #20991, #20599, #14288, #17355, #8800, #30336 ),
 ( #2508, #26680, #14895, #39669, #36630, #8192, #2108, #250, #34571, #3095, #15888, #37224, #15490, #13026, #25026, #451, #28470, #12433, #9987, #9395, #6528, #27875, #15683, #25226, #18339, #15286, #18739, #12833, #47, #5938, #18540, #9595, #37624, #28071 ),
 ( #27674, #30733, #645, #40061, #25417, #21773, #31524, #24825, #34178, #2896, #12238, #22172, #6330, #6135, #9792, #31128, #37815, #3291, #24628, #12637, #21977, #6722, #22367, #37419, #30930, #34378, #18933, #31321, #19131, #37022, #9192, #21578, #28274, #3687 ),
 ( #3491, #33980, #16085, #35378, #22570, #7327, #11001, #32333, #1252, #10189, #7738, #13428, #31723, #35580, #32126, #3886, #31918, #34979, #26020, #4291, #38620, #20142, #38420, #16691, #7535, #16898, #22975, #25822, #29075, #38016, #23179, #13633, #25617, #10592 ),
 ( #7129, #19938, #38222, #26225, #29279, #34773, #19328, #22770, #32541, #10795, #4495, #1448, #10391, #35172, #13833, #29477, #28874, #4696, #17100, #6922, #1653, #16284, #14035, #26426, #19527, #19734, #28670, #38822, #845, #4085, #13225, #16489, #1049, #24731 ),
 ( #39770, #27786, #152, #11949, #31039, #14237, #21486, #8900, #30643, #14994, #3004, #29874, #33699, #23386, #32739, #27382, #33892, #24538, #37130, #18646, #5097, #17505, #21685, #9302, #34086, #39969, #39018, #17304, #6244, #18252, #40171, #36737, #7935, #12147 ),
 ( #5848, #12342, #21292, #11196, #35781, #2608, #2801, #24339, #3205, #8138, #27585, #15593, #20345, #15194, #15392, #9100, #27979, #4896, #29678, #1860, #6044, #18449, #36934, #30838, #26628, #23587, #35983, #20546, #32939, #37923, #25328, #37529, #28578, #31826 ),
 ( #25129, #16194, #3992, #22274, #13130, #25522, #34880, #752, #10095, #22475, #35080, #6630, #3597, #7234, #7034, #4196, #28178, #9705, #6438, #19634, #19038, #16599, #15994, #19433, #22083, #34678, #16393, #24935, #21877, #37727, #28779, #34483, #12542, #31430 ),
 ( #28373, #955, #6831, #34285, #37328, #32030, #18843, #28980, #554, #38120, #12937, #9894, #9502, #31231, #13334, #19232, #12736, #25727, #31625, #3394, #3793, #15788, #10294, #22677, #357, #17617, #4604, #13740, #1355, #38732, #14146, #20456, #35281, #7439 ),
 ( #11311, #29586, #13539, #10908, #1156, #26544, #1764, #29188, #13943, #25926, #38932, #7845, #16804, #14349, #20050, #38326, #1971, #23295, #10497, #38525, #26129, #32649, #35689, #5004, #26740, #4805, #20252, #11108, #23492, #35887, #32445, #17210, #4397, #29792 ),
 ( #8045, #39126, #36093, #23087, #35486, #23692, #8250, #20657, #32852, #10701, #19846, #33058, #17415, #5207, #26338, #22877, #32235, #7644, #17004, #29384, #1559, #27340, #17818, #2165, #36488, #24292, #21049, #9252, #14753, #33654, #2957, #6197, #33458, #9057 ),
 ( #21440, #40120, #18401, #12101, #15148, #39530, #30195, #33848, #5602, #21636, #18010, #14549, #27143, #5805, #5994, #29988, #30398, #2369, #11706, #39728, #2756, #30793, #23891, #36296, #39331, #24487, #36885, #27539, #12300, #18207, #24094, #24686, #11508, #26943 ),
 ( #39921, #36690, #5405, #15344, #8655, #8458, #27734, #11903, #20857, #2567, #14951, #21245, #8858, #37082, #34041, #30599, #33256, #19185, #703, #6781, #9658, #28328, #21834, #6979, #508, #9455, #12889, #13081, #109, #22628, #18992, #34435, #31782, #25086 ),
 ( #28131, #19383, #34630, #37482, #37280, #10243, #22036, #34238, #15548, #13282, #10046, #15742, #27934, #3944, #6586, #22423, #25285, #16144, #37677, #12492, #6389, #9848, #16344, #309, #28530, #31381, #12691, #25677, #22225, #25472, #906, #3547, #35036, #15946 ),
 ( #18603, #28725, #3742, #31576, #3351, #37871, #34829, #18799, #38072, #30986, #3154, #24886, #31184, #1508, #16548, #7187, #1919, #28929, #26689, #10652, #32801, #16755, #29134, #19586, #1110, #23445, #31978, #35435, #4959, #38884, #13898, #16954, #38479, #26078 ),
 ( #13487, #29538, #1716, #4756, #29740, #10854, #1308, #17366, #25876, #4142, #7388, #14299, #20200, #38279, #4553, #26287, #35639, #19791, #7800, #35836, #23034, #11061, #23644, #7594, #39079, #10447, #17163, #32397, #38682, #19999, #26490, #13689, #29337, #22831 ),
 ( #23246, #35229, #32597, #14094, #32187, #11256, #7995, #20406, #4348, #2315, #33202, #2904, #5354, #24438, #11852, #14703, #14498, #27682, #27093, #39279, #33007, #30743, #27486, #17767, #5156, #21392, #11660, #39871, #5550, #33601, #17959, #29936, #23844, #30347 ),
 ( #21197, #5947, #12048, #18349, #36833, #18158, #5753, #2516, #30550, #2117, #26889, #36248, #40070, #15294, #2707, #8603, #20805, #24241, #15097, #11457, #21000, #9004, #39679, #30144, #33799, #14904, #17563, #36041, #12247, #8410, #8202, #39482, #20608, #24045 ),
 ( #36437, #33407, #27293, #36639, #8808, #653, #15498, #15896, #28080, #16094, #19140, #853, #57, #21782, #18548, #15691, #13035, #27884, #28283, #258, #28479, #31532, #24636, #9202, #12646, #9995, #25425, #18942, #34386, #25034, #3301, #21985, #19337, #18748 ),
 ( #22180, #6929, #459, #6338, #34781, #6146, #21586, #24835, #31730, #37632, #30938, #6537, #31329, #12843, #37233, #25234, #37822, #37428, #22374, #37033, #9604, #3893, #12442, #34581, #3500, #9801, #6732, #3696, #31136, #16292, #33988, #3104, #28677, #9403 ),
 ( #34186, #35179, #7335, #11009, #14043, #23394, #29287, #28881, #7136, #35789, #7545, #17109, #26029, #38023, #1457, #1057, #26434, #22982, #29486, #10600, #13435, #25625, #16906, #35590, #35386, #10804, #19945, #19535, #25830, #32343, #1662, #10399, #23189, #4298 ),
 ( #4503, #7746, #7944, #19741, #17312, #16699, #13842, #22778, #26233, #32549, #10196, #22578, #38428, #20150, #32136, #13233, #38229, #38629, #4705, #38833, #20353, #32748, #4905, #29686, #34987, #31925, #4093, #29083, #1259, #16498, #13641, #33753, #5106, #39027 ),
 ( #39424, #29885, #24390, #17513, #36783, #8955, #21348, #26837, #5496, #15045, #18303, #33150, #21144, #27238, #12000, #33551, #5899, #30497, #24187, #39626, #8551, #11802, #8148, #20554, #2067, #1869, #14247, #36584, #14652, #39228, #17910, #5698, #32948, #27041 ),
 ( #18109, #11608, #2464, #14852, #8755, #30294, #2658, #27436, #26638, #36189, #5304, #11204, #39822, #23595, #14443, #11407, #35991, #17714, #23790, #8358, #33353, #30089, #20758, #2263, #23991, #36388, #20947, #16044, #22136, #24988, #208, #21734, #9355, #28035 ),
 ( #12794, #25188, #28235, #12989, #34342, #12395, #610, #12197, #27637, #30890, #25380, #3452, #36986, #12597, #37383, #18895, #3054, #31287, #6685, #6292, #34535, #6885, #18699, #37778, #21538, #414, #15648, #9557, #34142, #9755, #37183, #21934, #30693, #40018 ),
 ( #33938, #6490, #37587, #24593, #34734, #31092, #3256, #3651, #15848, #27839, #9949, #12, #19093, #31484, #28431, #9152, #22330, #2858, #15246, #24784, #6097, #18501, #15445, #29435, #35336, #34936, #13184, #1613, #13592, #23141, #32084, #3852, #7494, #7089 ),
 ( #13996, #10753, #16447, #19486, #32500, #22936, #1410, #29036, #16861, #1212, #25579, #31882, #25979, #7700, #28833, #29238, #10352, #1010, #26385, #38379, #13793, #38783, #25783, #23348, #22728, #19899, #13391, #10553, #38580, #31681, #28633, #4251, #26186, #38177 ),
 ( #32293, #35538, #4454, #20102, #4656, #17058, #10960, #35742, #19286, #16249, #35135, #7286, #803, #37978, #10153, #4043, #19688, #22525, #16654, #24140, #38983, #39381, #11359, #39582, #2414, #24345, #32700, #36142, #33507, #11755, #2218, #17669, #39180, #26788 ),
 ( #17264, #30246, #14805, #5457, #30451, #11559, #29838, #18059, #29637, #4852, #8097, #2613, #20902, #14196, #5256, #14605, #36342, #20506, #8505, #36537, #23743, #8708, #7897, #8311, #15001, #11155, #17864, #33105, #26994, #20709, #27192, #14402, #30044, #20301 ),
 ( #23946, #23546, #33306, #21099, #1816, #26592, #27388, #35940, #39778, #5649, #11955, #17465, #2022, #32904, #5056, #12743, #6053, #36940, #15795, #27792, #28383, #40177, #21299, #33897, #158, #25137, #12943, #12349, #9106, #21492, #34091, #9507, #28185, #30650 ),
 ( #30844, #6637, #24940, #8909, #6251, #36743, #21887, #37335, #24545, #9308, #33704, #34291, #3211, #12154, #9711, #15401, #5855, #37537, #18654, #18257, #18454, #3010, #27985, #31047, #362, #22091, #12549, #15600, #6445, #18849, #31237, #24736, #3401, #39977 ),
 ( #27590, #34489, #19045, #2808, #560, #37136, #21693, #31436, #3603, #15999, #15201, #35444, #14303, #1723, #4558, #3801, #17570, #32403, #28585, #22282, #20613, #17372, #23039, #13695, #39084, #29543, #8001, #35646, #23451, #7804, #19238, #26083, #20207, #26696 ),
 ( #36046, #29744, #8209, #11262, #20411, #11066, #32603, #35841, #31633, #16199, #38483, #29942, #33012, #32806, #38689, #10658, #14099, #4965, #757, #10862, #1926, #26496, #7599, #23650, #5161, #20004, #2122, #25334, #37734, #16961, #38890, #9902, #34684, #29342 ),
 ( #6836, #1513, #13903, #26293, #4761, #23250, #17168, #21006, #18554, #17966, #15105, #11666, #24249, #33805, #26895, #23849, #27298, #9010, #36444, #14503, #27098, #18164, #5954, #36644, #27492, #39877, #36839, #30555, #12053, #24445, #37039, #8611, #5555, #9210 ),
 ( #30149, #24051, #8416, #30353, #30751, #5360, #5758, #2521, #18356, #21399, #30946, #39283, #14910, #40078, #2910, #8814, #21202, #39687, #33413, #11858, #21594, #33608, #24644, #2714, #11463, #15301, #36252, #27689, #12253, #2321, #33996, #20810, #6153, #33212 ),
 ( #17774, #14710, #39487, #266, #34392, #6347, #21992, #15903, #18754, #31338, #12451, #25040, #31145, #15698, #34194, #9611, #21789, #3307, #3111, #27891, #28087, #6544, #37437, #18948, #3507, #12652, #15506, #64, #24843, #37240, #9409, #2334, #20421, #39497 ),
 ( #23660, #35656, #39295, #26509, #24062, #20624, #14719, #8217, #38900, #11473, #11076, #36057, #27308, #8426, #17581, #23460, #36456, #29759, #7814, #11674, #33025, #20217, #8013, #35852, #2131, #5173, #27108, #8622, #14515, #29953, #23859, #33222, #36263, #1936 ),
 ( #32614, #14314, #20822, #5370, #21017, #5567, #32817, #4973, #33426, #17976, #26908, #30365, #10873, #17178, #2532, #17785, #14919, #30161, #4771, #23262, #17384, #29554, #1733, #14111, #26706, #39094, #11276, #2725, #34403, #22004, #18960, #24454, #3121, #12661 ),
 ( #28097, #36851, #9422, #30763, #9023, #6554, #18568, #34204, #31348, #5963, #3517, #2924, #76, #21408, #9219, #18765, #11870, #8824, #12267, #6357, #33815, #39697, #12065, #15518, #31154, #21604, #12460, #24853, #21802, #27900, #37249, #3318, #15914, #18368 ),
 ( #15312, #24259, #21211, #15709, #27698, #39888, #276, #40090, #36656, #24655, #33621, #37049, #25053, #37448, #5771, #34009, #6167, #30953, #9624, #18173, #30565, #15116, #27505, #37648, #10417, #22798, #25847, #10621, #31945, #10014, #38448, #32365, #874, #29104 ),
 ( #23002, #22597, #32157, #13253, #12859, #16518, #3711, #1277, #38043, #4317, #25645, #16112, #35405, #31547, #7564, #19965, #4524, #13050, #4111, #13660, #28299, #19354, #7356, #13454, #475, #19759, #25253, #16720, #35198, #38248, #35006, #26048, #34598, #6751 ),
 ( #9818, #22195, #19155, #10212, #28498, #22394, #671, #25440, #28901, #37839, #7156, #1078, #34797, #6947, #31751, #3913, #16312, #28695, #19554, #8525, #39995, #30472, #9127, #33123, #14627, #10823, #20920, #33728, #8332, #8729, #33326, #8932, #11975, #33917 ),
 ( #5473, #30064, #17688, #14827, #2632, #36762, #23212, #36162, #26255, #39798, #24365, #15020, #12174, #21120, #39398, #27610, #38651, #13866, #2239, #24568, #27410, #20732, #27213, #24161, #5672, #27015, #18082, #5875, #17886, #21323, #16924, #30269, #36963, #5276 ),
 ( #39602, #18278, #30670, #2832, #2437, #11776, #11579, #15224, #36558, #23967, #33528, #21514, #36362, #29307, #1479, #21907, #9331, #777, #28605, #25552, #31066, #9729, #19258, #22500, #37356, #25353, #31458, #16223, #37755, #13159, #34707, #28406, #3624, #12766 ),
 ( #9531, #6659, #3230, #15820, #9925, #18477, #15421, #18870, #582, #28008, #6072, #18674, #22110, #22306, #28207, #19068, #16019, #12963, #34510, #6858, #31658, #37953, #181, #34312, #10125, #3823, #30867, #21713, #15621, #40198, #6465, #3029, #37157, #37558 ),
 ( #12570, #27814, #12371, #24758, #31261, #24962, #6271, #3424, #34115, #386, #25161, #984, #4017, #17032, #29411, #32475, #17237, #38554, #16628, #4830, #16419, #31855, #35106, #29612, #7675, #13365, #32263, #1383, #23113, #7260, #35512, #10938, #10522, #38756 ),
 ( #4427, #23323, #20276, #10727, #16832, #20077, #1587, #4630, #25952, #29213, #38150, #35718, #13766, #25754, #26157, #13971, #28807, #38959, #35307, #22905, #11131, #7466, #7871, #26363, #4225, #32676, #1789, #13565, #10322, #26569, #1184, #22703, #19660, #14172 ),
 ( #32055, #34910, #7062, #29008, #19459, #38351, #19874, #23519, #18230, #5030, #2782, #26969, #8881, #33081, #5232, #35914, #32876, #39752, #17645, #23720, #2591, #14580, #15173, #39357, #8074, #20686, #27170, #11929, #39949, #11533, #36118, #8278, #20881, #36514 ),
 ( #33284, #30622, #30017, #33680, #11732, #20482, #5434, #17441, #8684, #24117, #11335, #36319, #29814, #21076, #30222, #39153, #36717, #2192, #1998, #24320, #17842, #14376, #23920, #8482, #14781, #2391, #27364, #21270, #39555, #33483, #5625, #18034, #30429, #14975 ),
 ( #5831, #27564, #26763, #21860, #6608, #33871, #16172, #12523, #27959, #28557, #24912, #12916, #3575, #21661, #532, #28158, #31017, #30819, #3769, #18628, #15372, #9081, #6806, #15971, #9279, #40150, #25309, #15768, #34461, #34265, #9685, #6419, #6022, #12324 ),
 ( #31406, #37508, #22251, #28352, #34655, #37706, #19017, #22062, #18824, #9870, #18427, #2984, #24711, #12127, #19211, #31600, #37306, #37111, #334, #24513, #27762, #9481, #36913, #31210, #21466, #34065, #6224, #3375, #12715, #3183, #15572, #25111, #131, #1332 ),
 ( #32006, #10472, #3969, #29358, #22854, #31804, #35259, #35464, #22451, #4780, #1134, #16575, #17188, #13513, #1536, #32422, #10270, #13921, #16779, #19612, #19408, #32626, #7211, #16369, #37898, #35667, #4579, #38097, #28756, #26315, #4373, #23061, #7413, #38503 ),
 ( #38708, #731, #4171, #20025, #26104, #10887, #16981, #23270, #7822, #7620, #10678, #19823, #20227, #7008, #930, #13308, #13109, #25499, #10072, #25903, #25703, #29163, #34860, #22651, #38301, #35056, #13714, #28954, #32210, #23870, #38909, #29563, #24270, #11086 ),
 ( #23670, #20634, #11878, #2343, #21220, #4983, #26718, #23469, #33034, #5575, #20430, #20832, #5183, #21026, #24071, #5780, #14122, #17594, #14929, #33435, #36272, #39305, #29963, #8228, #26917, #36664, #36066, #39705, #17796, #1742, #11483, #26521, #14729, #30170 ),
 ( #29767, #8834, #27119, #35862, #8436, #33234, #39506, #1949, #2142, #8024, #33631, #14526, #32827, #17394, #14324, #17985, #39103, #11287, #2540, #5380, #11683, #36464, #8633, #30376, #27316, #5971, #12468, #6561, #15320, #28106, #9226, #27706, #25258, #37257 ),
 ( #24861, #3327, #24464, #36862, #18377, #9823, #28304, #15716, #30962, #2931, #34212, #37456, #9031, #3129, #284, #21809, #40099, #9632, #9430, #27514, #18182, #12865, #39898, #37654, #21612, #3524, #12275, #24662, #30575, #12074, #34410, #37058, #30771, #22012 ),
 ( #34017, #2733, #6174, #6367, #18967, #34605, #18575, #15526, #27909, #84, #31162, #31355, #21417, #33823, #18772, #12668, #25061, #15920, #482, #22201, #15124, #16931, #28503, #3717, #6952, #1485, #19769, #13056, #4119, #13461, #35203, #19360, #7363, #23010 ),
 ( #31757, #38254, #16524, #10627, #32373, #10423, #28907, #32163, #29111, #4324, #38048, #1085, #10021, #35412, #25853, #37845, #22806, #1283, #676, #10831, #7163, #22605, #23221, #19561, #7570, #38454, #16318, #19974, #16728, #13665, #26055, #4529, #25445, #34802 ),
 ( #29315, #13874, #26264, #38658, #6757, #19160, #31552, #16120, #22399, #3919, #28703, #881, #13260, #25652, #10218, #35012, #31951, #20383, #11436, #14681, #26464, #8179, #17744, #39256, #4936, #27070, #29915, #4732, #35618, #30322, #17139, #14882, #39056, #20977 ),
 ( #8387, #27268, #11038, #32778, #29516, #26666, #11638, #38862, #26867, #11233, #39456, #30121, #11828, #20177, #23623, #33384, #24019, #2095, #5135, #36021, #14275, #32981, #2493, #29716, #5527, #23819, #7775, #17541, #32574, #20784, #36224, #23422, #20585, #1691 ),
 ( #14068, #14475, #33181, #5331, #7971, #2293, #36415, #8578, #17939, #35814, #39655, #17340, #1898, #21761, #9181, #30919, #15275, #3279, #30722, #33966, #24217, #33577, #27663, #34167, #24814, #37408, #18922, #5926, #18326, #21966, #25013, #27865, #238, #439 ),
 ( #18527, #28059, #37010, #8784, #12422, #39851, #9582, #6123, #12624, #21566, #12027, #6514, #27463, #31310, #3479, #3082, #37211, #9381, #6318, #35, #18726, #31116, #15876, #2884, #40047, #28262, #15672, #36615, #24417, #21372, #18137, #12226, #34367, #15073 ),
 ( #21174, #33777, #5728, #30526, #2686, #24618, #36811, #8982, #15474, #25813, #32114, #6711, #19120, #22160, #35161, #7316, #10380, #35367, #16477, #34762, #22963, #34561, #9780, #13017, #7522, #38211, #31514, #10180, #19516, #1038, #25406, #13419, #29064, #28660 ),
 ( #832, #19927, #3677, #22757, #38006, #31907, #3877, #4278, #19315, #22558, #12820, #16071, #16273, #19723, #16682, #26008, #32322, #6913, #31710, #10581, #13623, #28862, #1241, #29268, #28459, #4484, #7118, #38406, #25606, #37615, #16888, #635, #25214, #34966 ),
 ( #9976, #37803, #22355, #13212, #4074, #11184, #39209, #23575, #35566, #29463, #35972, #30072, #38811, #11389, #32728, #10988, #8533, #20533, #36171, #23973, #7925, #5479, #4882, #2047, #23376, #8126, #20738, #13820, #10784, #14224, #8338, #35770, #1437, #14023 ),
 ( #5085, #14425, #23770, #36369, #20334, #17294, #20927, #26819, #33335, #17088, #29667, #7728, #1849, #17696, #32530, #32930, #26616, #33132, #5282, #17893, #26214, #39008, #27024, #2246, #17494, #29863, #14633, #39406, #11586, #38607, #23168, #20132, #4685, #1642 ),
 ( #26417, #191, #11782, #27221, #30478, #24970, #3036, #36564, #27615, #36968, #18482, #2640, #30874, #6278, #5881, #34121, #7018, #18284, #37363, #21126, #27820, #15229, #9136, #21328, #9339, #36767, #40002, #30275, #39608, #33736, #8050, #15430, #3237, #9539 ),
 ( #30676, #2838, #34319, #12181, #31073, #21719, #39806, #18682, #6078, #8939, #8737, #21917, #24574, #33535, #24170, #2448, #15630, #27417, #18091, #28015, #33924, #12378, #21519, #24768, #37164, #5680, #15026, #12577, #14833, #11980, #24372, #10482, #16584, #26529 ),
 ( #4589, #26115, #16990, #25714, #38108, #7220, #11094, #29571, #29368, #32220, #4181, #35473, #38717, #10279, #4383, #1545, #23070, #28966, #10895, #13724, #28765, #19421, #4789, #1142, #13523, #31813, #941, #35676, #25913, #19620, #23278, #22863, #23477, #35267 ),
 ( #13929, #35873, #3979, #7422, #17196, #7830, #38511, #29175, #19831, #38310, #16787, #14130, #1340, #1751, #7628, #16379, #10686, #13319, #26323, #20034, #32014, #32431, #22662, #20238, #32635, #35065, #38917, #26927, #4991, #8842, #5388, #17402, #5191, #8236 ),
 ( #11886, #33640, #11692, #17803, #8640, #30383, #36471, #39313, #30177, #11297, #36671, #2353, #39111, #14737, #2548, #29775, #12082, #8444, #23877, #24472, #20839, #21228, #39712, #17601, #5787, #24078, #11492, #26725, #39905, #14533, #23677, #1958, #2741, #24277 ),
 ( #18191, #21033, #14937, #27127, #5583, #39513, #14332, #36075, #33442, #30583, #29970, #17995, #36280, #2150, #15133, #27324, #27522, #8032, #33241, #20439, #32836, #20642, #33041, #6374, #15929, #9040, #5979, #9438, #31365, #18584, #36869, #9235, #293, #28311 ),
 ( #31169, #18386, #21425, #31560, #30778, #16129, #93, #18975, #12675, #37465, #6568, #19167, #30970, #27917, #3726, #9640, #28512, #12282, #34025, #2939, #12476, #12873, #27715, #28114, #24870, #492, #3531, #13064, #33831, #37264, #22209, #25266, #3334, #18779 ),
 ( #15328, #40106, #24672, #37662, #9830, #34418, #686, #25069, #3136, #6766, #37065, #21620, #6181, #15533, #22019, #21817, #34221, #15726, #34613, #38057, #13675, #1492, #1093, #29323, #1699, #13472, #32581, #16327, #23018, #10432, #32171, #16532, #4537, #31960 ),
 ( #28711, #13883, #7371, #889, #35212, #19984, #6963, #29524, #25861, #38263, #25454, #22816, #26272, #16939, #35020, #38665, #1291, #4127, #3929, #17146, #28915, #13268, #22408, #20186, #10838, #22614, #25660, #23230, #29120, #7578, #19777, #35420, #4332, #19368 ),
 ( #16738, #35625, #10636, #7782, #4740, #37855, #10029, #32380, #34810, #26063, #31766, #10227, #7173, #19570, #38463, #24226, #39465, #26875, #39063, #30128, #33393, #4944, #39264, #36423, #17753, #23630, #5535, #8395, #36028, #14282, #17946, #5142, #5738, #17548 ),
 ( #8587, #30534, #38869, #2103, #39664, #30329, #20791, #23826, #29922, #32991, #11443, #8795, #8186, #36623, #2302, #26474, #36233, #14075, #11646, #14688, #1905, #33189, #11046, #24028, #5339, #29725, #27278, #14482, #23430, #14889, #27077, #35822, #11241, #26675 ),
 ( #2502, #11837, #20984, #21182, #33585, #18145, #7978, #20391, #32785, #17348, #20593, #24821, #33784, #12429, #37415, #24425, #6718, #3088, #18535, #19126, #15485, #3486, #34373, #12233, #31317, #18734, #21573, #21378, #34568, #9188, #5933, #39857, #37621, #6524 ),
 ( #25223, #18334, #9788, #22169, #2693, #27669, #6324, #15882, #15081, #33974, #21973, #28066, #12827, #18929, #27470, #28269, #25021, #245, #9388, #12630, #8990, #30729, #2890, #12034, #36817, #9589, #27871, #40055, #31124, #446, #15282, #43, #24624, #3287 ),
 ( #15679, #37017, #6130, #30925, #37218, #21769, #34174, #25612, #22565, #13828, #4288, #23175, #6919, #28667, #840, #31719, #22766, #1046, #35373, #16894, #35168, #13425, #32121, #13630, #19730, #34974, #25819, #34770, #19935, #38219, #22361, #10386, #26016, #13023 ),
 ( #29276, #32328, #7324, #7531, #7735, #37812, #1443, #16688, #4492, #4081, #16079, #29070, #19322, #26221, #1249, #38615, #28870, #3883, #10792, #16281, #35574, #31521, #3683, #13221, #38415, #28467, #642, #7125, #10588, #22971, #25413, #9983, #38013, #10186 ),
 ( #19524, #31915, #16484, #26423, #7931, #11792, #30283, #5291, #32936, #4890, #36178, #39412, #10998, #5093, #2251, #23778, #29675, #11595, #14431, #29472, #20138, #14839, #1648, #39614, #23582, #5486, #1855, #14233, #32538, #14032, #36377, #26624, #20341, #23981 ),
 ( #11395, #35979, #8541, #14638, #36572, #4692, #8132, #17899, #20935, #26826, #29870, #11192, #39015, #17502, #27229, #20542, #2454, #8344, #17095, #2056, #38818, #17703, #20748, #32734, #39216, #23382, #30078, #33138, #35778, #33343, #27031, #17301, #24177, #6085 ),
 ( #15034, #18097, #31079, #3247, #6283, #31277, #12383, #30683, #18886, #30486, #5686, #8945, #3440, #21724, #27426, #18490, #15435, #37170, #21334, #9344, #24977, #24580, #12585, #25179, #36975, #15837, #39812, #18688, #33929, #27826, #40009, #28023, #15235, #30879 ),
 ( #12187, #15637, #34129, #21924, #28221, #2847, #27622, #6481, #9548, #24774, #11987, #3043, #18292, #37370, #199, #9141, #24378, #401, #21526, #36774, #2647, #12782, #34327, #5887, #33744, #8744, #21132, #33542, #3, #35123, #19477, #31474, #25369, #31873 ),
 ( #22720, #7484, #29027, #19889, #25968, #19678, #7278, #4034, #32073, #3638, #16035, #37770, #29229, #32282, #4241, #10141, #22323, #13381, #16645, #28421, #22517, #1202, #1001, #6875, #13581, #16437, #6676, #37573, #4445, #19082, #16848, #793, #22926, #19275 ),
 ( #1398, #12980, #34723, #598, #28623, #38368, #9942, #28825, #13176, #10541, #35324, #13784, #22126, #25571, #9745, #34526, #25771, #7078, #37969, #16242, #31674, #3839, #34927, #38169, #10338, #2406, #17254, #5249, #11352, #36334, #17660, #8498, #14596, #8297 ),
 ( #32691, #30237, #29628, #26779, #23339, #35932, #30035, #38572, #35528, #38976, #20702, #7886, #26176, #38773, #29829, #2210, #8089, #39170, #23734, #33095, #2014, #36133, #26985, #20896, #20292, #1806, #33297, #39371, #17858, #1604, #35735, #20093, #14189, #11550 ),
 ( #26583, #10743, #4845, #14394, #23937, #23130, #11147, #10953, #26377, #23535, #5451, #7693, #32491, #4645, #17048, #29428, #13988, #20498, #32892, #5047, #17457, #34084, #24132, #39572, #30444, #18644, #21484, #8700, #2799, #27583, #9098, #2606, #33890, #12340 ),
 ( #18051, #12145, #15192, #40169, #9299, #24535, #39967, #6042, #30836, #18447, #36735, #36932, #5639, #24729, #3002, #21093, #15390, #27783, #36529, #15591, #33697, #21288, #37128, #5846, #33501, #21683, #27380, #6242, #31035, #8898, #14992, #3203, #11947, #39768 ),
 ( #27977, #30641, #24337, #14796, #18250, #27186, #11749, #39987, #30859, #6457, #24558, #18664, #12756, #34502, #12561, #31057, #9522, #31251, #37348, #40189, #3222, #12164, #37550, #15611, #36954, #27999, #3415, #30661, #12955, #9322, #24749, #28196, #37147, #15215 ),
 ( #173, #25149, #21704, #33720, #21898, #9119, #22101, #24953, #9721, #6263, #21503, #31449, #33909, #3615, #16011, #28394, #6063, #34303, #6650, #25344, #12361, #378, #18861, #19058, #572, #8921, #21313, #15811, #5865, #18270, #2822, #27603, #18467, #3021 ),
 ( #15411, #27804, #34106, #10311, #32254, #19449, #37745, #10114, #1173, #16820, #7250, #38341, #10511, #19864, #13555, #22894, #7455, #20067, #31844, #28797, #32463, #35297, #29401, #13150, #34897, #31645, #973, #13755, #28595, #28997, #13353, #29203, #4416, #13960 ),
 ( #25744, #22491, #37941, #35095, #1371, #26146, #3812, #16212, #6849, #38544, #10716, #23103, #4620, #25942, #4007, #7664, #19248, #34695, #7052, #17019, #35503, #767, #19650, #4213, #1575, #16409, #25542, #38138, #9916, #22295, #22694, #32046, #16618, #14567 ),
 ( #23707, #17224, #8062, #23906, #1780, #36108, #30208, #11720, #30005, #8266, #26957, #8471, #39344, #17430, #20673, #29601, #14769, #33070, #14161, #5221, #20871, #7861, #30415, #26752, #1987, #5424, #14366, #32664, #17633, #35904, #27158, #2181, #5020, #4821 ),
 ( #26560, #39543, #11523, #2380, #36308, #38949, #8672, #11121, #21065, #33471, #5613, #23506, #33271, #24106, #2580, #29804, #17830, #36503, #18024, #26353, #38747, #10927, #23313, #35707, #20265, #20471, #32864, #39142, #11325, #6598, #25099, #122, #27752, #39936 ),
 ( #36901, #14963, #27553, #18618, #34255, #24701, #15561, #27948, #37294, #31005, #12509, #24902, #37497, #9070, #6010, #9673, #9469, #19005, #30610, #12117, #8870, #18417, #31198, #5818, #6212, #30807, #6405, #21848, #31396, #39740, #2972, #323, #18813, #9267 ),
 ( #3364, #21260, #33668, #24307, #15756, #28146, #12702, #22049, #3172, #21454, #34450, #36706, #27352, #11918, #18220, #33862, #2770, #15163, #24502, #15360, #40138, #12313, #37099, #21650, #34054, #32563, #16158, #4721, #20372, #25299, #28543, #4923, #14058, #11222 ),
 ( #7763, #13862, #17128, #26451, #29504, #34844, #26251, #6795, #32766, #38647, #34644, #10820, #38850, #37693, #8167, #4521, #19396, #23409, #32359, #9861, #23209, #13094, #17329, #20166, #22438, #22239, #36009, #10059, #19199, #522, #39043, #35804, #718, #31588 ),
 ( #11027, #35606, #1679, #7959, #3756, #25485, #29704, #1885, #37885, #14265, #6995, #16920, #23612, #26653, #20573, #3562, #29304, #15960, #1475, #28340, #12903, #2482, #12017, #5123, #2083, #5513, #27452, #14669, #32968, #5320, #36603, #24405, #14870, #33567 ),
 ( #17530, #27654, #14461, #12217, #36404, #18318, #2280, #27060, #29903, #26855, #8974, #39445, #33168, #36800, #24008, #24609, #8566, #39245, #30107, #8770, #21363, #9171, #20965, #17731, #11625, #30312, #5717, #33770, #11425, #23809, #36211, #15062, #39838, #8374 ),
 ( #5917, #30711, #30516, #15265, #21160, #33370, #2876, #20774, #17927, #27256, #40038, #18126, #39642, #11817, #24204, #2675, #37003, #9775, #37795, #3075, #6312, #22348, #31505, #28651, #12413, #19113, #6508, #28257, #12618, #627, #28052, #31305, #21558, #30908 ),
 ( #24805, #3473, #16064, #15464, #25599, #21957, #37399, #13009, #9577, #27855, #15868, #31108, #9969, #37606, #231, #28, #13204, #25006, #37204, #18519, #16267, #25398, #18720, #9375, #34754, #25208, #3671, #431, #28452, #12814, #21752, #34160, #22152, #6904 ),
 ( #31702, #19309, #3869, #825, #37998, #6705, #34554, #33956, #3273, #15665, #34360, #6113, #18914, #35557, #22954, #35152, #26204, #29453, #1029, #35357, #32522, #13811, #19711, #1633, #4474, #19507, #10173, #4870, #31899, #29657, #13611, #35761, #32104, #4268 ),
 ( #25805, #7307, #4064, #1232, #26404, #13410, #1429, #26000, #14015, #4674, #26607, #34959, #38397, #7917, #38803, #16878, #19916, #10572, #7109, #10371, #17285, #23158, #16469, #7512, #29258, #38598, #22748, #10772, #10978, #28852, #16673, #23366, #20121, #1840 ),
 ( #7719, #32314, #17079, #20322, #32719, #14217, #22549, #38200, #29055, #20918, #29855, #8523, #33526, #20524, #2830, #39396, #14624, #18080, #27013, #5078, #33324, #8330, #27408, #14825, #17686, #17484, #30668, #5274, #2039, #35961, #33726, #30470, #36159, #26811 ),
 ( #21118, #5471, #36556, #17884, #32920, #39200, #30266, #39796, #20730, #8726, #30062, #33121, #5873, #2434, #5668, #21320, #2236, #15221, #11577, #39600, #23965, #27211, #2630, #11175, #8117, #36360, #15018, #11774, #39001, #11379, #24159, #11972, #24363, #36760 ),
 ( #23567, #18276, #14417, #23762, #8929, #12961, #37155, #9329, #39993, #36960, #3622, #21710, #27812, #6657, #18671, #19255, #31064, #12171, #24756, #31259, #16017, #3820, #3228, #40196, #12368, #24959, #384, #19065, #21512, #33915, #9125, #9727, #22108, #25158 ),
 ( #27608, #12764, #28204, #15418, #34113, #37752, #21904, #31455, #179, #24566, #15818, #3027, #580, #37354, #28403, #9529, #6269, #9922, #30865, #22303, #34702, #6855, #15619, #3421, #25351, #6070, #28005, #31654, #37556, #18474, #12568, #34310, #6463, #34508 ),
 ( #18868, #20272, #19657, #16828, #13361, #25949, #35509, #28602, #25549, #29004, #10723, #38146, #16220, #28804, #19871, #7671, #38348, #29209, #1380, #38551, #32260, #13762, #26154, #38753, #10319, #7257, #10934, #23110, #7867, #31852, #25750, #10121, #32052, #32470 ),
 ( #4221, #774, #22700, #4423, #4627, #32673, #16625, #980, #16416, #13562, #20074, #17028, #22497, #34906, #37949, #29408, #1584, #13968, #23320, #26360, #35103, #35714, #7059, #13156, #1179, #19456, #4014, #10518, #22902, #35304, #7462, #17437, #33280, #21073 ),
 ( #5622, #14778, #11926, #35911, #2388, #30013, #11530, #36115, #24114, #11332, #14576, #4827, #14168, #8275, #27166, #5431, #18031, #39748, #26760, #39149, #2588, #30425, #23716, #26965, #39552, #17839, #11728, #30217, #20682, #39354, #8071, #33479, #23916, #20478 ),
 ( #24317, #33078, #5228, #14971, #27361, #17642, #36316, #36510, #2189, #36714, #8478, #8681, #20878, #29609, #8878, #32873, #21267, #17233, #1786, #26566, #5027, #38955, #29811, #11128, #23514, #1994, #14373, #37303, #6605, #9867, #24708, #12711, #18821, #3572 ),
 ( #22059, #15764, #31206, #128, #3372, #39946, #12124, #21463, #25306, #15967, #28155, #6220, #18424, #9477, #25107, #24510, #18625, #331, #21857, #2980, #37505, #27955, #2778, #33676, #28348, #15170, #12912, #37108, #19013, #15369, #27759, #5828, #27561, #9681 ),
 ( #9275, #34457, #36909, #24909, #21658, #31403, #529, #18227, #30619, #34062, #37702, #9078, #12519, #3179, #31014, #12321, #15569, #33868, #40146, #6019, #34262, #30816, #6415, #38705, #7411, #22851, #10069, #35053, #22247, #19820, #28951, #37895, #35461, #927 ),
 ( #10468, #38499, #3766, #7005, #23058, #32208, #29355, #13106, #4370, #7207, #19405, #25899, #7616, #34652, #13305, #1329, #16776, #32418, #13710, #4576, #10675, #29159, #26101, #1130, #20022, #28554, #727, #22448, #13918, #16977, #1532, #19609, #31801, #38298 ),
 ( #6803, #34856, #35254, #26312, #32002, #19208, #31596, #16168, #25495, #3965, #16366, #28752, #25700, #38093, #10267, #22647, #4168, #16572, #13510, #4777, #1945, #27115, #1739, #2138, #14321, #2340, #5376, #27313, #35663, #39099, #36461, #14726, #5179, #20630 ),
 ( #17185, #29560, #20223, #33230, #17792, #8432, #33432, #14521, #32824, #21022, #32622, #7820, #11084, #5572, #23866, #14118, #8224, #17591, #39302, #23466, #11479, #39503, #26518, #35858, #11679, #20829, #17981, #38906, #30167, #36063, #29959, #26714, #24068, #17391 ),
 ( #8020, #8629, #33031, #20427, #26914, #30372, #4979, #14925, #11283, #23667, #2537, #36269, #29765, #10883, #23268, #28103, #15524, #18374, #18178, #31352, #5969, #2730, #36661, #34408, #31160, #36858, #27510, #12666, #3127, #21807, #9224, #37254, #39895, #34015 ),
 ( #24858, #9629, #3325, #22010, #281, #34209, #9428, #6172, #6364, #5777, #30572, #12071, #3521, #6559, #18770, #12273, #24460, #27907, #15714, #15121, #24660, #25059, #82, #9028, #37453, #18573, #8831, #39702, #18965, #21216, #15918, #2929, #11875, #21414 ),
 ( #33627, #24266, #33821, #30768, #15318, #27703, #40097, #37056, #21609, #30959, #12466, #4322, #4527, #31755, #674, #28501, #25650, #1083, #7360, #22199, #34602, #37652, #10421, #22804, #25851, #10624, #31949, #10018, #38452, #9821, #25256, #13054, #23007, #13458 ),
 ( #35010, #16521, #25443, #28905, #16725, #6754, #37843, #29109, #38252, #35410, #19158, #35201, #13258, #7161, #19358, #19766, #34800, #38046, #28302, #31550, #3917, #32161, #1281, #13663, #7568, #22397, #6949, #26053, #19971, #16316, #10215, #32371, #28701, #479 ),
 ( #878, #3714, #12863, #22602, #16117, #19559, #4116, #8385, #14066, #4730, #30118, #20582, #39253, #26664, #14473, #39054, #10829, #17742, #26864, #24017, #7773, #11434, #1896, #23621, #7969, #36220, #23420, #11231, #16929, #26261, #20381, #23817, #17539, #2290 ),
 ( #20975, #17338, #32775, #20782, #4934, #23218, #36018, #26461, #5329, #32978, #35812, #35616, #8576, #29713, #20175, #13871, #11636, #33179, #38860, #17136, #14679, #5133, #27068, #8177, #39453, #29913, #32572, #29514, #2093, #36413, #11036, #33381, #14273, #29313 ),
 ( #1483, #38656, #1689, #31462, #11826, #24215, #33575, #37959, #16228, #3628, #18875, #30524, #22116, #25358, #36612, #31266, #28410, #9733, #15627, #37760, #390, #14880, #5524, #782, #27266, #25558, #9535, #31663, #28012, #185, #17937, #39653, #22312, #12574 ),
 ( #34712, #8781, #37563, #21912, #9930, #586, #22505, #30320, #34316, #3829, #6863, #12770, #15824, #37360, #24966, #3428, #13165, #6470, #28612, #34514, #2490, #28211, #21172, #16023, #6664, #5725, #25165, #18135, #12968, #19072, #3234, #19263, #10130, #31860 ),
 ( #10942, #16424, #19667, #28814, #25957, #23328, #25759, #26165, #38357, #26368, #29417, #11138, #19465, #22911, #20281, #38761, #29218, #4433, #10529, #13570, #32268, #29617, #29014, #4835, #23118, #7067, #16837, #34915, #20083, #35517, #22708, #7472, #4023, #32480 ),
 ( #7876, #35313, #989, #35724, #1388, #38155, #16633, #4635, #10328, #13772, #32681, #17245, #38559, #10733, #7680, #17037, #1594, #19879, #13977, #35113, #1794, #14177, #7265, #26574, #38964, #13371, #32061, #4231, #1189, #2596, #39362, #29819, #5440, #33086 ),
 ( #27370, #36324, #8079, #11738, #39159, #36724, #33289, #39758, #20887, #11341, #5837, #26769, #18237, #30631, #2789, #8285, #27175, #8888, #39957, #14585, #14983, #8690, #33688, #11936, #15180, #24326, #5630, #21081, #30228, #33490, #2004, #14382, #23725, #27570 ),
 ( #35920, #32883, #8488, #18040, #5239, #23524, #36123, #39562, #21276, #17848, #24123, #36519, #30434, #20488, #5035, #17446, #20691, #17651, #26976, #30023, #2199, #11538, #23927, #2397, #14786, #140, #37714, #3581, #6425, #21866, #3189, #31023, #9489, #6815 ),
 ( #34468, #9691, #34663, #15775, #34071, #22259, #33878, #9088, #12330, #19219, #25117, #18434, #34271, #18830, #341, #24718, #12725, #28360, #6030, #37118, #12922, #22068, #31608, #2992, #6616, #37314, #31218, #15580, #31415, #18634, #3382, #12133, #21473, #27966 ),
 ( #25315, #3778, #6232, #12529, #9878, #16179, #24920, #28165, #19023, #37514, #28564, #15979, #538, #24520, #36920, #30825, #27768, #15379, #40157, #9285, #21670, #28763, #23276, #3977, #35674, #7828, #20236, #25712, #4381, #13927, #17194, #32012, #20032, #26112 ),
 ( #38106, #32633, #19829, #35471, #4787, #7218, #739, #4178, #1338, #10277, #10480, #32428, #13117, #10079, #13521, #7626, #22658, #25506, #13316, #16785, #4587, #22861, #13722, #38509, #23067, #29171, #10684, #16988, #37907, #35063, #16581, #22462, #29366, #34867 ),
 ( #19618, #938, #1543, #28964, #7016, #1140, #19417, #25909, #26321, #38308, #38715, #10893, #31811, #16377, #35265, #7419, #32218, #30381, #8234, #11490, #39511, #36072, #39710, #23875, #33440, #2148, #14128, #17801, #4989, #2546, #39310, #5580, #26925, #17400 ) ),
 .UNSPECIFIED., .F., .F., .F.,
 ( 4, 3, 3, 3, 3, 3, 3, 3, 3, 3, 3, 3, 3, 3, 3, 3, 3, 3, 3, 3, 3, 3, 3, 3, 3, 3, 3, 3, 3, 3, 3, 3, 3, 3, 3, 3, 3, 3, 3, 3, 3, 3, 3, 3, 3, 3, 3, 3, 3, 3, 3, 4 ),
 ( 4, 3, 3, 3, 3, 3, 3, 3, 3, 3, 3, 4 ),
 ( 0.5000000000000000000, 0.5156250000000000000, 0.5312500000000000000, 0.5468750000000000000, 0.5625000000000000000, 0.5781250000000000000, 0.5937500000000000000, 0.6093750000000000000, 0.6250000000000000000, 0.6406250000000000000, 0.6562500000000000000, 0.6640625000000000000, 0.6660156250000000000, 0.6665039062500000000, 0.6667480468750000000, 0.6669921875000000000, 0.6679687500000000000, 0.6718750000000000000, 0.6875000000000000000, 0.7031250000000000000, 0.7187500000000000000, 0.7343750000000000000, 0.7500000000000000000, 0.7656250000000000000, 0.7812500000000000000, 0.7968750000000000000, 0.8046875000000000000, 0.8085937500000000000, 0.8088378906250000000, 0.8090820312500000000, 0.8095703125000000000, 0.8105468750000000000, 0.8125000000000000000, 0.8281250000000000000, 0.8437500000000000000, 0.8593750000000000000, 0.8750000000000000000, 0.8906250000000000000, 0.9062500000000000000, 0.9218750000000000000, 0.9375000000000000000, 0.9531250000000000000, 0.9687500000000000000, 0.9843750000000000000, 0.9921875000000000000, 0.9960937500000000000, 0.9980468750000000000, 0.9990234375000000000, 0.9995117187500000000, 0.9997558593750000000, 0.9998779296875000000, 1.000000000000000000 ),
 ( 0.000000000000000000, 0.06250000000000011102, 0.1250000000000002220, 0.1875000000000003331, 0.2500000000000004441, 0.3750000000000006661, 0.5000000000000008882, 0.6250000000000011102, 0.7500000000000013323, 0.8750000000000015543, 0.9375000000000016653, 1.000000000000001776 ),
 .UNSPECIFIED. ) ;
#15516 = FACE_BOUND ( 'NONE', #18899, .T. ) ;
#15517 = FACE_OUTER_BOUND ( 'NONE', #22777, .T. ) ;
#15518 = CARTESIAN_POINT ( 'NONE',  ( -20.63291709985350053, 6.542238888207103642, -22.14536008743868933 ) ) ;
#15519 = LINE ( 'NONE', #24656, #36531 ) ;
#15520 = CARTESIAN_POINT ( 'NONE',  ( -0.7609933293816388833, 37.44611345180490503, 10.49999999999999467 ) ) ;
#15521 = CARTESIAN_POINT ( 'NONE',  ( 13.74558791142738912, -15.22183123319548770, -29.25951782139146928 ) ) ;
#15522 = DIRECTION ( 'NONE',  ( -1.000000000000000000, 0.000000000000000000, 0.000000000000000000 ) ) ;
#15523 = ADVANCED_FACE ( 'NONE', ( #16380 ), #8205, .T. ) ;
#15524 = CARTESIAN_POINT ( 'NONE',  ( 13.63088033700408452, 23.70229946530109899, -14.44436252122576114 ) ) ;
#15525 = EDGE_LOOP ( 'NONE', ( #22024, #19479, #23796, #29839 ) ) ;
#15526 = CARTESIAN_POINT ( 'NONE',  ( -15.81766387322535294, 24.25203275818095960, -8.314427518714673226 ) ) ;
#15527 = CARTESIAN_POINT ( 'NONE',  ( -22.68370119258293016, -18.87043823706580525, 20.69868183039781329 ) ) ;
#15528 = DIRECTION ( 'NONE',  ( 1.000000000000000000, 0.000000000000000000, 0.000000000000000000 ) ) ;
#15529 = CARTESIAN_POINT ( 'NONE',  ( 15.39433494388958046, 26.59358880772150258, -6.417088570401624281 ) ) ;
#15530 = ORIENTED_EDGE ( 'NONE', *, *, #38456, .F. ) ;
#15531 = CARTESIAN_POINT ( 'NONE',  ( 14.52509594610761923, 21.97885917798724975, 7.500000000000010658 ) ) ;
#15532 = ORIENTED_EDGE ( 'NONE', *, *, #17867, .F. ) ;
#15534 = DIRECTION ( 'NONE',  ( 0.000000000000000000, 0.000000000000000000, 1.000000000000000000 ) ) ;
#15533 = CARTESIAN_POINT ( 'NONE',  ( -14.42407661054300583, 25.27392573504564410, -11.57633654154478720 ) ) ;
#15535 = CARTESIAN_POINT ( 'NONE',  ( -9.875123302056525887, -18.52367353807504102, -26.21621392048563948 ) ) ;
#15536 = CARTESIAN_POINT ( 'NONE',  ( -13.64211604268330724, 20.79918788657763429, 13.00000000000000178 ) ) ;
#15537 = EDGE_LOOP ( 'NONE', ( #6291, #17223, #2846, #33719 ) ) ;
#15538 = CARTESIAN_POINT ( 'NONE',  ( -34.49769457167991504, -16.76017602247890892, -5.856898327356995893 ) ) ;
#15539 = CARTESIAN_POINT ( 'NONE',  ( -8.962781483812664263, -18.91548421640152711, -26.29799973468894692 ) ) ;
#15540 = CARTESIAN_POINT ( 'NONE',  ( 4.003793317224326742, 8.420815634768674229, 11.00000000000000000 ) ) ;
#15541 = CARTESIAN_POINT ( 'NONE',  ( 15.31670069829342573, 22.92704149593691554, -11.66084285614651250 ) ) ;
#15542 = ORIENTED_EDGE ( 'NONE', *, *, #8661, .T. ) ;
#15543 = CARTESIAN_POINT ( 'NONE',  ( 19.75709278228214316, 5.918078465942131494, -27.67886744341916128 ) ) ;
#15544 = CARTESIAN_POINT ( 'NONE',  ( -6.688306800005769048, 28.52217545723006609, 12.00000000000000000 ) ) ;
#15545 = CARTESIAN_POINT ( 'NONE',  ( 7.143250075007565592, 35.69054364144594871, 7.202682876670055023 ) ) ;
#15546 = CARTESIAN_POINT ( 'NONE',  ( -16.05099854214882171, -21.51520587156189279, -17.05908743440501851 ) ) ;
#15547 = ORIENTED_EDGE ( 'NONE', *, *, #9315, .T. ) ;
#15548 = CARTESIAN_POINT ( 'NONE',  ( -30.53615654196750739, -0.3717794457668220920, -8.746079897285124360 ) ) ;
#15549 = CARTESIAN_POINT ( 'NONE',  ( 30.58646958062722732, -0.2537825805908827115, -8.284971368571740769 ) ) ;
#15550 = CARTESIAN_POINT ( 'NONE',  ( -5.599788042746297378, 36.30662653786500016, 10.82238861112318418 ) ) ;
#15551 = CARTESIAN_POINT ( 'NONE',  ( 28.60147806546228821, -12.08038679647185454, 20.50957957746028626 ) ) ;
#15552 = ORIENTED_EDGE ( 'NONE', *, *, #36674, .T. ) ;
#15553 = EDGE_CURVE ( 'NONE', #27538, #36749, #28766, .T. ) ;
#15554 = CARTESIAN_POINT ( 'NONE',  ( 19.69645987729881043, 11.37175641224107814, -21.56489709563629376 ) ) ;
#15555 = DIRECTION ( 'NONE',  ( -0.000000000000000000, -0.000000000000000000, -1.000000000000000000 ) ) ;
#15556 = VERTEX_POINT ( 'NONE', #4384 ) ;
#15557 = CARTESIAN_POINT ( 'NONE',  ( 6.282361020112160688, 14.70372268239673197, 10.00000000000000000 ) ) ;
#15558 = CIRCLE ( 'NONE', #25934, 0.5000000000000001110 ) ;
#15559 = CARTESIAN_POINT ( 'NONE',  ( -30.33922525723529873, 6.243664897713534501, 23.00000000001065814 ) ) ;
#15560 = DIRECTION ( 'NONE',  ( 0.5877852522924691403, -0.8090169943749503378, 6.938893903907234689E-15 ) ) ;
#15561 = CARTESIAN_POINT ( 'NONE',  ( 2.710501123038885130, 37.71647222079759132, -7.547886179347838009 ) ) ;
#15562 = DIRECTION ( 'NONE',  ( 1.000000000000000000, 0.000000000000000000, 0.000000000000000000 ) ) ;
#15563 = CARTESIAN_POINT ( 'NONE',  ( -14.36830325120615548, 20.48707633493503621, 7.000000000000000000 ) ) ;
#15564 = CARTESIAN_POINT ( 'NONE',  ( -12.03641663870442713, 15.85735326529964873, 12.00000000000000000 ) ) ;
#15565 = AXIS2_PLACEMENT_3D ( 'NONE', #18859, #12754, #19054 ) ;
#15566 = FACE_OUTER_BOUND ( 'NONE', #36346, .T. ) ;
#15567 = CARTESIAN_POINT ( 'NONE',  ( 4.475131784526629630, 8.183115020678576101, 7.000000000000000000 ) ) ;
#15568 = ADVANCED_FACE ( 'NONE', ( #13320 ), #10350, .T. ) ;
#15569 = CARTESIAN_POINT ( 'NONE',  ( 13.39086794456952489, 24.19890610734487879, -14.39401347409533471 ) ) ;
#15570 = LINE ( 'NONE', #16367, #32093 ) ;
#15571 = VERTEX_POINT ( 'NONE', #13725 ) ;
#15573 = CARTESIAN_POINT ( 'NONE',  ( -14.98890122036483419, -28.67928442680469203, -4.999999999999999112 ) ) ;
#15572 = CARTESIAN_POINT ( 'NONE',  ( -14.97876122052304027, 14.11420655003455593, -28.25524194599643835 ) ) ;
#15574 = CARTESIAN_POINT ( 'NONE',  ( 13.05736835487433467, 16.11602540378438775, 10.49999999999999822 ) ) ;
#15575 = EDGE_CURVE ( 'NONE', #33995, #34769, #27905, .T. ) ;
#15576 = CARTESIAN_POINT ( 'NONE',  ( 15.46723536449282044, -26.71148257425455697, -5.946079193718386335 ) ) ;
#15577 = CARTESIAN_POINT ( 'NONE',  ( -22.79932625038946981, -26.94340799757786442, -4.999999999999999112 ) ) ;
#15578 = CARTESIAN_POINT ( 'NONE',  ( -4.724378136954611840, 12.76962061027129458, 13.00000000000000178 ) ) ;
#15579 = B_SPLINE_CURVE_WITH_KNOTS ( 'NONE', 3,
 ( #22750, #29660, #35763, #29057, #20124, #29456 ),
 .UNSPECIFIED., .F., .F.,
 ( 4, 2, 4 ),
 ( 0.000000000000000000, 0.5000000000000000000, 1.000000000000000000 ),
 .UNSPECIFIED. ) ;
#15580 = CARTESIAN_POINT ( 'NONE',  ( 11.17038230804670107, 17.76644183184714265, -26.22336807236404610 ) ) ;
#15581 = ORIENTED_EDGE ( 'NONE', *, *, #7795, .T. ) ;
#15582 = CARTESIAN_POINT ( 'NONE',  ( -33.75875814100324845, 2.759858869446484064, 11.00000000000000000 ) ) ;
#15583 = CARTESIAN_POINT ( 'NONE',  ( -14.50510232685715906, -25.43776907747248472, -10.65577769986489542 ) ) ;
#15584 = CARTESIAN_POINT ( 'NONE',  ( -17.04089262280391281, -28.02826808823053284, 15.13084544680188870 ) ) ;
#15585 = EDGE_CURVE ( 'NONE', #445, #22181, #1143, .T. ) ;
#15586 = CARTESIAN_POINT ( 'NONE',  ( -29.94129476457376882, -22.05385023193113980, -8.415718586356796038 ) ) ;
#15587 = CARTESIAN_POINT ( 'NONE',  ( 1.397217954152080166, -21.66464354399617775, -21.18345308184954590 ) ) ;
#15588 = CARTESIAN_POINT ( 'NONE',  ( 15.27813064198010196, 25.57022799658983558, -8.773304169343077774 ) ) ;
#15589 = CARTESIAN_POINT ( 'NONE',  ( 20.28966096934918184, 10.25376961063980907, -16.97639449884776752 ) ) ;
#15590 = CARTESIAN_POINT ( 'NONE',  ( 11.61633080063109702, 31.93537370176170853, 10.49999999999999822 ) ) ;
#15591 = CARTESIAN_POINT ( 'NONE',  ( -4.056756644314476468, 28.55033231052837550, -16.67183270246686178 ) ) ;
#15592 = ORIENTED_EDGE ( 'NONE', *, *, #23908, .F. ) ;
#15593 = CARTESIAN_POINT ( 'NONE',  ( -32.81213598086766581, -5.178738028136198324, -9.908093442003993445 ) ) ;
#15594 = CARTESIAN_POINT ( 'NONE',  ( -19.49168883800204455, 11.25353179757921751, 18.42518152272108978 ) ) ;
#15595 = ORIENTED_EDGE ( 'NONE', *, *, #19413, .T. ) ;
#15596 = FACE_OUTER_BOUND ( 'NONE', #22125, .T. ) ;
#15597 = DIRECTION ( 'NONE',  ( 1.000000000000000000, 0.000000000000000000, 0.000000000000000000 ) ) ;
#15598 = ADVANCED_FACE ( 'NONE', ( #24079 ), #15332, .T. ) ;
#15599 = AXIS2_PLACEMENT_3D ( 'NONE', #20213, #23656, #33218 ) ;
#15600 = CARTESIAN_POINT ( 'NONE',  ( -20.91237790324122159, 1.319957874075606385, -26.26824219631393476 ) ) ;
#15601 = EDGE_CURVE ( 'NONE', #30975, #8691, #33042, .T. ) ;
#15602 = CARTESIAN_POINT ( 'NONE',  ( 27.77279998450218912, -11.16583192376935862, -15.71995317866785946 ) ) ;
#15603 = EDGE_CURVE ( 'NONE', #20131, #17593, #27655, .T. ) ;
#15604 = EDGE_LOOP ( 'NONE', ( #4207, #23789 ) ) ;
#15605 = CARTESIAN_POINT ( 'NONE',  ( 19.48557158514982746, -11.25000000000009415, -0.000000000000000000 ) ) ;
#15606 = ORIENTED_EDGE ( 'NONE', *, *, #9109, .T. ) ;
#15607 = CARTESIAN_POINT ( 'NONE',  ( -11.77091082532341204, 29.60251629318183575, 12.00000000000000000 ) ) ;
#15608 = CARTESIAN_POINT ( 'NONE',  ( -19.48557158514998022, -11.24999999999982414, 3.000000000000000000 ) ) ;
#15609 = FACE_OUTER_BOUND ( 'NONE', #24468, .T. ) ;
#15610 = VERTEX_POINT ( 'NONE', #17996 ) ;
#15611 = CARTESIAN_POINT ( 'NONE',  ( -2.700909190172711138, 24.47130327029587349, -20.72671218256706993 ) ) ;
#15612 = AXIS2_PLACEMENT_3D ( 'NONE', #36708, #24309, #17432 ) ;
#15613 = CARTESIAN_POINT ( 'NONE',  ( 8.221629120123230550, 5.055853521246038262, 10.00000000000000000 ) ) ;
#15614 = PLANE ( 'NONE',  #10505 ) ;
#15615 = CARTESIAN_POINT ( 'NONE',  ( 14.09933648065468503, 26.02968990214155198, 11.00000000000000000 ) ) ;
#15616 =( BOUNDED_SURFACE ( )  B_SPLINE_SURFACE ( 2, 3, ( 
 ( #9068, #37292, #3170, #28144, #9467, #321 ),
 ( #120, #15559, #24699, #27946, #18022, #37096 ),
 ( #15358, #39934, #37495, #12311, #27750, #24900 ) ),
 .UNSPECIFIED., .F., .F., .F. ) 
 B_SPLINE_SURFACE_WITH_KNOTS ( ( 3, 3 ),
 ( 4, 2, 4 ),
 ( 0.000000000000000000, 1.000000000000000000 ),
 ( 5.507097317918141499, 5.759586531581287971, 6.012075745244433556 ),
 .UNSPECIFIED. ) 
 GEOMETRIC_REPRESENTATION_ITEM ( )  RATIONAL_B_SPLINE_SURFACE ( (
 ( 1.000000000000000000, 1.000000000000000000, 1.000000000000000000, 1.000000000000000000, 1.000000000000000000, 1.000000000000000000),
 ( 0.7071067811865474617, 0.7071067811865474617, 0.7071067811865474617, 0.7071067811865474617, 0.7071067811865474617, 0.7071067811865474617),
 ( 1.000000000000000000, 1.000000000000000000, 1.000000000000000000, 1.000000000000000000, 1.000000000000000000, 1.000000000000000000) ) ) 
 REPRESENTATION_ITEM ( '' )  SURFACE ( )  );
#15617 = EDGE_CURVE ( 'NONE', #12299, #23375, #39112, .T. ) ;
#15618 = DIRECTION ( 'NONE',  ( 0.000000000000000000, 0.000000000000000000, 1.000000000000000000 ) ) ;
#15619 = CARTESIAN_POINT ( 'NONE',  ( 10.08828624387746586, 22.01629898975007293, -20.18907799365789302 ) ) ;
#15620 = VERTEX_POINT ( 'NONE', #11693 ) ;
#15621 = CARTESIAN_POINT ( 'NONE',  ( -17.74591135789209773, 10.55662882352565646, -27.17856662802773116 ) ) ;
#15622 = CARTESIAN_POINT ( 'NONE',  ( 18.68934290552659760, 29.94321432092586122, 23.00000000000375522 ) ) ;
#15623 = ADVANCED_FACE ( 'NONE', ( #35874 ), #1959, .F. ) ;
#15624 = CARTESIAN_POINT ( 'NONE',  ( 9.670856713498491075, -18.12756278475329808, -28.70101805749319723 ) ) ;
#15625 = CARTESIAN_POINT ( 'NONE',  ( 9.343266739736584725, 17.68301270189219210, 10.00000000000000000 ) ) ;
#15626 = CONICAL_SURFACE ( 'NONE', #20826, 0.9999999999999981126, 0.7853981633974562726 ) ;
#15627 = CARTESIAN_POINT ( 'NONE',  ( 13.17275120719023107, 22.30352509093737012, -16.43557425179639964 ) ) ;
#15628 = CARTESIAN_POINT ( 'NONE',  ( 2.168404344971008868E-14, -26.63027081345975589, -4.999999999999999112 ) ) ;
#15629 = CARTESIAN_POINT ( 'NONE',  ( -3.000488737322915878, 30.46850471150003159, 9.000000000000001776 ) ) ;
#15630 = CARTESIAN_POINT ( 'NONE',  ( -13.74893865958837580, 23.44248173773514310, -14.47139730366743571 ) ) ;
#15631 = CARTESIAN_POINT ( 'NONE',  ( -21.46071079579204977, -24.07222328743980455, -12.13688642999643896 ) ) ;
#15632 = CARTESIAN_POINT ( 'NONE',  ( 8.971832194761836021, -22.56238950268238952, -16.70641590008881039 ) ) ;
#15633 = CARTESIAN_POINT ( 'NONE',  ( 13.54214413866547240, 22.71670133636794731, -15.45773015834430097 ) ) ;
#15634 = CARTESIAN_POINT ( 'NONE',  ( 31.02556648718628196, -22.39342206112319289, -5.000000000000000000 ) ) ;
#15635 = CARTESIAN_POINT ( 'NONE',  ( 5.599788042746504324, 36.30662653786479410, 10.82238861112336537 ) ) ;
#15636 = ORIENTED_EDGE ( 'NONE', *, *, #215, .T. ) ;
#15637 = CARTESIAN_POINT ( 'NONE',  ( -10.30584816049105257, 34.79301137796964127, -5.444905193120368025 ) ) ;
#15638 = DIRECTION ( 'NONE',  ( -0.000000000000000000, -0.000000000000000000, -1.000000000000000000 ) ) ;
#15639 = CARTESIAN_POINT ( 'NONE',  ( -12.97403502154108779, 15.97168783648715618, 10.66666666666666252 ) ) ;
#15640 = TOROIDAL_SURFACE ( 'NONE', #730, 16.00000000000000000, 1.000000000000000000 ) ;
#15641 = CARTESIAN_POINT ( 'NONE',  ( 18.00000000000000000, 22.50000000000001421, 3.000000000000000000 ) ) ;
#15642 = ORIENTED_EDGE ( 'NONE', *, *, #29902, .F. ) ;
#15643 = CARTESIAN_POINT ( 'NONE',  ( 20.60885639961789906, 0.8764464790524432170, -28.07880677701691141 ) ) ;
#15644 = VECTOR ( 'NONE', #16916, 1000.000000000000000 ) ;
#15645 = CARTESIAN_POINT ( 'NONE',  ( 14.44277748876681855, 26.55045409923015853, 7.500000000000000888 ) ) ;
#15646 = DIRECTION ( 'NONE',  ( -1.000000000000000000, 0.000000000000000000, 0.000000000000000000 ) ) ;
#15647 = ORIENTED_EDGE ( 'NONE', *, *, #30723, .F. ) ;
#15648 = CARTESIAN_POINT ( 'NONE',  ( -21.27250862215679206, 0.8036217730998547193, -25.01755668826255175 ) ) ;
#15649 = CYLINDRICAL_SURFACE ( 'NONE', #24173, 1.000000000000000000 ) ;
#15650 = ORIENTED_EDGE ( 'NONE', *, *, #28985, .F. ) ;
#15651 = CARTESIAN_POINT ( 'NONE',  ( 29.00584441142848746, -5.994069036618491886, -14.94548092090875535 ) ) ;
#15652 = VERTEX_POINT ( 'NONE', #14738 ) ;
#15653 = CARTESIAN_POINT ( 'NONE',  ( 16.63496159151925369, 29.12310921430783850, 12.73282698324831941 ) ) ;
#15654 = B_SPLINE_CURVE_WITH_KNOTS ( 'NONE', 3,
 ( #16822, #1375, #23710, #21262, #38951, #17832, #27355, #36310, #11722, #27160, #2582, #39742, #33473, #33670, #14369, #30210, #23508, #26959 ),
 .UNSPECIFIED., .F., .F.,
 ( 4, 2, 2, 2, 2, 2, 2, 2, 4 ),
 ( 0.000000000000000000, 0.1249999999999999722, 0.2499999999999999445, 0.3749999999999998890, 0.4999999999999998890, 0.6249999999999998890, 0.7499999999999997780, 0.8749999999999997780, 1.000000000000000000 ),
 .UNSPECIFIED. ) ;
#15655 = VECTOR ( 'NONE', #34307, 1000.000000000000000 ) ;
#15656 = CARTESIAN_POINT ( 'NONE',  ( -8.137585970691985082, 29.15429895402941440, 10.50000000000000000 ) ) ;
#15657 = CARTESIAN_POINT ( 'NONE',  ( 6.811226782241714517, 35.33967249274190436, 10.49999999999999822 ) ) ;
#15658 = CARTESIAN_POINT ( 'NONE',  ( -9.267781094590318958, 26.19038745656696676, 20.25080042701543448 ) ) ;
#15659 = LINE ( 'NONE', #28045, #2565 ) ;
#15660 = EDGE_LOOP ( 'NONE', ( #38318, #12331 ) ) ;
#15661 = CARTESIAN_POINT ( 'NONE',  ( 3.781037291632489250, 7.996959361763587459, 10.49999999999999822 ) ) ;
#15662 = DIRECTION ( 'NONE',  ( 1.000000000000000000, 0.000000000000000000, 0.000000000000000000 ) ) ;
#15663 = CARTESIAN_POINT ( 'NONE',  ( 12.59251905104225600, 14.34933092922137021, 7.455539900862797609 ) ) ;
#15664 = DIRECTION ( 'NONE',  ( 0.000000000000000000, 0.000000000000000000, 1.000000000000000000 ) ) ;
#15665 = CARTESIAN_POINT ( 'NONE',  ( 9.732527571296289537, 33.77328167068598219, -8.933206717022359911 ) ) ;
#15666 = CIRCLE ( 'NONE', #13713, 1.000000000000000000 ) ;
#15667 = AXIS2_PLACEMENT_3D ( 'NONE', #1419, #35752, #17067 ) ;
#15668 = CARTESIAN_POINT ( 'NONE',  ( 14.30237662736994508, -22.54417004151479631, -16.27104889190381698 ) ) ;
#15669 = LINE ( 'NONE', #31112, #14550 ) ;
#15670 = CARTESIAN_POINT ( 'NONE',  ( -12.31033848243476214, 14.30014505118406021, 10.49999999999999822 ) ) ;
#15671 = ORIENTED_EDGE ( 'NONE', *, *, #20072, .F. ) ;
#15672 = CARTESIAN_POINT ( 'NONE',  ( -11.33053354013682856, 18.02203028756851211, -25.01733111074807070 ) ) ;
#15673 = CARTESIAN_POINT ( 'NONE',  ( -18.97483082528767540, -25.68201547601522350, 17.92354375535288824 ) ) ;
#15674 = CARTESIAN_POINT ( 'NONE',  ( 15.03078399508466134, -26.24871699600646124, -8.298773291112503614 ) ) ;
#15675 = CIRCLE ( 'NONE', #31887, 1.000000000000000000 ) ;
#15676 = FACE_OUTER_BOUND ( 'NONE', #16286, .T. ) ;
#15677 = EDGE_LOOP ( 'NONE', ( #23777, #25902, #4848, #29332 ) ) ;
#15678 = VERTEX_POINT ( 'NONE', #11298 ) ;
#15679 = CARTESIAN_POINT ( 'NONE',  ( -13.86191765000857856, 30.49075772208747992, -4.999999999999998224 ) ) ;
#15680 = CARTESIAN_POINT ( 'NONE',  ( -19.35675346592083557, -25.73740943145480742, -10.41501234748526983 ) ) ;
#15681 = FACE_BOUND ( 'NONE', #14514, .T. ) ;
#15682 = EDGE_LOOP ( 'NONE', ( #14398, #4684, #22520 ) ) ;
#15683 = CARTESIAN_POINT ( 'NONE',  ( -24.16886640984839119, -7.534202883240132209, -19.77792120075160653 ) ) ;
#15684 = CARTESIAN_POINT ( 'NONE',  ( -9.413550212251061922, -18.21086026825004112, -29.35007373650224238 ) ) ;
#15685 = DIRECTION ( 'NONE',  ( -1.000000000000000000, 0.000000000000000000, 0.000000000000000000 ) ) ;
#15686 = VERTEX_POINT ( 'NONE', #26928 ) ;
#15687 = CARTESIAN_POINT ( 'NONE',  ( 20.43785338154470921, 1.730618592969307867, -30.00000000000000355 ) ) ;
#15688 = DIRECTION ( 'NONE',  ( 0.000000000000000000, 0.000000000000000000, 1.000000000000000000 ) ) ;
#15689 = DIRECTION ( 'NONE',  ( -0.7071067811865526798, 0.000000000000000000, -0.7071067811865422437 ) ) ;
#15690 = VERTEX_POINT ( 'NONE', #38918 ) ;
#15691 = CARTESIAN_POINT ( 'NONE',  ( -27.78115282291058818, 0.1336662928856390542, -13.50786979312386471 ) ) ;
#15692 = ORIENTED_EDGE ( 'NONE', *, *, #18359, .T. ) ;
#15693 = CARTESIAN_POINT ( 'NONE',  ( 24.52549093940175950, -1.059282194882694927, -19.29662230946326673 ) ) ;
#15694 = CARTESIAN_POINT ( 'NONE',  ( 17.30788606036681543, -10.99133882972088472, -30.00000000000004263 ) ) ;
#15695 = CARTESIAN_POINT ( 'NONE',  ( 33.85500357264645999, -15.79720895788926427, 17.42190598798393353 ) ) ;
#15696 = ADVANCED_FACE ( 'NONE', ( #8237 ), #30384, .F. ) ;
#15697 = VERTEX_POINT ( 'NONE', #14333 ) ;
#15698 = CARTESIAN_POINT ( 'NONE',  ( -25.59020507252603949, 4.375312855643961107, -11.74991072239141765 ) ) ;
#15699 = CARTESIAN_POINT ( 'NONE',  ( 0.4999999999999990563, 31.00000000000000355, 9.000000000000001776 ) ) ;
#15700 = DIRECTION ( 'NONE',  ( -0.000000000000000000, -0.000000000000000000, 1.000000000000000000 ) ) ;
#15701 = DIRECTION ( 'NONE',  ( -1.000000000000000000, 0.000000000000000000, 0.000000000000000000 ) ) ;
#15702 = EDGE_CURVE ( 'NONE', #29636, #11564, #4961, .T. ) ;
#15703 = AXIS2_PLACEMENT_3D ( 'NONE', #30601, #8860, #36491 ) ;
#15704 = CYLINDRICAL_SURFACE ( 'NONE', #17573, 1.000000000000000000 ) ;
#15705 = EDGE_CURVE ( 'NONE', #31788, #21571, #33536, .T. ) ;
#15706 = AXIS2_PLACEMENT_3D ( 'NONE', #28319, #2948, #9649 ) ;
#15707 = LINE ( 'NONE', #36653, #38516 ) ;
#15708 = CARTESIAN_POINT ( 'NONE',  ( 32.28722999652337933, 1.315479119629257010, 12.14047268033097460 ) ) ;
#15709 = CARTESIAN_POINT ( 'NONE',  ( -24.15419107429150003, 8.025926297992866054, -6.445781696981516262 ) ) ;
#15710 = DIRECTION ( 'NONE',  ( -0.000000000000000000, -0.000000000000000000, 1.000000000000000000 ) ) ;
#15711 = CARTESIAN_POINT ( 'NONE',  ( 2.494936919103933448, 34.23777120880591696, 6.000000000000000000 ) ) ;
#15712 = CARTESIAN_POINT ( 'NONE',  ( 17.38440248539185262, -18.07777754567372952, -19.86656258602833702 ) ) ;
#15713 = CARTESIAN_POINT ( 'NONE',  ( -13.30736791469135483, 15.68301270237671474, 10.49999999999999822 ) ) ;
#15714 = CARTESIAN_POINT ( 'NONE',  ( 13.08626868863102288, 22.46072230355650845, -16.41598118283816277 ) ) ;
#15715 = ORIENTED_EDGE ( 'NONE', *, *, #22187, .F. ) ;
#15716 = CARTESIAN_POINT ( 'NONE',  ( -16.00871871683318659, 23.70244287861901356, -8.319657716573615858 ) ) ;
#15717 = VECTOR ( 'NONE', #36216, 1000.000000000000000 ) ;
#15718 = CARTESIAN_POINT ( 'NONE',  ( -25.98021325959596695, -4.875178728620359614, 20.50957957746029336 ) ) ;
#15719 = EDGE_CURVE ( 'NONE', #30551, #2500, #21161, .T. ) ;
#15720 = EDGE_CURVE ( 'NONE', #10872, #38519, #26350, .T. ) ;
#15721 = DIRECTION ( 'NONE',  ( 1.000000000000000000, 0.000000000000000000, 0.000000000000000000 ) ) ;
#15722 = CARTESIAN_POINT ( 'NONE',  ( 13.78636421790129063, 23.36015420247935737, -14.47817171644321910 ) ) ;
#15723 = ORIENTED_EDGE ( 'NONE', *, *, #13207, .T. ) ;
#15724 = DIRECTION ( 'NONE',  ( 0.000000000000000000, 0.000000000000000000, 1.000000000000000000 ) ) ;
#15725 = ORIENTED_EDGE ( 'NONE', *, *, #18485, .F. ) ;
#15727 = DIRECTION ( 'NONE',  ( 0.2079116908177533474, -0.9781476007338067991, 0.000000000000000000 ) ) ;
#15726 = CARTESIAN_POINT ( 'NONE',  ( -13.36282164858120147, 23.07485381450693751, -15.42106084104891828 ) ) ;
#15728 = CARTESIAN_POINT ( 'NONE',  ( -10.67195756934210316, -19.53628626400035984, -22.71718723575088461 ) ) ;
#15729 = DIRECTION ( 'NONE',  ( 0.000000000000000000, 0.000000000000000000, 1.000000000000000000 ) ) ;
#15730 = ORIENTED_EDGE ( 'NONE', *, *, #34446, .T. ) ;
#15731 = CARTESIAN_POINT ( 'NONE',  ( -33.36273675432661179, -16.18931552824140496, -8.847619819632241089 ) ) ;
#15732 = CARTESIAN_POINT ( 'NONE',  ( -8.865215912320328684, -18.48469441140770542, -29.36070228624526024 ) ) ;
#15733 = DIRECTION ( 'NONE',  ( -0.000000000000000000, -0.000000000000000000, -1.000000000000000000 ) ) ;
#15734 = CARTESIAN_POINT ( 'NONE',  ( 12.94160102779525445, 16.66888978004905653, -25.21160078660660631 ) ) ;
#15735 = ORIENTED_EDGE ( 'NONE', *, *, #6027, .F. ) ;
#15736 = CARTESIAN_POINT ( 'NONE',  ( 23.87359454083856747, 4.573863347061236873, -15.74749371091426653 ) ) ;
#15737 = CYLINDRICAL_SURFACE ( 'NONE', #16729, 59.99999999999997868 ) ;
#15738 = CONICAL_SURFACE ( 'NONE', #2773, 0.4999999999999958922, 0.7853981633974446153 ) ;
#15739 = CARTESIAN_POINT ( 'NONE',  ( 9.331903152615748098, 11.35703883385568602, 9.500000000000000000 ) ) ;
#15740 = DIRECTION ( 'NONE',  ( 0.000000000000000000, 0.000000000000000000, 1.000000000000000000 ) ) ;
#15741 = VERTEX_POINT ( 'NONE', #33443 ) ;
#15742 = CARTESIAN_POINT ( 'NONE',  ( -29.92778146367382774, -0.3254292208867340386, -10.15219817829411397 ) ) ;
#15743 = CARTESIAN_POINT ( 'NONE',  ( 20.53661583307810901, 0.6341784373652767925, -28.69910307870409483 ) ) ;
#15744 = AXIS2_PLACEMENT_3D ( 'NONE', #2898, #6332, #252 ) ;
#15745 = CARTESIAN_POINT ( 'NONE',  ( 27.36681752352244956, -15.80023946406895341, 20.50957957746029336 ) ) ;
#15746 = ORIENTED_EDGE ( 'NONE', *, *, #10777, .F. ) ;
#15747 = B_SPLINE_CURVE_WITH_KNOTS ( 'NONE', 3,
 ( #13065, #29121, #25455, #7174, #31961, #25267, #31767, #4128 ),
 .UNSPECIFIED., .F., .F.,
 ( 4, 2, 2, 4 ),
 ( 0.000000000000000000, 0.0002364868538934306529, 0.0004729737077868613059, 0.0009459474155737255391 ),
 .UNSPECIFIED. ) ;
#15748 = EDGE_CURVE ( 'NONE', #34986, #253, #34791, .T. ) ;
#15749 = CARTESIAN_POINT ( 'NONE',  ( 16.77267017469755217, -29.13948811618736912, -13.79123840944735413 ) ) ;
#15750 = DIRECTION ( 'NONE',  ( -0.000000000000000000, -0.000000000000000000, -1.000000000000000000 ) ) ;
#15751 = VERTEX_POINT ( 'NONE', #17403 ) ;
#15752 = CARTESIAN_POINT ( 'NONE',  ( 5.049784273262975631, -26.77689918168219307, -5.000000000000000000 ) ) ;
#15753 = AXIS2_PLACEMENT_3D ( 'NONE', #30764, #1031, #33622 ) ;
#15754 = CYLINDRICAL_SURFACE ( 'NONE', #26, 6.000000000000005329 ) ;
#15755 = CARTESIAN_POINT ( 'NONE',  ( 3.914034194965609892, 30.06176806842420035, 7.000000000000000000 ) ) ;
#15756 = CARTESIAN_POINT ( 'NONE',  ( 3.853265673577690009, 37.77810895946699077, -6.702677861497350342 ) ) ;
#15757 = CARTESIAN_POINT ( 'NONE',  ( 14.47283171447379146, 21.48159823030312054, 11.00000000000000000 ) ) ;
#15758 = CARTESIAN_POINT ( 'NONE',  ( 0.000000000000000000, 22.50000000000000355, 13.00000000000000178 ) ) ;
#15759 = AXIS2_PLACEMENT_3D ( 'NONE', #34023, #24469, #91 ) ;
#15760 = LINE ( 'NONE', #9676, #31770 ) ;
#15761 = DIRECTION ( 'NONE',  ( 0.000000000000000000, 0.000000000000000000, -1.000000000000000000 ) ) ;
#15762 = DIRECTION ( 'NONE',  ( 0.000000000000000000, 0.000000000000000000, 1.000000000000000000 ) ) ;
#15763 = LINE ( 'NONE', #28154, #17170 ) ;
#15764 = CARTESIAN_POINT ( 'NONE',  ( 15.00330998323748055, 28.06465100738194351, -5.468235726354898851 ) ) ;
#15765 = CARTESIAN_POINT ( 'NONE',  ( 3.503793317224320969, 8.420815634768672453, 11.00000000000000000 ) ) ;
#15766 = VERTEX_POINT ( 'NONE', #20840 ) ;
#15767 = AXIS2_PLACEMENT_3D ( 'NONE', #29763, #13916, #5177 ) ;
#15769 = DIRECTION ( 'NONE',  ( -0.8090169943749504489, -0.5877852522924691403, 0.000000000000000000 ) ) ;
#15768 = CARTESIAN_POINT ( 'NONE',  ( -15.57484573673720796, 13.69435820708697982, -26.56392333108821191 ) ) ;
#15770 = LINE ( 'NONE', #12918, #32847 ) ;
#15771 = CARTESIAN_POINT ( 'NONE',  ( 10.81386370403635944, -19.99604346397223864, -21.62019203441402837 ) ) ;
#15772 = ADVANCED_FACE ( 'NONE', ( #5584 ), #5389, .F. ) ;
#15773 = CARTESIAN_POINT ( 'NONE',  ( -12.94346141028061759, -16.53452242939091121, -26.54686612419656555 ) ) ;
#15774 = CARTESIAN_POINT ( 'NONE',  ( 11.68691289177312420, 18.91070414389390564, -22.73532874761463773 ) ) ;
#15775 = CARTESIAN_POINT ( 'NONE',  ( 15.36131648685467610, 26.71043341655636638, -6.416599091998089754 ) ) ;
#15776 = ORIENTED_EDGE ( 'NONE', *, *, #5213, .T. ) ;
#15777 = CARTESIAN_POINT ( 'NONE',  ( -8.744117900323420400, 12.16605582823075160, 9.500000000000000000 ) ) ;
#15778 = CARTESIAN_POINT ( 'NONE',  ( -10.75859123654805316, -20.00912467510691783, -21.62693100897464404 ) ) ;
#15779 = AXIS2_PLACEMENT_3D ( 'NONE', #4575, #16976, #38092 ) ;
#15780 = CARTESIAN_POINT ( 'NONE',  ( -22.69494504450977956, -28.86495990325026284, 12.73282698324813644 ) ) ;
#15781 = CARTESIAN_POINT ( 'NONE',  ( -30.29849476799594044, -22.30624241272796482, -7.553674803089624135 ) ) ;
#15782 = AXIS2_PLACEMENT_3D ( 'NONE', #6211, #22842, #10257 ) ;
#15783 = CARTESIAN_POINT ( 'NONE',  ( 1.239157320478834423, -20.53705677395570461, -28.86354223400775254 ) ) ;
#15784 = CARTESIAN_POINT ( 'NONE',  ( 11.47031954842671730, 17.36846946539129988, -26.86199371866775820 ) ) ;
#15785 = CARTESIAN_POINT ( 'NONE',  ( 22.17218238145936837, 9.941665176672954018, -10.87683032894513246 ) ) ;
#15786 = CARTESIAN_POINT ( 'NONE',  ( -9.331903152615899089, 11.35703883385581037, 10.50000000000000533 ) ) ;
#15787 = VERTEX_POINT ( 'NONE', #20239 ) ;
#15788 = CARTESIAN_POINT ( 'NONE',  ( -24.90016405581419434, -2.372344258043737497, -19.14849256580092884 ) ) ;
#15789 = CIRCLE ( 'NONE', #35896, 16.00000000000000000 ) ;
#15790 = CARTESIAN_POINT ( 'NONE',  ( -25.97912795568404576, 2.630260520731678930, 17.92354375535789046 ) ) ;
#15791 = EDGE_LOOP ( 'NONE', ( #19191, #33972, #25257, #37985 ) ) ;
#15792 = CARTESIAN_POINT ( 'NONE',  ( -8.917741276437942233, 30.52956727630665057, 13.00000000000000178 ) ) ;
#15793 = AXIS2_PLACEMENT_3D ( 'NONE', #16454, #32506, #1415 ) ;
#15794 = DIRECTION ( 'NONE',  ( 1.000000000000000000, 0.000000000000000000, 0.000000000000000000 ) ) ;
#15795 = CARTESIAN_POINT ( 'NONE',  ( -25.62784820657104135, 0.7174978263156285285, -16.47873148568791635 ) ) ;
#15796 = EDGE_CURVE ( 'NONE', #9989, #24087, #8445, .T. ) ;
#15797 = CARTESIAN_POINT ( 'NONE',  ( 22.15328883633298318, -8.178027178684930121, -21.92584078457036867 ) ) ;
#15798 = CARTESIAN_POINT ( 'NONE',  ( 36.76835206499524844, -7.129807841006594593, 13.32518128616614739 ) ) ;
#15799 = AXIS2_PLACEMENT_3D ( 'NONE', #11961, #24351, #20719 ) ;
#15800 = EDGE_LOOP ( 'NONE', ( #14993, #20705, #13467 ) ) ;
#15801 = EDGE_CURVE ( 'NONE', #26077, #10259, #29572, .T. ) ;
#15802 = CARTESIAN_POINT ( 'NONE',  ( 0.000000000000000000, 22.50000000000000355, 7.000000000000000000 ) ) ;
#15803 = ORIENTED_EDGE ( 'NONE', *, *, #28481, .F. ) ;
#15804 = B_SPLINE_CURVE_WITH_KNOTS ( 'NONE', 3,
 ( #22903, #7463, #19872, #4424, #4628, #26761 ),
 .UNSPECIFIED., .F., .F.,
 ( 4, 2, 4 ),
 ( 0.000000000000000000, 0.1492836598722001307, 0.2985673197444002613 ),
 .UNSPECIFIED. ) ;
#15805 = DIRECTION ( 'NONE',  ( -0.000000000000000000, -0.000000000000000000, -1.000000000000000000 ) ) ;
#15806 = DIRECTION ( 'NONE',  ( 0.6691306063588670083, 0.7431448254773862505, -0.000000000000000000 ) ) ;
#15807 = EDGE_CURVE ( 'NONE', #27094, #12629, #26530, .T. ) ;
#15808 = DIRECTION ( 'NONE',  ( 0.5000000000000039968, 0.8660254037844363761, 0.000000000000000000 ) ) ;
#15809 = ORIENTED_EDGE ( 'NONE', *, *, #34498, .T. ) ;
#15810 = AXIS2_PLACEMENT_3D ( 'NONE', #17578, #20418, #35653 ) ;
#15811 = CARTESIAN_POINT ( 'NONE',  ( -1.699711140334807302, 21.35824065759481627, -25.59207206193138973 ) ) ;
#15812 = CARTESIAN_POINT ( 'NONE',  ( -9.427394655437487003, 10.98460639141788242, 10.49999999999999822 ) ) ;
#15813 = DIRECTION ( 'NONE',  ( 0.8090169943749426773, -0.5877852522924796874, 0.000000000000000000 ) ) ;
#15814 = CARTESIAN_POINT ( 'NONE',  ( 10.33795143809920702, 20.40792924032132660, 10.50000000000000000 ) ) ;
#15815 = LINE ( 'NONE', #578, #12589 ) ;
#15816 = DIRECTION ( 'NONE',  ( 1.000000000000000000, 0.000000000000000000, 0.000000000000000000 ) ) ;
#15817 = AXIS2_PLACEMENT_3D ( 'NONE', #6854, #1178, #36114 ) ;
#15818 = CARTESIAN_POINT ( 'NONE',  ( 13.25468081180020263, 29.55206051663221345, -9.525608598956070594 ) ) ;
#15819 = ORIENTED_EDGE ( 'NONE', *, *, #23533, .F. ) ;
#15820 = CARTESIAN_POINT ( 'NONE',  ( -21.21721043375235283, 12.69857392348516711, -6.454068583460846220 ) ) ;
#15821 = CARTESIAN_POINT ( 'NONE',  ( -2.166144593658632989, 42.50000000000004974, 22.99999999999999289 ) ) ;
#15822 = CARTESIAN_POINT ( 'NONE',  ( 15.30366455603881803, -26.31361304454697603, -8.292863508495639024 ) ) ;
#15823 = FACE_OUTER_BOUND ( 'NONE', #37032, .T. ) ;
#15824 = CARTESIAN_POINT ( 'NONE',  ( 14.71377148196451934, 25.46827901036206399, -10.64846216776593657 ) ) ;
#15825 = EDGE_CURVE ( 'NONE', #1914, #22876, #8843, .T. ) ;
#15826 = CARTESIAN_POINT ( 'NONE',  ( 11.41987377193677489, -19.41918266173338026, -20.90349153980996988 ) ) ;
#15827 = PLANE ( 'NONE',  #25843 ) ;
#15828 = ADVANCED_FACE ( 'NONE', ( #27716 ), #14024, .T. ) ;
#15829 = AXIS2_PLACEMENT_3D ( 'NONE', #12900, #28539, #715 ) ;
#15830 = CARTESIAN_POINT ( 'NONE',  ( -24.44490540209602614, -24.40828659446678373, -10.25875033300979311 ) ) ;
#15831 = CARTESIAN_POINT ( 'NONE',  ( 11.94839969841157590, -24.33362986171098186, -12.62691988318393221 ) ) ;
#15832 = CARTESIAN_POINT ( 'NONE',  ( 15.15622143329154525, 25.96001174859074467, -8.769384549947115914 ) ) ;
#15833 = CARTESIAN_POINT ( 'NONE',  ( 24.38153214571670446, -17.61758732495730939, -15.69893765422416010 ) ) ;
#15834 = CARTESIAN_POINT ( 'NONE',  ( 8.395951170269764674, 10.09331379572982357, 10.68306085400111982 ) ) ;
#15835 = CARTESIAN_POINT ( 'NONE',  ( -10.14060191828655100, 25.26915018278946690, 11.00000000000000000 ) ) ;
#15836 = ORIENTED_EDGE ( 'NONE', *, *, #27748, .T. ) ;
#15837 = CARTESIAN_POINT ( 'NONE',  ( -7.072584127764374173, 21.29840595540943937, -23.29275699177380332 ) ) ;
#15838 = CYLINDRICAL_SURFACE ( 'NONE', #2408, 1.000000000000000000 ) ;
#15839 = CARTESIAN_POINT ( 'NONE',  ( 11.11016527260166420, 31.83082137946473367, 7.499999999999997335 ) ) ;
#15840 = CIRCLE ( 'NONE', #11324, 1.000000000000000000 ) ;
#15841 = DIRECTION ( 'NONE',  ( -0.000000000000000000, -0.000000000000000000, -1.000000000000000000 ) ) ;
#15842 = VERTEX_POINT ( 'NONE', #37466 ) ;
#15843 = CARTESIAN_POINT ( 'NONE',  ( 29.96329728503961221, 0.06029566601255719610, -9.238937171761827827 ) ) ;
#15844 = CARTESIAN_POINT ( 'NONE',  ( -14.46080647158818522, 26.53523365061255745, 10.49999999999999822 ) ) ;
#15845 = CARTESIAN_POINT ( 'NONE',  ( -9.151574469205524309, 1.945227203041487218, 11.00000000000000000 ) ) ;
#15846 = B_SPLINE_SURFACE_WITH_KNOTS ( 'NONE', 1, 3, ( 
 ( #39156, #22908, #26161, #29816, #4429, #14582, #38556, #23115, #38353, #8076 ),
 ( #20278, #1385, #35514, #20485, #20079, #17443, #17034, #32879, #11337, #5234 ) ),
 .UNSPECIFIED., .F., .F., .F.,
 ( 2, 2 ),
 ( 4, 2, 2, 2, 4 ),
 ( 0.000000000000000000, 1.000000000000000000 ),
 ( 1.570796326794891673, 1.963495408493616923, 2.356194490192342172, 2.748893571891067644, 3.141592653589793116 ),
 .UNSPECIFIED. ) ;
#15847 = ORIENTED_EDGE ( 'NONE', *, *, #3771, .F. ) ;
#15848 = CARTESIAN_POINT ( 'NONE',  ( -30.13613696638300610, 0.06374650685281088580, -8.768336777620580946 ) ) ;
#15849 = CYLINDRICAL_SURFACE ( 'NONE', #16402, 1.000000000000000000 ) ;
#15850 = ADVANCED_FACE ( 'NONE', ( #33832 ), #6375, .F. ) ;
#15851 = ORIENTED_EDGE ( 'NONE', *, *, #3553, .F. ) ;
#15852 = CARTESIAN_POINT ( 'NONE',  ( 20.29344634343774700, -4.154788219150724160, -27.84155812886654502 ) ) ;
#15853 = ADVANCED_FACE ( 'NONE', ( #30779 ), #34419, .F. ) ;
#15854 = ORIENTED_EDGE ( 'NONE', *, *, #25457, .T. ) ;
#15855 = CARTESIAN_POINT ( 'NONE',  ( 9.166052203147213362, 37.72018303276097129, 13.32518128616612962 ) ) ;
#15856 = FACE_OUTER_BOUND ( 'NONE', #39773, .T. ) ;
#15857 = DIRECTION ( 'NONE',  ( -0.000000000000000000, -0.000000000000000000, -1.000000000000000000 ) ) ;
#15858 = CARTESIAN_POINT ( 'NONE',  ( 10.78342637327578046, 29.81468131102270291, 18.87996532025786323 ) ) ;
#15859 = VECTOR ( 'NONE', #25993, 1000.000000000000000 ) ;
#15860 = EDGE_CURVE ( 'NONE', #6329, #20052, #294, .T. ) ;
#15861 = DIRECTION ( 'NONE',  ( 1.000000000000000000, 0.000000000000000000, 0.000000000000000000 ) ) ;
#15862 = ORIENTED_EDGE ( 'NONE', *, *, #9034, .T. ) ;
#15863 = DIRECTION ( 'NONE',  ( 1.000000000000000000, 0.000000000000000000, 0.000000000000000000 ) ) ;
#15864 = CARTESIAN_POINT ( 'NONE',  ( -19.71057812522863628, 5.645469553838248444, -29.99999999999999645 ) ) ;
#15865 = CARTESIAN_POINT ( 'NONE',  ( 10.14060191828658120, 25.26915018278934255, 10.50000000000000000 ) ) ;
#15866 = DIRECTION ( 'NONE',  ( -0.000000000000000000, -0.000000000000000000, -1.000000000000000000 ) ) ;
#15867 = CARTESIAN_POINT ( 'NONE',  ( 16.01654674860193595, 17.47364687737974975, -16.80141053676624452 ) ) ;
#15868 = CARTESIAN_POINT ( 'NONE',  ( 8.811643058094634995, 34.19349861355132703, -9.354887791571313116 ) ) ;
#15869 = CARTESIAN_POINT ( 'NONE',  ( 11.31110988152877894, -17.30322875125625615, -27.97697571136258787 ) ) ;
#15870 = CYLINDRICAL_SURFACE ( 'NONE', #28803, 57.00000000000003553 ) ;
#15871 = EDGE_CURVE ( 'NONE', #17841, #38914, #18590, .T. ) ;
#15872 = CARTESIAN_POINT ( 'NONE',  ( -12.56321727241662423, 14.36790371874266370, 10.49999999999999467 ) ) ;
#15873 = EDGE_CURVE ( 'NONE', #34838, #30940, #3137, .T. ) ;
#15874 = VECTOR ( 'NONE', #5676, 1000.000000000000000 ) ;
#15875 = ORIENTED_EDGE ( 'NONE', *, *, #7273, .F. ) ;
#15876 = CARTESIAN_POINT ( 'NONE',  ( -12.15709906223975700, 19.89297644826506328, -20.54567599615587881 ) ) ;
#15877 = CARTESIAN_POINT ( 'NONE',  ( -32.26343921792069835, -3.257266818579767964, 17.42190598798350365 ) ) ;
#15878 = CARTESIAN_POINT ( 'NONE',  ( 13.46238087013228579, -24.08803019759326247, -13.52451462657619352 ) ) ;
#15879 = CARTESIAN_POINT ( 'NONE',  ( -10.70158575030357895, 30.79011836036732319, 10.50000000000000000 ) ) ;
#15880 = VERTEX_POINT ( 'NONE', #27523 ) ;
#15881 = ORIENTED_EDGE ( 'NONE', *, *, #6213, .T. ) ;
#15882 = CARTESIAN_POINT ( 'NONE',  ( -14.16754981693137339, 28.95138659793071056, -8.202177504148025378 ) ) ;
#15883 = CIRCLE ( 'NONE', #19127, 0.5000000000000015543 ) ;
#15884 = CARTESIAN_POINT ( 'NONE',  ( -19.33876548823874231, -27.12358307434724125, -6.816496654975429337 ) ) ;
#15885 = FACE_BOUND ( 'NONE', #11003, .T. ) ;
#15886 = AXIS2_PLACEMENT_3D ( 'NONE', #33520, #30464, #7053 ) ;
#15887 = EDGE_LOOP ( 'NONE', ( #5713, #26185, #16354, #2547 ) ) ;
#15888 = CARTESIAN_POINT ( 'NONE',  ( -34.02488686188301159, -10.57580012044028805, -9.338804097880540667 ) ) ;
#15889 = CARTESIAN_POINT ( 'NONE',  ( -10.11677155123750005, -19.20203320946534475, -23.86710499911539785 ) ) ;
#15890 = CARTESIAN_POINT ( 'NONE',  ( 5.982165713378432059, 28.55918256678898715, 9.000000000000001776 ) ) ;
#15891 = ORIENTED_EDGE ( 'NONE', *, *, #1682, .T. ) ;
#15892 = CARTESIAN_POINT ( 'NONE',  ( 30.70345270623383627, 0.1631843812369964120, -5.474135951704134584 ) ) ;
#15893 = DIRECTION ( 'NONE',  ( 0.000000000000000000, 0.000000000000000000, -1.000000000000000000 ) ) ;
#15894 = DIRECTION ( 'NONE',  ( -0.8660254037844364872, 0.5000000000000038858, 0.000000000000000000 ) ) ;
#15895 = ORIENTED_EDGE ( 'NONE', *, *, #34124, .F. ) ;
#15896 = CARTESIAN_POINT ( 'NONE',  ( -30.39538365534349040, -0.04934266608166847090, -8.295282253696063535 ) ) ;
#15897 = ORIENTED_EDGE ( 'NONE', *, *, #13603, .F. ) ;
#15898 = CARTESIAN_POINT ( 'NONE',  ( 31.65024234132572545, -1.763089522669275322, -8.678469945394718721 ) ) ;
#15899 = CARTESIAN_POINT ( 'NONE',  ( -9.819550942989188513, -18.04686579641860078, -30.00000000000000000 ) ) ;
#15900 = CARTESIAN_POINT ( 'NONE',  ( 25.49851591039082876, -25.57752154475394946, 16.87380292611441845 ) ) ;
#15901 = ADVANCED_FACE ( 'NONE', ( #9041 ), #5980, .T. ) ;
#15902 = VERTEX_POINT ( 'NONE', #40107 ) ;
#15903 = CARTESIAN_POINT ( 'NONE',  ( -26.55359138347274239, 4.403205473926642632, -8.349092865648199080 ) ) ;
#15904 = CARTESIAN_POINT ( 'NONE',  ( -20.66733686379708956, -29.21156249568803531, -4.999999999999997335 ) ) ;
#15905 = CIRCLE ( 'NONE', #30815, 6.000000000000006217 ) ;
#15906 = CARTESIAN_POINT ( 'NONE',  ( 0.5415361484146276050, 27.50000000000005684, 20.99999999999998934 ) ) ;
#15907 = DIRECTION ( 'NONE',  ( -0.6724985119639582676, -0.2185080122244135170, -0.7071067811865457964 ) ) ;
#15908 = DIRECTION ( 'NONE',  ( -0.000000000000000000, -0.000000000000000000, -1.000000000000000000 ) ) ;
#15909 = VECTOR ( 'NONE', #26720, 1000.000000000000000 ) ;
#15910 = AXIS2_PLACEMENT_3D ( 'NONE', #4417, #20472, #35905 ) ;
#15911 = TOROIDAL_SURFACE ( 'NONE', #29548, 1.000000000000000000, 0.5000000000000000000 ) ;
#15912 = FACE_BOUND ( 'NONE', #4755, .T. ) ;
#15913 = PLANE ( 'NONE',  #1037 ) ;
#15914 = CARTESIAN_POINT ( 'NONE',  ( -19.48816862725384169, 6.402609444000542993, -29.41693484488668631 ) ) ;
#15915 = DIRECTION ( 'NONE',  ( 1.000000000000000000, 0.000000000000000000, 0.000000000000000000 ) ) ;
#15916 = CARTESIAN_POINT ( 'NONE',  ( 23.69164916738933258, -26.06248331711220345, -8.067269366965431843 ) ) ;
#15917 = CARTESIAN_POINT ( 'NONE',  ( -13.05736835487441994, 16.11602540378456183, 10.49999999999999822 ) ) ;
#15918 = CARTESIAN_POINT ( 'NONE',  ( 10.86287567075531157, 17.54031720676627515, -28.06684646824993123 ) ) ;
#15919 = EDGE_LOOP ( 'NONE', ( #9454, #24637, #6494, #11974 ) ) ;
#15920 = CARTESIAN_POINT ( 'NONE',  ( -14.28253842008971297, 21.30371530270891256, -15.55968883884288445 ) ) ;
#15921 = CARTESIAN_POINT ( 'NONE',  ( -28.61121519738577135, -15.27903652329813333, 20.25080042701592120 ) ) ;
#15922 = EDGE_CURVE ( 'NONE', #697, #20919, #15329, .T. ) ;
#15923 = LINE ( 'NONE', #16731, #13995 ) ;
#15924 = CARTESIAN_POINT ( 'NONE',  ( 14.76097837988864825, 25.32778234306308462, -10.65473370507753437 ) ) ;
#15925 = ORIENTED_EDGE ( 'NONE', *, *, #17514, .T. ) ;
#15926 = EDGE_CURVE ( 'NONE', #31607, #6918, #11459, .T. ) ;
#15927 = CARTESIAN_POINT ( 'NONE',  ( -5.706342468480190000, 20.64589803375067945, 6.000000000000000000 ) ) ;
#15928 = VERTEX_POINT ( 'NONE', #24278 ) ;
#15930 = DIRECTION ( 'NONE',  ( 0.8090169943749505599, 0.5877852522924689183, 0.000000000000000000 ) ) ;
#15929 = CARTESIAN_POINT ( 'NONE',  ( -11.58297502488001385, 19.01036633197951176, -22.71718434665674380 ) ) ;
#15931 = CARTESIAN_POINT ( 'NONE',  ( -9.708379805665277473, -18.29787746346482891, -27.44150705248273425 ) ) ;
#15932 = DIRECTION ( 'NONE',  ( 1.000000000000000000, 0.000000000000000000, 0.000000000000000000 ) ) ;
#15933 = ORIENTED_EDGE ( 'NONE', *, *, #186, .T. ) ;
#15934 = CARTESIAN_POINT ( 'NONE',  ( -34.37712449666406656, -15.41263033719045339, -7.552124065748168746 ) ) ;
#15935 = CARTESIAN_POINT ( 'NONE',  ( -11.23442614370865833, -21.53855194063014267, -18.51691792380379198 ) ) ;
#15936 = DIRECTION ( 'NONE',  ( -0.5877852522924797984, -0.8090169943749425663, 0.000000000000000000 ) ) ;
#15937 = CARTESIAN_POINT ( 'NONE',  ( 15.29729418701016996, 21.14454537556351355, -13.64836929760071094 ) ) ;
#15938 = ORIENTED_EDGE ( 'NONE', *, *, #19552, .T. ) ;
#15939 = CARTESIAN_POINT ( 'NONE',  ( 25.09639509413040059, 5.514876398772647903, -10.80109637251452881 ) ) ;
#15940 = DIRECTION ( 'NONE',  ( 1.000000000000000000, 0.000000000000000000, 0.000000000000000000 ) ) ;
#15941 = LINE ( 'NONE', #37674, #36821 ) ;
#15942 = ADVANCED_FACE ( 'NONE', ( #24673 ), #18976, .T. ) ;
#15943 = CARTESIAN_POINT ( 'NONE',  ( -0.4999999999999998890, 37.00000000000000711, 7.000000000000000000 ) ) ;
#15944 = CIRCLE ( 'NONE', #12081, 15.00000000000000000 ) ;
#15945 = ORIENTED_EDGE ( 'NONE', *, *, #9844, .F. ) ;
#15946 = CARTESIAN_POINT ( 'NONE',  ( -20.49328727640310888, 0.5260942599782594264, -29.99999999999999645 ) ) ;
#15947 = CARTESIAN_POINT ( 'NONE',  ( 21.29626117702810362, 0.6323340879910104295, -24.99883547235564407 ) ) ;
#15948 = AXIS2_PLACEMENT_3D ( 'NONE', #11074, #29152, #13703 ) ;
#15949 = CIRCLE ( 'NONE', #23100, 0.4999999999999998335 ) ;
#15950 = CARTESIAN_POINT ( 'NONE',  ( 29.20803623499950419, -13.20745421916094209, 20.25080042701566541 ) ) ;
#15951 = VERTEX_POINT ( 'NONE', #34026 ) ;
#15952 = CARTESIAN_POINT ( 'NONE',  ( -3.859759734048395785E-14, -22.74351282448223799, -21.56489709563626533 ) ) ;
#15953 = DIRECTION ( 'NONE',  ( 1.000000000000000000, 0.000000000000000000, 0.000000000000000000 ) ) ;
#15954 = ORIENTED_EDGE ( 'NONE', *, *, #662, .T. ) ;
#15955 = EDGE_CURVE ( 'NONE', #37418, #28046, #3532, .T. ) ;
#15956 = B_SPLINE_CURVE_WITH_KNOTS ( 'NONE', 3,
 ( #26651, #23610, #17527, #7197, #26853, #9372, #15261, #14865, #33368, #21748, #33767, #3068, #12012, #24004, #27649, #27253, #12410, #8972 ),
 .UNSPECIFIED., .F., .F.,
 ( 4, 2, 2, 2, 2, 2, 2, 2, 4 ),
 ( 0.000000000000000000, 0.1250000000000000833, 0.2500000000000001665, 0.3750000000000002220, 0.5000000000000003331, 0.6250000000000004441, 0.7500000000000002220, 0.8750000000000001110, 1.000000000000000000 ),
 .UNSPECIFIED. ) ;
#15957 = CARTESIAN_POINT ( 'NONE',  ( 12.99377146717206344, 26.19620116591418224, 10.50000000000000000 ) ) ;
#15958 = CARTESIAN_POINT ( 'NONE',  ( 5.440908595777817602, 35.94977745735560859, 7.500000000000000888 ) ) ;
#15959 = DIRECTION ( 'NONE',  ( 0.000000000000000000, 0.000000000000000000, 1.000000000000000000 ) ) ;
#15960 = CARTESIAN_POINT ( 'NONE',  ( 5.015607813569435969, 30.50653394152838516, -14.78114538601825600 ) ) ;
#15961 = CARTESIAN_POINT ( 'NONE',  ( 3.326583613081082635, 38.15036234293571482, 12.00000000000000000 ) ) ;
#15962 = CARTESIAN_POINT ( 'NONE',  ( 14.41430201638238984, 20.48224166989774631, 10.99999999999999289 ) ) ;
#15963 = CYLINDRICAL_SURFACE ( 'NONE', #30479, 0.4999999999999999445 ) ;
#15964 = CARTESIAN_POINT ( 'NONE',  ( -3.597409820281606940, 14.42008525284352594, 7.000000000000000000 ) ) ;
#15965 = PLANE ( 'NONE',  #4763 ) ;
#15966 = CARTESIAN_POINT ( 'NONE',  ( 9.303655249773155944, 10.73386218874824216, 7.000000000000000000 ) ) ;
#15967 = CARTESIAN_POINT ( 'NONE',  ( 14.59836673145885122, 27.18161558271501832, -9.180379322459677027 ) ) ;
#15969 = CIRCLE ( 'NONE', #32840, 1.000000000000000000 ) ;
#15968 = FACE_OUTER_BOUND ( 'NONE', #18142, .T. ) ;
#15970 = ORIENTED_EDGE ( 'NONE', *, *, #11235, .F. ) ;
#15972 = DIRECTION ( 'NONE',  ( 1.000000000000000000, 0.000000000000000000, 0.000000000000000000 ) ) ;
#15971 = CARTESIAN_POINT ( 'NONE',  ( -16.12111101626893372, 14.39761757377728912, -22.15277786026702245 ) ) ;
#15973 = CARTESIAN_POINT ( 'NONE',  ( 7.659620408498160060, 26.92228390473674793, 9.000000000000001776 ) ) ;
#15974 = CIRCLE ( 'NONE', #30887, 1.000000000000000000 ) ;
#15975 = EDGE_CURVE ( 'NONE', #37255, #19619, #17295, .T. ) ;
#15976 = CARTESIAN_POINT ( 'NONE',  ( 15.10398894348100995, -26.26589654887872527, -8.298239031644310870 ) ) ;
#15977 = CARTESIAN_POINT ( 'NONE',  ( 8.927394655428274817, 11.06314620770945290, 7.000000000000000000 ) ) ;
#15978 = CARTESIAN_POINT ( 'NONE',  ( 15.42079449665415680, 26.76609254708107244, -5.474200704454040611 ) ) ;
#15979 = CARTESIAN_POINT ( 'NONE',  ( 14.83638920640944292, 25.62079248104728535, -10.17951853491134351 ) ) ;
#15980 = ORIENTED_EDGE ( 'NONE', *, *, #31958, .F. ) ;
#15981 = LINE ( 'NONE', #15381, #2986 ) ;
#15982 = CARTESIAN_POINT ( 'NONE',  ( -14.63471340173679280, -25.63113514326269993, -10.18257656473890371 ) ) ;
#15983 = CARTESIAN_POINT ( 'NONE',  ( -26.32119069355245955, -27.53777429989661485, 13.32518128616608877 ) ) ;
#15984 = CARTESIAN_POINT ( 'NONE',  ( -16.53721940376430055, -12.13086247549455443, -29.21783723221567186 ) ) ;
#15985 = CARTESIAN_POINT ( 'NONE',  ( -4.434780010005740181, -23.77905508842546922, -12.85394067315957578 ) ) ;
#15986 = CARTESIAN_POINT ( 'NONE',  ( 12.01796449282804424, 18.59096114822754231, -22.78820876937768247 ) ) ;
#15987 = ADVANCED_FACE ( 'NONE', ( #34222 ), #36672, .F. ) ;
#15988 = EDGE_LOOP ( 'NONE', ( #7186, #15715 ) ) ;
#15989 = CARTESIAN_POINT ( 'NONE',  ( 18.25678040558227622, 9.365065964941067023, -28.86123873035057130 ) ) ;
#15990 = CARTESIAN_POINT ( 'NONE',  ( -5.440908595777636414, 35.94977745735568675, 7.000000000000000000 ) ) ;
#15991 = EDGE_CURVE ( 'NONE', #30348, #12011, #39341, .T. ) ;
#15992 = CARTESIAN_POINT ( 'NONE',  ( -10.74031445979289856, 33.85370084240260269, 16.87380292611523913 ) ) ;
#15993 = ORIENTED_EDGE ( 'NONE', *, *, #34983, .F. ) ;
#15994 = CARTESIAN_POINT ( 'NONE',  ( -24.21134473998290559, -3.011152994252887627, -20.11598446922123884 ) ) ;
#15995 = CARTESIAN_POINT ( 'NONE',  ( -24.95394407863866704, 1.780357051476928243, 18.87996532026248175 ) ) ;
#15996 = ORIENTED_EDGE ( 'NONE', *, *, #21290, .T. ) ;
#15997 = DIRECTION ( 'NONE',  ( -0.6691306063588653430, -0.7431448254773878048, 0.000000000000000000 ) ) ;
#15998 = CARTESIAN_POINT ( 'NONE',  ( 9.697889840765407499, 31.90483559858327212, 7.000000000000000000 ) ) ;
#15999 = CARTESIAN_POINT ( 'NONE',  ( -29.21372990917784662, 0.8930521456687262605, -9.252833956221683920 ) ) ;
#16000 = CARTESIAN_POINT ( 'NONE',  ( 25.45230351418204151, -11.15605511405185091, -17.62830037521853299 ) ) ;
#16001 = CARTESIAN_POINT ( 'NONE',  ( 22.67022523934590694, -28.72937257582105275, 13.32518128616577080 ) ) ;
#16002 = VECTOR ( 'NONE', #12676, 1000.000000000000000 ) ;
#16003 = ORIENTED_EDGE ( 'NONE', *, *, #4197, .F. ) ;
#16004 = EDGE_CURVE ( 'NONE', #19822, #33574, #14706, .T. ) ;
#16005 = ORIENTED_EDGE ( 'NONE', *, *, #29264, .F. ) ;
#16006 = EDGE_CURVE ( 'NONE', #31354, #400, #3930, .T. ) ;
#16007 = CARTESIAN_POINT ( 'NONE',  ( -6.686869517299739663, 14.99761530854305391, 10.50000000000000533 ) ) ;
#16008 = DIRECTION ( 'NONE',  ( -1.000000000000000000, 0.000000000000000000, 0.000000000000000000 ) ) ;
#16009 = CARTESIAN_POINT ( 'NONE',  ( -4.003810537522578983, 8.420815593655365916, 10.49999999999999822 ) ) ;
#16010 = EDGE_LOOP ( 'NONE', ( #35949, #4001, #39093 ) ) ;
#16011 = CARTESIAN_POINT ( 'NONE',  ( -2.776705887744885803, 34.22514237022959804, -11.98289488661590951 ) ) ;
#16012 = CARTESIAN_POINT ( 'NONE',  ( -9.408554248005561504, 10.90613044664337572, 10.49999999999999467 ) ) ;
#16013 = DIRECTION ( 'NONE',  ( 1.000000000000000000, 0.000000000000000000, 0.000000000000000000 ) ) ;
#16014 = CARTESIAN_POINT ( 'NONE',  ( -4.727507481117100063, 31.88885898370948269, 10.00000000000000000 ) ) ;
#16015 = DIRECTION ( 'NONE',  ( 1.000000000000000000, 0.000000000000000000, 0.000000000000000000 ) ) ;
#16016 = CARTESIAN_POINT ( 'NONE',  ( 10.21785616688032583, 25.03138605371555414, 10.75000000000000000 ) ) ;
#16017 = CARTESIAN_POINT ( 'NONE',  ( 10.12684856687054236, 24.03473075183826069, -18.03693486850220040 ) ) ;
#16018 = ORIENTED_EDGE ( 'NONE', *, *, #34596, .F. ) ;
#16019 = CARTESIAN_POINT ( 'NONE',  ( -19.94802261067724203, 11.91594554592121114, -14.92335899463314242 ) ) ;
#16020 = DIRECTION ( 'NONE',  ( 0.000000000000000000, 0.000000000000000000, 1.000000000000000000 ) ) ;
#16021 = CARTESIAN_POINT ( 'NONE',  ( 14.40609022250728444, -25.07970014599643349, -11.59567163901805387 ) ) ;
#16022 = LINE ( 'NONE', #13569, #12016 ) ;
#16023 = CARTESIAN_POINT ( 'NONE',  ( 11.85601099147671178, 19.42086764860403036, -21.61009544485835931 ) ) ;
#16024 = CARTESIAN_POINT ( 'NONE',  ( 16.77267017469755217, -29.13948811618736912, -13.79123840944735413 ) ) ;
#16025 = ADVANCED_FACE ( 'NONE', ( #35421 ), #16328, .F. ) ;
#16026 = DIRECTION ( 'NONE',  ( 0.6691306063588570163, -0.7431448254773953543, 0.000000000000000000 ) ) ;
#16027 = CIRCLE ( 'NONE', #24441, 1.000000000000000000 ) ;
#16028 = CARTESIAN_POINT ( 'NONE',  ( -17.82960224414886596, -17.77519942552612520, -19.83192060708631743 ) ) ;
#16029 = CARTESIAN_POINT ( 'NONE',  ( 6.772447531124758058, -21.91223081777216564, -18.87814742099377341 ) ) ;
#16030 = CARTESIAN_POINT ( 'NONE',  ( 11.44368038160577683, 17.93323933076874255, -25.03240686958881156 ) ) ;
#16031 = CARTESIAN_POINT ( 'NONE',  ( 26.97183419387431158, -19.50619947319538383, -12.90440121806097729 ) ) ;
#16032 = CARTESIAN_POINT ( 'NONE',  ( 8.412270287199559604, 10.07085245822950448, 10.49999999999999822 ) ) ;
#16033 = CARTESIAN_POINT ( 'NONE',  ( -0.3582326297815359162, 33.31072022568110924, 12.00000000000000000 ) ) ;
#16034 = ORIENTED_EDGE ( 'NONE', *, *, #12718, .T. ) ;
#16035 = CARTESIAN_POINT ( 'NONE',  ( -9.049625497917114458, 33.98022236337723712, -9.362205654903002383 ) ) ;
#16036 = DIRECTION ( 'NONE',  ( 0.2079116908177663092, 0.9781476007338042455, 0.000000000000000000 ) ) ;
#16037 = AXIS2_PLACEMENT_3D ( 'NONE', #14775, #2185, #17638 ) ;
#16038 = CARTESIAN_POINT ( 'NONE',  ( -0.6108529249775870307, 37.48755679569043053, 7.500000000000000888 ) ) ;
#16039 = ORIENTED_EDGE ( 'NONE', *, *, #17261, .T. ) ;
#16040 = CARTESIAN_POINT ( 'NONE',  ( 30.52100727590019957, -0.04949924042143036274, -7.826100079217978234 ) ) ;
#16041 = CARTESIAN_POINT ( 'NONE',  ( -14.33090402811213337, 26.16159042914076949, 10.49999999999999822 ) ) ;
#16042 = DIRECTION ( 'NONE',  ( 0.6345370204113957024, -0.5138379476002926660, 0.5773502691896373884 ) ) ;
#16043 = ORIENTED_EDGE ( 'NONE', *, *, #31988, .T. ) ;
#16044 = CARTESIAN_POINT ( 'NONE',  ( -20.96756735925385229, 0.8276901569395326286, -26.22661741445136840 ) ) ;
#16045 = CARTESIAN_POINT ( 'NONE',  ( -17.60052849991877721, -23.51059660139243590, -14.14515744553814258 ) ) ;
#16046 = ORIENTED_EDGE ( 'NONE', *, *, #37543, .T. ) ;
#16047 = CARTESIAN_POINT ( 'NONE',  ( 34.37689022701968611, -6.182391807707502629, -7.210918363890624683 ) ) ;
#16048 = ORIENTED_EDGE ( 'NONE', *, *, #1108, .F. ) ;
#16049 = CARTESIAN_POINT ( 'NONE',  ( -16.76301160834940873, 29.17407194211730825, 12.14047268033010596 ) ) ;
#16050 = DIRECTION ( 'NONE',  ( 0.000000000000000000, -0.000000000000000000, -1.000000000000000000 ) ) ;
#16051 = DIRECTION ( 'NONE',  ( 0.000000000000000000, 0.000000000000000000, 1.000000000000000000 ) ) ;
#16052 = EDGE_CURVE ( 'NONE', #8090, #21833, #35496, .T. ) ;
#16053 = CARTESIAN_POINT ( 'NONE',  ( 8.489237591500947033, 31.47375793094898810, 19.27171037444156099 ) ) ;
#16054 = AXIS2_PLACEMENT_3D ( 'NONE', #32595, #19789, #4754 ) ;
#16055 = AXIS2_PLACEMENT_3D ( 'NONE', #35526, #19886, #10951 ) ;
#16056 = LINE ( 'NONE', #5910, #7086 ) ;
#16057 = ORIENTED_EDGE ( 'NONE', *, *, #2091, .T. ) ;
#16058 = DIRECTION ( 'NONE',  ( 0.4539904997395417530, 0.8910065241883703413, 0.000000000000000000 ) ) ;
#16059 = CARTESIAN_POINT ( 'NONE',  ( 9.866575328975670800, 17.98194059978866122, -29.99999999999999645 ) ) ;
#16060 = DIRECTION ( 'NONE',  ( 1.000000000000000000, 0.000000000000000000, 0.000000000000000000 ) ) ;
#16061 = DIRECTION ( 'NONE',  ( 1.000000000000000000, 0.000000000000000000, 0.000000000000000000 ) ) ;
#16062 = CARTESIAN_POINT ( 'NONE',  ( 17.67500771205885712, 19.99486213594162010, -6.434741731482024996 ) ) ;
#16063 = AXIS2_PLACEMENT_3D ( 'NONE', #11704, #39918, #27537 ) ;
#16064 = CARTESIAN_POINT ( 'NONE',  ( 9.123773087559795769, 35.63818776545269174, -5.873441756282732129 ) ) ;
#16065 = ORIENTED_EDGE ( 'NONE', *, *, #31754, .F. ) ;
#16066 = CARTESIAN_POINT ( 'NONE',  ( 16.36351675325202137, -26.72998542747626871, -7.330931130651400451 ) ) ;
#16067 = DIRECTION ( 'NONE',  ( -0.5000000000000042188, -0.8660254037844361541, 0.000000000000000000 ) ) ;
#16068 = CARTESIAN_POINT ( 'NONE',  ( -12.17073081513906985, 14.31852474926588670, 10.49999999999999645 ) ) ;
#16069 = EDGE_CURVE ( 'NONE', #21179, #15193, #32246, .T. ) ;
#16070 = EDGE_LOOP ( 'NONE', ( #11730, #24874, #26415 ) ) ;
#16071 = CARTESIAN_POINT ( 'NONE',  ( -14.84491883786760980, 25.59395107166792727, -10.18114221944758135 ) ) ;
#16072 = CARTESIAN_POINT ( 'NONE',  ( -33.53288488731320882, -7.900844017968387867, 17.92354375535173361 ) ) ;
#16073 = CARTESIAN_POINT ( 'NONE',  ( 11.34245683043676500, -21.00257692745146443, -19.51844232644348764 ) ) ;
#16074 = ADVANCED_FACE ( 'NONE', ( #28916 ), #3727, .T. ) ;
#16075 = CARTESIAN_POINT ( 'NONE',  ( -2.476907992048017260, 18.63850621467409496, 6.000000000000000000 ) ) ;
#16076 = VERTEX_POINT ( 'NONE', #31561 ) ;
#16077 = ORIENTED_EDGE ( 'NONE', *, *, #13731, .F. ) ;
#16078 = CIRCLE ( 'NONE', #11624, 0.5000000000000000000 ) ;
#16079 = CARTESIAN_POINT ( 'NONE',  ( -12.84571259627460016, 30.17467865810253613, -9.499430740182077670 ) ) ;
#16080 = PLANE ( 'NONE',  #24980 ) ;
#16081 = FACE_BOUND ( 'NONE', #12191, .T. ) ;
#16082 = VECTOR ( 'NONE', #13839, 1000.000000000000227 ) ;
#16083 = AXIS2_PLACEMENT_3D ( 'NONE', #1555, #38521, #31823 ) ;
#16084 = EDGE_CURVE ( 'NONE', #1489, #7593, #15747, .T. ) ;
#16085 = CARTESIAN_POINT ( 'NONE',  ( -35.29093393616297902, -8.784390315875461042, -5.878240462516181708 ) ) ;
#16086 = CARTESIAN_POINT ( 'NONE',  ( -11.43337157596636544, -20.99096340568458530, -19.50882303433272469 ) ) ;
#16087 = CARTESIAN_POINT ( 'NONE',  ( -14.64211604268330902, 20.79918788657763429, 13.00000000000000178 ) ) ;
#16088 = ORIENTED_EDGE ( 'NONE', *, *, #17381, .F. ) ;
#16089 = CARTESIAN_POINT ( 'NONE',  ( 23.53087566707228007, 1.464397449701676068, -19.60697909502530223 ) ) ;
#16090 = DIRECTION ( 'NONE',  ( 0.000000000000000000, 0.000000000000000000, 1.000000000000000000 ) ) ;
#16091 = FACE_OUTER_BOUND ( 'NONE', #24834, .T. ) ;
#16092 = AXIS2_PLACEMENT_3D ( 'NONE', #9012, #36647, #28089 ) ;
#16093 = VERTEX_POINT ( 'NONE', #10228 ) ;
#16094 = CARTESIAN_POINT ( 'NONE',  ( -30.04181568689138260, -0.02446475513555576228, -9.235284800656327064 ) ) ;
#16095 = EDGE_LOOP ( 'NONE', ( #20163, #23550 ) ) ;
#16096 = CARTESIAN_POINT ( 'NONE',  ( 24.40599740997825862, -0.7005350811509940545, -19.34016958161941346 ) ) ;
#16097 = AXIS2_PLACEMENT_3D ( 'NONE', #33750, #8352, #36580 ) ;
#16098 = CARTESIAN_POINT ( 'NONE',  ( 23.74914942275265162, -8.582573258223918700, 21.00000000000001776 ) ) ;
#16099 = CARTESIAN_POINT ( 'NONE',  ( 18.93294331123277985, -26.86907422048189176, 16.87380292611448951 ) ) ;
#16100 = ORIENTED_EDGE ( 'NONE', *, *, #31983, .T. ) ;
#16101 = ADVANCED_FACE ( 'NONE', ( #10030 ), #29631, .T. ) ;
#16102 = ADVANCED_FACE ( 'NONE', ( #22615 ), #32172, .F. ) ;
#16103 = CARTESIAN_POINT ( 'NONE',  ( 3.295881626406574672, 9.398963235502481695, 10.00000000000000000 ) ) ;
#16104 = EDGE_CURVE ( 'NONE', #11163, #34728, #16130, .T. ) ;
#16105 = CARTESIAN_POINT ( 'NONE',  ( 4.791301586986472572, 25.75006569903030851, 21.00000000000000355 ) ) ;
#16106 = DIRECTION ( 'NONE',  ( -0.000000000000000000, -0.000000000000000000, -1.000000000000000000 ) ) ;
#16107 = CYLINDRICAL_SURFACE ( 'NONE', #36380, 1.000000000000000888 ) ;
#16108 = AXIS2_PLACEMENT_3D ( 'NONE', #32498, #2413, #2020 ) ;
#16109 = CONICAL_SURFACE ( 'NONE', #35579, 1.000000000000000888, 0.7853981633974487231 ) ;
#16110 = CARTESIAN_POINT ( 'NONE',  ( -11.30412111481561510, 32.00546000420963821, 10.94611345180490680 ) ) ;
#16111 = CARTESIAN_POINT ( 'NONE',  ( 25.71480618106366478, 9.014447550976075973, 11.00000000000101963 ) ) ;
#16112 = CARTESIAN_POINT ( 'NONE',  ( -23.00670302975767001, 8.813160239992733125, -10.36552060695138522 ) ) ;
#16113 = CARTESIAN_POINT ( 'NONE',  ( 22.73890499347229266, -26.44294304952364527, -7.647982415843417314 ) ) ;
#16114 = VECTOR ( 'NONE', #10455, 1000.000000000000000 ) ;
#16115 = CARTESIAN_POINT ( 'NONE',  ( -14.44707628845733005, 26.53512579137188609, 7.497105610438111967 ) ) ;
#16116 = EDGE_CURVE ( 'NONE', #1841, #17659, #9831, .T. ) ;
#16117 = CARTESIAN_POINT ( 'NONE',  ( 15.29112707284399697, 26.78136894998224804, -6.884427309518560634 ) ) ;
#16118 = AXIS2_PLACEMENT_3D ( 'NONE', #2611, #14193, #32899 ) ;
#16119 = ORIENTED_EDGE ( 'NONE', *, *, #38670, .T. ) ;
#16120 = CARTESIAN_POINT ( 'NONE',  ( -15.45299194632486817, 25.37713463119194657, -8.304757890177965507 ) ) ;
#16121 = CARTESIAN_POINT ( 'NONE',  ( -21.12676971146075289, -20.25531951604057568, 20.50957957746008375 ) ) ;
#16122 = EDGE_CURVE ( 'NONE', #37631, #12591, #3672, .T. ) ;
#16123 = FACE_OUTER_BOUND ( 'NONE', #27620, .T. ) ;
#16124 = CARTESIAN_POINT ( 'NONE',  ( 15.04050438790828359, 25.89781307577547409, -9.239200427050345610 ) ) ;
#16125 = ORIENTED_EDGE ( 'NONE', *, *, #13082, .F. ) ;
#16126 = CARTESIAN_POINT ( 'NONE',  ( 18.46594824408953883, -9.479048207884551047, -27.70750746852463919 ) ) ;
#16127 = DIRECTION ( 'NONE',  ( 1.000000000000000000, 0.000000000000000000, 0.000000000000000000 ) ) ;
#16128 = ORIENTED_EDGE ( 'NONE', *, *, #14867, .T. ) ;
#16130 = LINE ( 'NONE', #1094, #6905 ) ;
#16129 = CARTESIAN_POINT ( 'NONE',  ( -15.21106512963387480, 26.79959205483123341, -7.350366708388557768 ) ) ;
#16131 = CARTESIAN_POINT ( 'NONE',  ( -10.12380078748041967, -18.23434954340907410, -26.79320281504661949 ) ) ;
#16132 = CYLINDRICAL_SURFACE ( 'NONE', #3013, 1.000000000000000888 ) ;
#16133 = ORIENTED_EDGE ( 'NONE', *, *, #37090, .T. ) ;
#16134 = CARTESIAN_POINT ( 'NONE',  ( -34.01707189250791430, -16.51593366370477867, -7.547920849479440086 ) ) ;
#16135 = CARTESIAN_POINT ( 'NONE',  ( -13.58096217418507834, -25.42507875219865809, -10.20197574081395686 ) ) ;
#16136 = DIRECTION ( 'NONE',  ( 1.000000000000000000, 0.000000000000000000, 0.000000000000000000 ) ) ;
#16137 = CARTESIAN_POINT ( 'NONE',  ( 12.82616162776056257, 17.22787463660536034, -24.04226039045894936 ) ) ;
#16138 = ORIENTED_EDGE ( 'NONE', *, *, #15364, .F. ) ;
#16139 = CARTESIAN_POINT ( 'NONE',  ( 20.54619531059088189, 5.238262143020175898, -24.25515232715240188 ) ) ;
#16140 = CARTESIAN_POINT ( 'NONE',  ( 19.26948696230199687, 27.85601271560034675, 3.000000000000000000 ) ) ;
#16141 = PLANE ( 'NONE',  #21844 ) ;
#16142 = CARTESIAN_POINT ( 'NONE',  ( -10.66948297901429932, 33.02599466632846514, 10.49999999999999822 ) ) ;
#16143 = ORIENTED_EDGE ( 'NONE', *, *, #9288, .F. ) ;
#16144 = CARTESIAN_POINT ( 'NONE',  ( -26.74272548658042936, -0.08550078280221545812, -15.40661396295627661 ) ) ;
#16146 = CARTESIAN_POINT ( 'NONE',  ( 31.05663563045704478, -0.3811732190980007817, -6.877908887127494708 ) ) ;
#16145 = VECTOR ( 'NONE', #10809, 999.9999999999998863 ) ;
#16147 = VECTOR ( 'NONE', #4500, 1000.000000000000114 ) ;
#16148 = CARTESIAN_POINT ( 'NONE',  ( 27.14644468510662279, -3.730463242941908231, 19.99202127657103389 ) ) ;
#16149 = EDGE_LOOP ( 'NONE', ( #23938, #6043, #24350, #31144, #39187 ) ) ;
#16150 = CIRCLE ( 'NONE', #20048, 17.00000000000000000 ) ;
#16151 = CARTESIAN_POINT ( 'NONE',  ( -37.62663912510979003, -8.659558992827880886, -14.26382729546507555 ) ) ;
#16152 = DIRECTION ( 'NONE',  ( 0.5254827454987487378, -0.4731467892558173238, 0.7071067811865534569 ) ) ;
#16153 = ORIENTED_EDGE ( 'NONE', *, *, #27265, .F. ) ;
#16154 = EDGE_CURVE ( 'NONE', #20195, #9989, #33687, .T. ) ;
#16155 = LINE ( 'NONE', #3559, #19746 ) ;
#16156 = LINE ( 'NONE', #26089, #17561 ) ;
#16157 = CARTESIAN_POINT ( 'NONE',  ( 0.9819609608163288872, 14.62372257652092422, 12.00000000000000000 ) ) ;
#16158 = CARTESIAN_POINT ( 'NONE',  ( 2.210526487218244185, 21.88195040076548992, -24.24797893842004370 ) ) ;
#16159 = DIRECTION ( 'NONE',  ( -0.8090169943749504489, -0.5877852522924690293, 0.000000000000000000 ) ) ;
#16160 = VERTEX_POINT ( 'NONE', #25862 ) ;
#16161 = CARTESIAN_POINT ( 'NONE',  ( -6.492361549288664158, 35.85278612139737220, 10.87262190629282799 ) ) ;
#16162 = CARTESIAN_POINT ( 'NONE',  ( 6.440829913680675034, 10.60893893836775348, 13.00000000000000178 ) ) ;
#16163 = CARTESIAN_POINT ( 'NONE',  ( 22.22908212014391793, -18.19034539544399465, -16.69010318239997304 ) ) ;
#16164 = LINE ( 'NONE', #35252, #8263 ) ;
#16165 = FACE_OUTER_BOUND ( 'NONE', #39542, .T. ) ;
#16166 = SURFACE_STYLE_USAGE ( .BOTH. , #37107 ) ;
#16167 = AXIS2_PLACEMENT_3D ( 'NONE', #5327, #14677, #33573 ) ;
#16168 = CARTESIAN_POINT ( 'NONE',  ( 14.97811516567272250, 26.90743356226946759, -8.273984026653725010 ) ) ;
#16169 = CYLINDRICAL_SURFACE ( 'NONE', #22362, 1.000000000000000000 ) ;
#16170 = AXIS2_PLACEMENT_3D ( 'NONE', #36515, #8483, #8279 ) ;
#16171 = ORIENTED_EDGE ( 'NONE', *, *, #10366, .F. ) ;
#16173 = DIRECTION ( 'NONE',  ( 1.000000000000000000, 0.000000000000000000, 0.000000000000000000 ) ) ;
#16172 = CARTESIAN_POINT ( 'NONE',  ( -18.60376045229827824, 17.50160579387829429, -7.896274594234498068 ) ) ;
#16174 = CARTESIAN_POINT ( 'NONE',  ( 37.09709568333406082, -7.051483854461560341, 11.00000000000008527 ) ) ;
#16175 = CARTESIAN_POINT ( 'NONE',  ( 15.04920134050132319, -26.13886538990421826, -8.767989598681507957 ) ) ;
#16176 = LINE ( 'NONE', #9875, #21757 ) ;
#16177 = CARTESIAN_POINT ( 'NONE',  ( 12.65668697161344980, 21.04834371600279397, -18.45301148604537644 ) ) ;
#16178 = ORIENTED_EDGE ( 'NONE', *, *, #39171, .F. ) ;
#16179 = CARTESIAN_POINT ( 'NONE',  ( 15.28655252905469730, 26.54335169034005659, -7.357393274253329452 ) ) ;
#16180 = VECTOR ( 'NONE', #15258, 1000.000000000000000 ) ;
#16181 = B_SPLINE_SURFACE_WITH_KNOTS ( 'NONE', 1, 3, ( 
 ( #20403, #14090, #32798, #4955, #39479, #14901, #29737, #2312, #26487, #23641 ),
 ( #24237, #14294, #2114, #30342, #26686, #26886, #38881, #2513, #36245, #11252 ) ),
 .UNSPECIFIED., .F., .F., .F.,
 ( 2, 2 ),
 ( 4, 2, 2, 2, 4 ),
 ( 0.000000000000000000, 1.000000000000000000 ),
 ( 4.237807397716013114, 4.630506479414739474, 5.023205561113466722, 5.415904642812193970, 5.808603724510920330 ),
 .UNSPECIFIED. ) ;
#16182 = VERTEX_POINT ( 'NONE', #16739 ) ;
#16183 = CARTESIAN_POINT ( 'NONE',  ( 3.229431105722923245, 20.49260818092372460, 13.00000000000000178 ) ) ;
#16184 = CARTESIAN_POINT ( 'NONE',  ( -9.507670998357182768, -18.30485029568063382, -28.08089151536464456 ) ) ;
#16185 = CARTESIAN_POINT ( 'NONE',  ( -35.73872160561192146, -18.42674013420461776, 13.32518128616620423 ) ) ;
#16186 = CARTESIAN_POINT ( 'NONE',  ( -30.78128484184130187, -22.64136542128004592, -5.436615360335371072 ) ) ;
#16187 = CARTESIAN_POINT ( 'NONE',  ( -1.766708854211077595, -20.47917438257665879, -29.42887188877706706 ) ) ;
#16188 = CARTESIAN_POINT ( 'NONE',  ( 15.74108267814583506, 25.56877728144000272, -5.946523357311115809 ) ) ;
#16189 = ORIENTED_EDGE ( 'NONE', *, *, #25481, .T. ) ;
#16190 = CARTESIAN_POINT ( 'NONE',  ( 18.63330078627290831, 8.706250619080577735, -28.29465965160086682 ) ) ;
#16191 = CARTESIAN_POINT ( 'NONE',  ( 7.688300058587269170, 16.47782454277055564, 13.00000000000000178 ) ) ;
#16192 = CARTESIAN_POINT ( 'NONE',  ( 1.681518492368163198, 38.03812643383474779, 16.87380292611441845 ) ) ;
#16193 = ORIENTED_EDGE ( 'NONE', *, *, #18070, .F. ) ;
#16194 = CARTESIAN_POINT ( 'NONE',  ( -33.99706561663532511, -4.510256399178081743, -5.454631704968152306 ) ) ;
#16195 = CARTESIAN_POINT ( 'NONE',  ( -16.15127118876187140, 15.63943246416160981, 18.87996532025774599 ) ) ;
#16196 = ORIENTED_EDGE ( 'NONE', *, *, #23281, .F. ) ;
#16197 = DIRECTION ( 'NONE',  ( 0.000000000000000000, 0.000000000000000000, -1.000000000000000000 ) ) ;
#16198 = CARTESIAN_POINT ( 'NONE',  ( 24.27939416804019856, -12.77206359138141067, 22.99999999999999645 ) ) ;
#16199 = CARTESIAN_POINT ( 'NONE',  ( -28.44303449390735494, 1.764778243225489041, -9.267788830656531474 ) ) ;
#16200 = CARTESIAN_POINT ( 'NONE',  ( 34.60165783442131726, -15.16164455357073493, -7.126201915243990825 ) ) ;
#16201 = CARTESIAN_POINT ( 'NONE',  ( 36.34526107768950709, -5.221918994412432014, 12.73282698324840467 ) ) ;
#16202 = AXIS2_PLACEMENT_3D ( 'NONE', #3175, #13299, #37298 ) ;
#16203 = ADVANCED_FACE ( 'NONE', ( #7372 ), #29324, .F. ) ;
#16204 = ORIENTED_EDGE ( 'NONE', *, *, #21555, .F. ) ;
#16205 = ORIENTED_EDGE ( 'NONE', *, *, #23363, .F. ) ;
#16206 = VECTOR ( 'NONE', #33115, 1000.000000000000000 ) ;
#16207 = CARTESIAN_POINT ( 'NONE',  ( 4.003793317224326742, 8.420815634768674229, 7.499999999999990230 ) ) ;
#16208 = CARTESIAN_POINT ( 'NONE',  ( -2.421689871081827317, 8.701977744317861863, 9.500000000000000000 ) ) ;
#16209 = DIRECTION ( 'NONE',  ( -0.5877852522924796874, -0.8090169943749426773, 0.000000000000000000 ) ) ;
#16210 = ORIENTED_EDGE ( 'NONE', *, *, #691, .F. ) ;
#16211 = ADVANCED_FACE ( 'NONE', ( #38464 ), #12774, .T. ) ;
#16212 = CARTESIAN_POINT ( 'NONE',  ( -0.7423364057732033672, 37.73799070049938109, -7.971040485890229732 ) ) ;
#16213 = EDGE_CURVE ( 'NONE', #13704, #7803, #2303, .T. ) ;
#16214 = DIRECTION ( 'NONE',  ( 0.6123724356957989112, 0.3535533905932687349, -0.7071067811865463515 ) ) ;
#16215 = LINE ( 'NONE', #13152, #27988 ) ;
#16216 = EDGE_CURVE ( 'NONE', #113, #8524, #38061, .T. ) ;
#16217 = DIRECTION ( 'NONE',  ( 0.6916548014802315070, 0.1470157664651950413, -0.7071067811865424657 ) ) ;
#16218 = DIRECTION ( 'NONE',  ( 0.9781476007338043566, -0.2079116908177657264, 0.000000000000000000 ) ) ;
#16219 = DIRECTION ( 'NONE',  ( -0.9781476007338042455, 0.2079116908177664758, 0.000000000000000000 ) ) ;
#16220 = CARTESIAN_POINT ( 'NONE',  ( 13.54008180094028369, 28.15075258002628900, -10.49033432201353477 ) ) ;
#16221 = DIRECTION ( 'NONE',  ( -1.000000000000000000, 0.000000000000000000, 0.000000000000000000 ) ) ;
#16222 = ORIENTED_EDGE ( 'NONE', *, *, #24007, .F. ) ;
#16224 = LINE ( 'NONE', #1384, #32360 ) ;
#16223 = CARTESIAN_POINT ( 'NONE',  ( -18.16760906032456191, 9.915766630534925241, -26.62071025163185212 ) ) ;
#16225 = CARTESIAN_POINT ( 'NONE',  ( -8.437494165184659778, 40.76200631401351160, 23.00000000000000000 ) ) ;
#16226 = CARTESIAN_POINT ( 'NONE',  ( 9.697117038158115321, -18.30344589899865682, -27.44232109050611612 ) ) ;
#16227 = CARTESIAN_POINT ( 'NONE',  ( -5.620290338810452369, 13.91368318151059214, 10.75000000000001066 ) ) ;
#16228 = CARTESIAN_POINT ( 'NONE',  ( 15.07355143598519653, 26.23066616942490725, -8.763531730697579292 ) ) ;
#16229 = CARTESIAN_POINT ( 'NONE',  ( -7.289639608743034849, -27.06962010326280321, -13.42901749168595060 ) ) ;
#16230 = LINE ( 'NONE', #13167, #34299 ) ;
#16231 = VECTOR ( 'NONE', #2634, 1000.000000000000000 ) ;
#16232 = CARTESIAN_POINT ( 'NONE',  ( -19.19123774765981594, -20.32519271048812470, -16.83485235770917043 ) ) ;
#16233 = CARTESIAN_POINT ( 'NONE',  ( 5.635282026549600864, -19.76630616200782242, -30.00000000000002132 ) ) ;
#16234 = CARTESIAN_POINT ( 'NONE',  ( 12.77347909899223666, 20.87875728061086633, -18.47285699837302886 ) ) ;
#16235 = CARTESIAN_POINT ( 'NONE',  ( 26.78380537101320158, -18.14658901527507595, -13.81421069608905050 ) ) ;
#16236 = EDGE_CURVE ( 'NONE', #13390, #18096, #31564, .T. ) ;
#16237 = DIRECTION ( 'NONE',  ( 1.000000000000000000, 0.000000000000000000, 0.000000000000000000 ) ) ;
#16238 = LINE ( 'NONE', #28620, #31942 ) ;
#16239 = EDGE_CURVE ( 'NONE', #34227, #31250, #23431, .T. ) ;
#16240 = VERTEX_POINT ( 'NONE', #11444 ) ;
#16241 = CIRCLE ( 'NONE', #35702, 1.000000000000000888 ) ;
#16242 = CARTESIAN_POINT ( 'NONE',  ( -6.503115034744880063, 27.62047085464899965, -16.75544015141223753 ) ) ;
#16243 = CARTESIAN_POINT ( 'NONE',  ( 14.56494338438156610, 21.47191690367849048, 10.99387789255783687 ) ) ;
#16244 = ORIENTED_EDGE ( 'NONE', *, *, #17367, .T. ) ;
#16245 = CARTESIAN_POINT ( 'NONE',  ( 30.36599317559471345, -0.01867231823262901699, -8.297552807227344118 ) ) ;
#16246 = FACE_OUTER_BOUND ( 'NONE', #32601, .T. ) ;
#16247 = CARTESIAN_POINT ( 'NONE',  ( 0.000000000000000000, 22.50000000000000355, 3.000000000000000000 ) ) ;
#16248 = ORIENTED_EDGE ( 'NONE', *, *, #18782, .T. ) ;
#16249 = CARTESIAN_POINT ( 'NONE',  ( -29.84897892274408804, 0.1853354081241826434, -9.240966997248238002 ) ) ;
#16250 = LINE ( 'NONE', #25381, #21560 ) ;
#16251 = ORIENTED_EDGE ( 'NONE', *, *, #3166, .F. ) ;
#16252 = CARTESIAN_POINT ( 'NONE',  ( 20.15412120921589079, -4.773411862323607480, -27.81894205312340063 ) ) ;
#16253 = ORIENTED_EDGE ( 'NONE', *, *, #31938, .T. ) ;
#16254 = CARTESIAN_POINT ( 'NONE',  ( 0.000000000000000000, 0.000000000000000000, 0.000000000000000000 ) ) ;
#16255 = CARTESIAN_POINT ( 'NONE',  ( -14.89626057892329847, 32.60452476689614087, 11.00000000000000000 ) ) ;
#16256 = LINE ( 'NONE', #37389, #30712 ) ;
#16257 = CARTESIAN_POINT ( 'NONE',  ( 6.557822374958316658, 35.99981354310111215, 10.49999999999999822 ) ) ;
#16258 = EDGE_CURVE ( 'NONE', #16887, #32514, #17349, .T. ) ;
#16259 = CARTESIAN_POINT ( 'NONE',  ( 12.55429062395116446, 25.98950339719798563, 18.87996532025784546 ) ) ;
#16260 = CARTESIAN_POINT ( 'NONE',  ( 14.36830325120613594, 20.48707633493483371, 9.000000000000001776 ) ) ;
#16261 = VERTEX_POINT ( 'NONE', #29525 ) ;
#16262 = CARTESIAN_POINT ( 'NONE',  ( -15.94745313500304462, 12.88431841366640640, -30.00000000000001421 ) ) ;
#16263 = CARTESIAN_POINT ( 'NONE',  ( -1.829593030691901284E-15, 22.50000000000001066, 3.000000000000000000 ) ) ;
#16264 = CIRCLE ( 'NONE', #29892, 1.000000000000000888 ) ;
#16265 = CARTESIAN_POINT ( 'NONE',  ( -11.11016527260153808, 31.83082137946488643, 7.000000000000000000 ) ) ;
#16266 = CARTESIAN_POINT ( 'NONE',  ( 17.27189083593461305, 19.38243549486986694, -10.30461736581324672 ) ) ;
#16267 = CARTESIAN_POINT ( 'NONE',  ( 6.781401459173456381, 26.34037369773561821, -17.76491729653662333 ) ) ;
#16268 = ORIENTED_EDGE ( 'NONE', *, *, #6124, .T. ) ;
#16269 = CARTESIAN_POINT ( 'NONE',  ( 15.73177369934751546, -26.14870740989517728, -9.202792353689568827 ) ) ;
#16270 = LINE ( 'NONE', #34558, #19118 ) ;
#16271 = DIRECTION ( 'NONE',  ( 0.000000000000000000, 0.000000000000000000, 1.000000000000000000 ) ) ;
#16272 = ORIENTED_EDGE ( 'NONE', *, *, #6603, .F. ) ;
#16273 = CARTESIAN_POINT ( 'NONE',  ( -14.74173057345504745, 25.38325330337421448, -10.65401870494813430 ) ) ;
#16274 = CIRCLE ( 'NONE', #12388, 20.00000000000003908 ) ;
#16275 = CARTESIAN_POINT ( 'NONE',  ( -25.86085639997994434, -26.44089909996126408, 15.72805884748940031 ) ) ;
#16276 = CARTESIAN_POINT ( 'NONE',  ( 9.892406512096915350, -19.27897539523535286, -23.89377238802892123 ) ) ;
#16277 = CARTESIAN_POINT ( 'NONE',  ( 0.000000000000000000, 22.50000000000000355, 7.000000000000000000 ) ) ;
#16278 = ADVANCED_FACE ( 'NONE', ( #8396 ), #33190, .F. ) ;
#16279 = VERTEX_POINT ( 'NONE', #20792 ) ;
#16280 = ORIENTED_EDGE ( 'NONE', *, *, #35101, .F. ) ;
#16281 = CARTESIAN_POINT ( 'NONE',  ( -10.62610282291096908, 24.67057416925172575, -17.05606316619996221 ) ) ;
#16282 = CARTESIAN_POINT ( 'NONE',  ( -12.53503683000786317, -17.06533638865724711, -25.95590165904247115 ) ) ;
#16283 = CARTESIAN_POINT ( 'NONE',  ( -5.050662510305666153, -26.77689918168226058, 11.00000000000000178 ) ) ;
#16284 = CARTESIAN_POINT ( 'NONE',  ( -25.26715884121037448, -5.457600878228082486, -18.89157672615069572 ) ) ;
#16285 = DIRECTION ( 'NONE',  ( 0.000000000000000000, 0.000000000000000000, -1.000000000000000000 ) ) ;
#16286 = EDGE_LOOP ( 'NONE', ( #38908, #31570, #24032, #36025 ) ) ;
#16287 = CARTESIAN_POINT ( 'NONE',  ( 29.23574345009283704, 0.2107415669908022926, -10.65726852293757254 ) ) ;
#16288 = CARTESIAN_POINT ( 'NONE',  ( 12.93090914525160429, 21.64873284465707926, -17.43820100234846393 ) ) ;
#16289 = CARTESIAN_POINT ( 'NONE',  ( 14.76265446396241110, 21.90695576875680217, 10.49999999999999822 ) ) ;
#16290 = CIRCLE ( 'NONE', #80, 15.00000000000000000 ) ;
#16291 = ORIENTED_EDGE ( 'NONE', *, *, #17852, .F. ) ;
#16292 = CARTESIAN_POINT ( 'NONE',  ( -20.69558676386508722, 0.8167323363481363563, -27.44640420991715146 ) ) ;
#16293 = DIRECTION ( 'NONE',  ( 1.000000000000000000, 0.000000000000000000, 0.000000000000000000 ) ) ;
#16294 = ORIENTED_EDGE ( 'NONE', *, *, #21557, .T. ) ;
#16295 = CARTESIAN_POINT ( 'NONE',  ( 24.07014152680269703, -2.057471556945281943, -20.21244778586666158 ) ) ;
#16296 = LINE ( 'NONE', #28682, #38849 ) ;
#16297 = CARTESIAN_POINT ( 'NONE',  ( 34.38615473478414231, -15.96524117249927954, 16.87380292611441490 ) ) ;
#16298 = ORIENTED_EDGE ( 'NONE', *, *, #9015, .T. ) ;
#16299 = CARTESIAN_POINT ( 'NONE',  ( 11.38745366800453063, 34.53793118711288201, 15.72805884748937011 ) ) ;
#16300 = CARTESIAN_POINT ( 'NONE',  ( -19.26948696230207858, 27.85601271560029701, 23.00000000000000000 ) ) ;
#16301 = ADVANCED_FACE ( 'NONE', ( #1700 ), #32992, .T. ) ;
#16302 = CARTESIAN_POINT ( 'NONE',  ( -4.568463557893644555, 27.32878864566640686, 20.94377226548398241 ) ) ;
#16303 = VECTOR ( 'NONE', #17879, 1000.000000000000000 ) ;
#16304 = DIRECTION ( 'NONE',  ( 0.6691306063588569053, -0.7431448254773954654, 0.000000000000000000 ) ) ;
#16305 = EDGE_CURVE ( 'NONE', #35366, #31091, #29726, .T. ) ;
#16306 = VECTOR ( 'NONE', #27443, 1000.000000000000114 ) ;
#16307 = EDGE_CURVE ( 'NONE', #13873, #4778, #7979, .T. ) ;
#16308 = FACE_OUTER_BOUND ( 'NONE', #21881, .T. ) ;
#16309 = EDGE_CURVE ( 'NONE', #14259, #8510, #1624, .T. ) ;
#16310 = FACE_BOUND ( 'NONE', #11883, .T. ) ;
#16311 = CARTESIAN_POINT ( 'NONE',  ( 30.17922767059877032, -0.7536324250949818504, 17.42190598798392998 ) ) ;
#16312 = CARTESIAN_POINT ( 'NONE',  ( -21.42042906878900865, 9.376721029140135499, -14.90424463124249677 ) ) ;
#16313 = CARTESIAN_POINT ( 'NONE',  ( 13.93925166872112875, -17.41998327387213763, -23.39582284468144024 ) ) ;
#16314 = DIRECTION ( 'NONE',  ( -0.9335804264971965249, 0.3583679495453138131, 0.000000000000000000 ) ) ;
#16315 = VERTEX_POINT ( 'NONE', #14689 ) ;
#16316 = CARTESIAN_POINT ( 'NONE',  ( 10.96769517727479304, 17.57291733725187299, -27.43959740574487327 ) ) ;
#16317 = ORIENTED_EDGE ( 'NONE', *, *, #5023, .F. ) ;
#16318 = CARTESIAN_POINT ( 'NONE',  ( -12.01564447343423048, 17.47318069141996233, -25.10589379291032230 ) ) ;
#16319 = CARTESIAN_POINT ( 'NONE',  ( -23.00727501322622714, -19.64144336131490221, 20.50957957746029336 ) ) ;
#16320 = CARTESIAN_POINT ( 'NONE',  ( 10.81260707898150208, 32.90853150812155548, 10.49999999999999645 ) ) ;
#16321 = CARTESIAN_POINT ( 'NONE',  ( 14.30703310639081849, 24.43075738655355522, -12.55189784990152724 ) ) ;
#16322 = ORIENTED_EDGE ( 'NONE', *, *, #32198, .T. ) ;
#16323 = CARTESIAN_POINT ( 'NONE',  ( 26.88093566382320887, -13.77087523494271792, -15.68169874583660217 ) ) ;
#16324 = CARTESIAN_POINT ( 'NONE',  ( 14.98890121934614506, -28.67928442654198307, -0.000000000000000000 ) ) ;
#16325 = EDGE_CURVE ( 'NONE', #6684, #35424, #22484, .T. ) ;
#16326 = ORIENTED_EDGE ( 'NONE', *, *, #17564, .F. ) ;
#16328 = CYLINDRICAL_SURFACE ( 'NONE', #8867, 1.000000000000000000 ) ;
#16327 = CARTESIAN_POINT ( 'NONE',  ( -11.00125217484130147, 17.88729467479140567, -26.20505879420463913 ) ) ;
#16329 = EDGE_CURVE ( 'NONE', #2814, #18344, #10843, .T. ) ;
#16330 = CARTESIAN_POINT ( 'NONE',  ( -9.820084318045166683, -18.37969044849650757, -26.81932440670792062 ) ) ;
#16331 = CARTESIAN_POINT ( 'NONE',  ( 12.62480652560819472, 14.42233381811226600, 10.49999999999999822 ) ) ;
#16332 = EDGE_CURVE ( 'NONE', #697, #29252, #16027, .T. ) ;
#16333 = CIRCLE ( 'NONE', #19574, 1.000000000000002665 ) ;
#16334 = VERTEX_POINT ( 'NONE', #23631 ) ;
#16335 = CARTESIAN_POINT ( 'NONE',  ( -32.45949353565496409, -15.74491919779192806, -10.17783366908536813 ) ) ;
#16336 = CARTESIAN_POINT ( 'NONE',  ( -14.22070947177296851, -26.40434344209961637, -5.946558550297234902 ) ) ;
#16337 = CARTESIAN_POINT ( 'NONE',  ( 3.863783140547853712E-14, -86.77689918168233874, 0.000000000000000000 ) ) ;
#16338 = CARTESIAN_POINT ( 'NONE',  ( 16.49060731112116684, 23.31193391774742807, -5.474701027004573284 ) ) ;
#16339 = EDGE_LOOP ( 'NONE', ( #17311, #38210, #34760 ) ) ;
#16340 = CARTESIAN_POINT ( 'NONE',  ( 27.23700843456267151, 3.778717822207238175, -7.382781898693922429 ) ) ;
#16341 = CARTESIAN_POINT ( 'NONE',  ( 13.24038105676655164, 15.43301270189216368, 10.49999999999999822 ) ) ;
#16342 = DIRECTION ( 'NONE',  ( 0.000000000000000000, 0.000000000000000000, -1.000000000000000000 ) ) ;
#16343 = ORIENTED_EDGE ( 'NONE', *, *, #37701, .F. ) ;
#16344 = CARTESIAN_POINT ( 'NONE',  ( -23.44040957046583173, 0.2069204251881845147, -20.49466620512498238 ) ) ;
#16345 = CARTESIAN_POINT ( 'NONE',  ( 27.32033147505850224, -0.01464922774640640794, -14.44792093758196749 ) ) ;
#16346 = CARTESIAN_POINT ( 'NONE',  ( 23.94831201522132602, -21.88372720616970923, 19.66345542862529783 ) ) ;
#16347 = EDGE_LOOP ( 'NONE', ( #5804, #39811, #21048, #13292 ) ) ;
#16348 = AXIS2_PLACEMENT_3D ( 'NONE', #16907, #111, #10197 ) ;
#16349 = CARTESIAN_POINT ( 'NONE',  ( 11.41987377193677489, -19.41918266173338026, -20.90349153980996988 ) ) ;
#16350 = EDGE_CURVE ( 'NONE', #38194, #25405, #32896, .T. ) ;
#16351 = DIRECTION ( 'NONE',  ( 1.000000000000000000, 0.000000000000000000, 0.000000000000000000 ) ) ;
#16352 = EDGE_CURVE ( 'NONE', #1614, #2419, #20594, .T. ) ;
#16353 = ADVANCED_FACE ( 'NONE', ( #29923 ), #2104, .T. ) ;
#16354 = ORIENTED_EDGE ( 'NONE', *, *, #13240, .T. ) ;
#16355 = CYLINDRICAL_SURFACE ( 'NONE', #17173, 1.000000000000000888 ) ;
#16356 = DIRECTION ( 'NONE',  ( 0.000000000000000000, 0.000000000000000000, -1.000000000000000000 ) ) ;
#16357 = LINE ( 'NONE', #38084, #34595 ) ;
#16358 = AXIS2_PLACEMENT_3D ( 'NONE', #32369, #26660, #17134 ) ;
#16359 = CARTESIAN_POINT ( 'NONE',  ( 14.60301432615392514, 21.46791548645758141, 11.00000000000000178 ) ) ;
#16360 = VERTEX_POINT ( 'NONE', #20985 ) ;
#16361 = CARTESIAN_POINT ( 'NONE',  ( 12.03571151536236528, 31.45218678977230908, 7.000000000000000000 ) ) ;
#16362 = FACE_OUTER_BOUND ( 'NONE', #36499, .T. ) ;
#16363 = CARTESIAN_POINT ( 'NONE',  ( 23.96003644509144337, -20.87731938338408000, -13.86997135298250505 ) ) ;
#16364 = CARTESIAN_POINT ( 'NONE',  ( 14.62786683182123859, 20.45979510329145157, 10.94611345180490503 ) ) ;
#16365 = CARTESIAN_POINT ( 'NONE',  ( 1.000000000000000000, 37.50000000000000711, 11.00000000000000000 ) ) ;
#16366 = CARTESIAN_POINT ( 'NONE',  ( 14.73628306789068887, 26.39990037738499851, -9.676459069332137730 ) ) ;
#16367 = CARTESIAN_POINT ( 'NONE',  ( -5.064571727552472424, 31.45661825943146894, 6.000000000000000000 ) ) ;
#16368 = ORIENTED_EDGE ( 'NONE', *, *, #17692, .F. ) ;
#16370 = FACE_OUTER_BOUND ( 'NONE', #9504, .T. ) ;
#16369 = CARTESIAN_POINT ( 'NONE',  ( -15.13822083024485465, 15.68883449183921108, -22.06930914276376399 ) ) ;
#16371 = CARTESIAN_POINT ( 'NONE',  ( 13.23567246089205618, 15.94827353676168613, 10.49999999999999822 ) ) ;
#16372 = CIRCLE ( 'NONE', #30679, 1.000000000000000888 ) ;
#16373 = CARTESIAN_POINT ( 'NONE',  ( 14.83864103363871934, -25.82583482475954995, -9.709532566869290449 ) ) ;
#16374 = CARTESIAN_POINT ( 'NONE',  ( 14.36830325120613239, 20.48707633493482660, 11.00000000000000000 ) ) ;
#16375 = CARTESIAN_POINT ( 'NONE',  ( 15.40441473722033372, 26.73208805529019827, -5.946081656235632451 ) ) ;
#16376 = ORIENTED_EDGE ( 'NONE', *, *, #37498, .T. ) ;
#16377 = CARTESIAN_POINT ( 'NONE',  ( 14.53140152873310775, 24.97328356840171182, -11.59890379914568115 ) ) ;
#16378 = ORIENTED_EDGE ( 'NONE', *, *, #3168, .T. ) ;
#16380 = FACE_OUTER_BOUND ( 'NONE', #34153, .T. ) ;
#16379 = CARTESIAN_POINT ( 'NONE',  ( -13.98917752177664475, 24.03416810030780937, -13.50391462411186438 ) ) ;
#16381 = CARTESIAN_POINT ( 'NONE',  ( -10.52525848093844196, -19.57894633451951805, -22.73643589974196999 ) ) ;
#16382 = CARTESIAN_POINT ( 'NONE',  ( -16.95459465864602677, -28.62006465032632363, 13.92931973827769987 ) ) ;
#16383 = ADVANCED_FACE ( 'NONE', ( #24029 ), #36424, .F. ) ;
#16384 = VECTOR ( 'NONE', #25367, 1000.000000000000000 ) ;
#16385 = CARTESIAN_POINT ( 'NONE',  ( -30.57778148685732944, -22.50129585022499867, -6.703186603742934402 ) ) ;
#16386 = CARTESIAN_POINT ( 'NONE',  ( -4.617270946191116998, -24.33986194121566271, -10.36143787604604682 ) ) ;
#16387 = CARTESIAN_POINT ( 'NONE',  ( 15.52679059097398273, 25.14300703315133134, -8.306665296563053857 ) ) ;
#16388 = ORIENTED_EDGE ( 'NONE', *, *, #30757, .T. ) ;
#16389 = CARTESIAN_POINT ( 'NONE',  ( 21.94669886647698220, 10.98376864938533082, -8.898427312023766689 ) ) ;
#16390 = CARTESIAN_POINT ( 'NONE',  ( -13.82587227205766389, 37.11292025503280456, 11.00000000000000000 ) ) ;
#16391 = CARTESIAN_POINT ( 'NONE',  ( -1.681518492368433426, 38.03812643383474779, 16.87380292611441135 ) ) ;
#16392 = EDGE_LOOP ( 'NONE', ( #22557, #25631, #33870, #19682, #35178 ) ) ;
#16393 = CARTESIAN_POINT ( 'NONE',  ( -21.45859226520986951, -2.583396648404852503, -24.66285604314880686 ) ) ;
#16394 = CARTESIAN_POINT ( 'NONE',  ( -13.31403195207871981, 20.45929608442119729, 19.27171037444204060 ) ) ;
#16395 = ORIENTED_EDGE ( 'NONE', *, *, #22788, .F. ) ;
#16396 = DIRECTION ( 'NONE',  ( -1.000000000000000000, 0.000000000000000000, 0.000000000000000000 ) ) ;
#16397 = DIRECTION ( 'NONE',  ( 1.000000000000000000, 0.000000000000000000, -0.000000000000000000 ) ) ;
#16398 = CARTESIAN_POINT ( 'NONE',  ( 19.09187170439694725, -7.719518535268413473, -28.46272815273926682 ) ) ;
#16399 = CARTESIAN_POINT ( 'NONE',  ( 31.34430980808824430, -24.70897660846287636, 12.14047268033096927 ) ) ;
#16400 = EDGE_CURVE ( 'NONE', #22349, #13390, #21221, .T. ) ;
#16401 = EDGE_LOOP ( 'NONE', ( #13826, #13742 ) ) ;
#16402 = AXIS2_PLACEMENT_3D ( 'NONE', #25580, #22137, #25784 ) ;
#16403 = ORIENTED_EDGE ( 'NONE', *, *, #10340, .F. ) ;
#16404 = CARTESIAN_POINT ( 'NONE',  ( 11.11016527260166420, 31.83082137946473367, 9.000000000000001776 ) ) ;
#16405 = CARTESIAN_POINT ( 'NONE',  ( -19.07667540522614047, 16.81475038866948069, -5.000000000000000000 ) ) ;
#16406 = AXIS2_PLACEMENT_3D ( 'NONE', #25276, #37669, #13072 ) ;
#16407 = LINE ( 'NONE', #1170, #1956 ) ;
#16408 = ORIENTED_EDGE ( 'NONE', *, *, #38128, .T. ) ;
#16409 = CARTESIAN_POINT ( 'NONE',  ( -0.4436405235953277959, 22.83777681550889582, -22.98300611285952755 ) ) ;
#16410 = DIRECTION ( 'NONE',  ( 0.9781476007338070211, 0.2079116908177534029, -0.000000000000000000 ) ) ;
#16411 = DIRECTION ( 'NONE',  ( 0.3090169943749573878, 0.9510565162951503115, 0.000000000000000000 ) ) ;
#16412 = CARTESIAN_POINT ( 'NONE',  ( 8.472151273871505239, 28.78272654129060371, 10.50000000000000000 ) ) ;
#16413 = FACE_OUTER_BOUND ( 'NONE', #5296, .T. ) ;
#16414 = VECTOR ( 'NONE', #21461, 999.9999999999998863 ) ;
#16415 = DIRECTION ( 'NONE',  ( 0.000000000000000000, -0.5821182788257928120, 0.8131041196900287149 ) ) ;
#16416 = CARTESIAN_POINT ( 'NONE',  ( 14.16561412993485014, 28.57187406534849927, -8.667803205440176129 ) ) ;
#16417 = CARTESIAN_POINT ( 'NONE',  ( 2.363107919609636731, 7.722275577008987035, 10.49999999999999822 ) ) ;
#16418 = ORIENTED_EDGE ( 'NONE', *, *, #35361, .F. ) ;
#16420 = CARTESIAN_POINT ( 'NONE',  ( -10.70158575030358072, 30.79011836036732674, 9.500000000000000000 ) ) ;
#16419 = CARTESIAN_POINT ( 'NONE',  ( -18.58854498669193944, 12.12440799916769940, -19.06110518814004706 ) ) ;
#16421 = DIRECTION ( 'NONE',  ( 1.000000000000000000, 0.000000000000000000, 0.000000000000000000 ) ) ;
#16422 = CARTESIAN_POINT ( 'NONE',  ( 15.37591282558991601, -26.51818385147999635, -7.356517339422841140 ) ) ;
#16423 = FACE_OUTER_BOUND ( 'NONE', #10747, .T. ) ;
#16424 = CARTESIAN_POINT ( 'NONE',  ( 15.39755691330850951, 26.84919286949167017, -5.473884989333777540 ) ) ;
#16425 = CARTESIAN_POINT ( 'NONE',  ( 6.023418944065110914, 39.81932404830325112, -14.45070082761206365 ) ) ;
#16426 = LINE ( 'NONE', #25761, #28397 ) ;
#16427 = AXIS2_PLACEMENT_3D ( 'NONE', #16809, #13745, #4406 ) ;
#16428 = CARTESIAN_POINT ( 'NONE',  ( -16.56729576810697324, -17.53405923247618858, -20.95322699904796693 ) ) ;
#16429 = CARTESIAN_POINT ( 'NONE',  ( 8.251618643569010203, -24.83515768495495379, -9.332969128487192734 ) ) ;
#16430 = CARTESIAN_POINT ( 'NONE',  ( 15.00280477620397512, 25.59022088404001138, -9.712201262136385793 ) ) ;
#16431 = CARTESIAN_POINT ( 'NONE',  ( 29.94381607632180220, -21.64440053025225552, -8.853049120304181230 ) ) ;
#16432 = ADVANCED_FACE ( 'NONE', ( #6673 ), #25249, .T. ) ;
#16433 = AXIS2_PLACEMENT_3D ( 'NONE', #38261, #16735, #25452 ) ;
#16434 = DIRECTION ( 'NONE',  ( -0.000000000000000000, -0.000000000000000000, -1.000000000000000000 ) ) ;
#16435 = DIRECTION ( 'NONE',  ( 1.000000000000000000, -1.734723475976805319E-15, 0.000000000000000000 ) ) ;
#16436 = ORIENTED_EDGE ( 'NONE', *, *, #8273, .F. ) ;
#16437 = CARTESIAN_POINT ( 'NONE',  ( -5.802259185096063199, 21.80286457058984340, -23.19183301011633347 ) ) ;
#16438 = VECTOR ( 'NONE', #23464, 1000.000000000000000 ) ;
#16439 = CARTESIAN_POINT ( 'NONE',  ( 14.66026487122505451, 21.46189821169926759, 10.96580508970281542 ) ) ;
#16440 = ORIENTED_EDGE ( 'NONE', *, *, #15801, .F. ) ;
#16441 = CARTESIAN_POINT ( 'NONE',  ( 21.28174780547579914, 0.7376432744340452041, -25.01040352120890020 ) ) ;
#16442 = EDGE_CURVE ( 'NONE', #29890, #39914, #33562, .T. ) ;
#16443 = DIRECTION ( 'NONE',  ( 1.000000000000000000, 0.000000000000000000, 0.000000000000000000 ) ) ;
#16444 = CARTESIAN_POINT ( 'NONE',  ( -23.61737546510164165, -7.194424252576709478, 20.99999999999999645 ) ) ;
#16445 = ADVANCED_FACE ( 'NONE', ( #25175 ), #31090, .T. ) ;
#16446 = VERTEX_POINT ( 'NONE', #34719 ) ;
#16447 = CARTESIAN_POINT ( 'NONE',  ( -30.75812384186223625, 0.07155913731190695348, -5.946101298864587825 ) ) ;
#16448 = CARTESIAN_POINT ( 'NONE',  ( -19.54254079969926750, -25.96847085201792282, -9.956545144438887718 ) ) ;
#16449 = AXIS2_PLACEMENT_3D ( 'NONE', #5178, #38905, #2136 ) ;
#16450 = ORIENTED_EDGE ( 'NONE', *, *, #34335, .T. ) ;
#16451 = CARTESIAN_POINT ( 'NONE',  ( 34.72648361517081383, -9.366762812312714459, -8.036555274816278072 ) ) ;
#16452 = AXIS2_PLACEMENT_3D ( 'NONE', #33470, #36705, #27947 ) ;
#16453 = VERTEX_POINT ( 'NONE', #11838 ) ;
#16454 = CARTESIAN_POINT ( 'NONE',  ( 0.000000000000000000, 0.000000000000000000, 0.000000000000000000 ) ) ;
#16455 = CARTESIAN_POINT ( 'NONE',  ( -12.39897218486444963, 35.60749793648266603, 12.14047268033129257 ) ) ;
#16456 = CARTESIAN_POINT ( 'NONE',  ( 3.476901250629512941, 26.36149378532653031, 12.00000000000000000 ) ) ;
#16457 = CARTESIAN_POINT ( 'NONE',  ( -3.996141029131407230, 8.041929616041358031, 7.381627713044569106 ) ) ;
#16458 = CARTESIAN_POINT ( 'NONE',  ( 3.681484855442201720, 33.42880943655697479, 19.66345542862528717 ) ) ;
#16459 = AXIS2_PLACEMENT_3D ( 'NONE', #20477, #26153, #25948 ) ;
#16460 = CARTESIAN_POINT ( 'NONE',  ( -11.44473057578096764, 31.45924896672619298, 10.49999999999999822 ) ) ;
#16461 = EDGE_LOOP ( 'NONE', ( #12645, #26156, #18657, #4073 ) ) ;
#16462 = SURFACE_STYLE_FILL_AREA ( #38195 ) ;
#16463 = CARTESIAN_POINT ( 'NONE',  ( -11.90291963069949155, 16.69351461089588540, -29.99999999999999289 ) ) ;
#16464 = PRESENTATION_LAYER_ASSIGNMENT (  '', '', ( #34607 ) ) ;
#16465 = DIRECTION ( 'NONE',  ( 1.000000000000000000, 0.000000000000000000, 0.000000000000000000 ) ) ;
#16466 = EDGE_CURVE ( 'NONE', #15571, #26406, #3635, .T. ) ;
#16467 = DIRECTION ( 'NONE',  ( -0.000000000000000000, -0.000000000000000000, -1.000000000000000000 ) ) ;
#16468 = CARTESIAN_POINT ( 'NONE',  ( 16.70512624272670976, 16.98008137324713118, -15.81966299108973573 ) ) ;
#16469 = CARTESIAN_POINT ( 'NONE',  ( 7.632467833249850564, 23.73579192844700714, -19.92015518565826326 ) ) ;
#16470 = CIRCLE ( 'NONE', #39174, 1.000000000000000000 ) ;
#16471 = ORIENTED_EDGE ( 'NONE', *, *, #30493, .F. ) ;
#16472 = CARTESIAN_POINT ( 'NONE',  ( -11.77091082532341204, 29.60251629318183575, 13.00000000000000178 ) ) ;
#16473 = CARTESIAN_POINT ( 'NONE',  ( 12.28607510256881241, -20.87432611439488639, -19.40397933997828872 ) ) ;
#16474 = DIRECTION ( 'NONE',  ( 0.8090169943749426773, -0.5877852522924797984, 0.000000000000000000 ) ) ;
#16475 = DIRECTION ( 'NONE',  ( 0.7431448254773954654, 0.6691306063588569053, -0.000000000000000000 ) ) ;
#16476 = EDGE_LOOP ( 'NONE', ( #22077, #4663, #1331, #26554 ) ) ;
#16477 = CARTESIAN_POINT ( 'NONE',  ( -13.22195404768716642, 22.21339375608201294, -16.44601427550475847 ) ) ;
#16478 = VECTOR ( 'NONE', #3956, 1000.000000000000000 ) ;
#16479 = CARTESIAN_POINT ( 'NONE',  ( -30.90861030616400029, -0.03770625498372660866, 16.30093088680191116 ) ) ;
#16480 = CARTESIAN_POINT ( 'NONE',  ( 13.33431249370194926, -24.07337194581927164, -13.53033386366181468 ) ) ;
#16481 = CARTESIAN_POINT ( 'NONE',  ( -7.935100905948476502, 11.57827057593827469, 7.000000000000000000 ) ) ;
#16482 = ORIENTED_EDGE ( 'NONE', *, *, #32983, .T. ) ;
#16483 = ORIENTED_EDGE ( 'NONE', *, *, #28867, .F. ) ;
#16484 = CARTESIAN_POINT ( 'NONE',  ( -12.64192529757091954, 32.30851842349025560, -5.897544463971819084 ) ) ;
#16485 = CARTESIAN_POINT ( 'NONE',  ( 2.229431105722923245, 20.49260818092372460, 13.00000000000000178 ) ) ;
#16486 = EDGE_CURVE ( 'NONE', #31354, #23547, #17712, .T. ) ;
#16487 = FACE_BOUND ( 'NONE', #8452, .T. ) ;
#16488 = AXIS2_PLACEMENT_3D ( 'NONE', #21168, #28055, #15468 ) ;
#16489 = CARTESIAN_POINT ( 'NONE',  ( -20.11683937074663930, -4.305318936261572915, -28.53642093606467967 ) ) ;
#16490 = CARTESIAN_POINT ( 'NONE',  ( -5.473344025737326035, 14.11593743010433677, 10.50000000000000355 ) ) ;
#16491 = EDGE_LOOP ( 'NONE', ( #5112, #10751 ) ) ;
#16492 = CIRCLE ( 'NONE', #19002, 1.000000000000000888 ) ;
#16493 = CARTESIAN_POINT ( 'NONE',  ( 29.67767680329217939, 0.1815030806635676563, -9.711878978317606936 ) ) ;
#16494 = CARTESIAN_POINT ( 'NONE',  ( 15.41558956984165363, 26.78481017248027740, -5.000000000000000000 ) ) ;
#16495 = DIRECTION ( 'NONE',  ( -0.000000000000000000, -0.000000000000000000, -1.000000000000000000 ) ) ;
#16496 = ADVANCED_FACE ( 'NONE', ( #24426 ), #8991, .F. ) ;
#16497 = VERTEX_POINT ( 'NONE', #26375 ) ;
#16498 = CARTESIAN_POINT ( 'NONE',  ( -20.69415337481283501, 0.8377244533787358005, -27.44776534124708434 ) ) ;
#16499 = CARTESIAN_POINT ( 'NONE',  ( -1.278175571584109660, 14.08178954835378427, 9.000000000000001776 ) ) ;
#16500 = EDGE_LOOP ( 'NONE', ( #13037, #5830, #16664, #25233 ) ) ;
#16501 = CARTESIAN_POINT ( 'NONE',  ( 25.36917227601168889, -1.505153948585238322, -18.21253142723226759 ) ) ;
#16502 = AXIS2_PLACEMENT_3D ( 'NONE', #26141, #23096, #7658 ) ;
#16503 = DIRECTION ( 'NONE',  ( 1.000000000000000000, 0.000000000000000000, 0.000000000000000000 ) ) ;
#16504 = CARTESIAN_POINT ( 'NONE',  ( 24.21699896819641040, -27.13078975446658703, 15.72805884748975558 ) ) ;
#16505 = VERTEX_POINT ( 'NONE', #26173 ) ;
#16506 = CARTESIAN_POINT ( 'NONE',  ( 13.63376536442992837, 31.74814110635675846, 15.72805884748940031 ) ) ;
#16507 = DIRECTION ( 'NONE',  ( -0.9945218953682742891, -0.1045284632676437425, 0.000000000000000000 ) ) ;
#16508 = CARTESIAN_POINT ( 'NONE',  ( -6.175735745372779917, 24.95935742585754014, 20.94377226548369109 ) ) ;
#16509 = CIRCLE ( 'NONE', #3510, 1.000000000000004441 ) ;
#16510 = FACE_OUTER_BOUND ( 'NONE', #35025, .T. ) ;
#16511 = ADVANCED_FACE ( 'NONE', ( #38770 ), #17046, .F. ) ;
#16512 = DIRECTION ( 'NONE',  ( 0.000000000000000000, 0.000000000000000000, 1.000000000000000000 ) ) ;
#16513 = EDGE_CURVE ( 'NONE', #39537, #15233, #7691, .T. ) ;
#16514 = PRODUCT_DEFINITION_SHAPE ( 'NONE', 'NONE',  #40206 ) ;
#16515 = CIRCLE ( 'NONE', #32738, 0.5000000000000015543 ) ;
#16516 = CARTESIAN_POINT ( 'NONE',  ( 4.211395437248501850, 12.61633075744433796, 12.00000000000000000 ) ) ;
#16517 = CARTESIAN_POINT ( 'NONE',  ( 26.89145897429045107, 3.386615419904837498, 16.87380292612509436 ) ) ;
#16518 = CARTESIAN_POINT ( 'NONE',  ( -23.46155114344813342, 8.928999627652238757, -7.419147749525820679 ) ) ;
#16519 = CARTESIAN_POINT ( 'NONE',  ( 17.65433335263828596, -21.92020081565964418, -16.00066446180797186 ) ) ;
#16520 = DIRECTION ( 'NONE',  ( 1.000000000000000000, 1.224646799147351235E-16, -0.000000000000000000 ) ) ;
#16521 = CARTESIAN_POINT ( 'NONE',  ( 15.36061443993781062, 26.97785078317152596, -5.473250886727928588 ) ) ;
#16522 = VERTEX_POINT ( 'NONE', #13578 ) ;
#16523 = AXIS2_PLACEMENT_3D ( 'NONE', #34155, #5715, #15662 ) ;
#16524 = CARTESIAN_POINT ( 'NONE',  ( -15.84332410282777559, 25.22439668510312316, -5.946718473460527399 ) ) ;
#16525 = CARTESIAN_POINT ( 'NONE',  ( -30.09689698601766850, -15.93509466225727422, 19.66345542862561757 ) ) ;
#16526 = CARTESIAN_POINT ( 'NONE',  ( 10.81260707898162821, 32.90853150812142047, 10.59344459855564047 ) ) ;
#16527 = CARTESIAN_POINT ( 'NONE',  ( 15.44688523099049959, 26.67261462138580441, -5.474175438101869240 ) ) ;
#16528 = VERTEX_POINT ( 'NONE', #17252 ) ;
#16529 = CARTESIAN_POINT ( 'NONE',  ( 30.67527980673472143, -15.70519271476555190, -11.97612696850552716 ) ) ;
#16530 = CARTESIAN_POINT ( 'NONE',  ( 14.47283171447379502, 21.48159823030311344, 9.000000000000001776 ) ) ;
#16531 = EDGE_LOOP ( 'NONE', ( #33793, #25882, #20033, #25029 ) ) ;
#16533 = CARTESIAN_POINT ( 'NONE',  ( -14.47283171447380390, 21.48159823030330529, 11.00000000000000000 ) ) ;
#16532 = CARTESIAN_POINT ( 'NONE',  ( -10.81748158546086280, 17.46796835832452288, -28.69910257507550000 ) ) ;
#16534 = CARTESIAN_POINT ( 'NONE',  ( -16.41154929109325877, -26.54183177608878808, -8.252701314873407412 ) ) ;
#16535 = EDGE_CURVE ( 'NONE', #20904, #1089, #39375, .T. ) ;
#16536 = CARTESIAN_POINT ( 'NONE',  ( 3.458865582155095986, 18.48521636184714012, 6.000000000000000000 ) ) ;
#16537 = VERTEX_POINT ( 'NONE', #1395 ) ;
#16538 = CARTESIAN_POINT ( 'NONE',  ( -19.01480660951762403, -7.883819887955906935, -28.46126324442468558 ) ) ;
#16539 = CARTESIAN_POINT ( 'NONE',  ( -13.86090271882461522, -25.47782269314085823, -10.19673432174426786 ) ) ;
#16540 = FACE_OUTER_BOUND ( 'NONE', #7544, .T. ) ;
#16541 = CARTESIAN_POINT ( 'NONE',  ( 12.66487866387964978, 16.11973886863585648, -29.38096022884959879 ) ) ;
#16542 = ORIENTED_EDGE ( 'NONE', *, *, #21166, .F. ) ;
#16543 = CARTESIAN_POINT ( 'NONE',  ( 21.35709708808257901, 3.778198925977738210, -23.05548261300866741 ) ) ;
#16544 = FACE_OUTER_BOUND ( 'NONE', #24680, .T. ) ;
#16545 = CARTESIAN_POINT ( 'NONE',  ( -14.44277748876676881, 26.55045409923033972, 7.499999999999993783 ) ) ;
#16546 = B_SPLINE_CURVE_WITH_KNOTS ( 'NONE', 3,
 ( #38999, #33119, #11969, #24360, #36757, #21317, #33723, #11172, #23564, #35959, #5469, #20522, #32916, #2430, #5075, #39392, #17684, #29853 ),
 .UNSPECIFIED., .F., .F.,
 ( 4, 2, 2, 2, 2, 2, 2, 2, 4 ),
 ( 0.000000000000000000, 0.1250000000000000000, 0.2500000000000000000, 0.3750000000000000000, 0.5000000000000000000, 0.6250000000000000000, 0.7500000000000000000, 0.8750000000000000000, 1.000000000000000000 ),
 .UNSPECIFIED. ) ;
#16547 = ORIENTED_EDGE ( 'NONE', *, *, #15991, .T. ) ;
#16548 = CARTESIAN_POINT ( 'NONE',  ( -28.56343558534357996, -0.1369546348107109623, -12.52232705135813262 ) ) ;
#16549 = VECTOR ( 'NONE', #16689, 1000.000000000000000 ) ;
#16550 = CARTESIAN_POINT ( 'NONE',  ( 31.48691846961225593, -0.7858779617076784296, -6.401761492272640908 ) ) ;
#16551 = CARTESIAN_POINT ( 'NONE',  ( 20.20329687195648560, -21.14155277498772278, 20.25080042701565830 ) ) ;
#16552 = EDGE_LOOP ( 'NONE', ( #32863, #36815, #22860, #25352 ) ) ;
#16553 = VECTOR ( 'NONE', #7006, 1000.000000000000000 ) ;
#16554 = CARTESIAN_POINT ( 'NONE',  ( -20.90924525106831666, -8.502318254486386451, -19.80438750953543803 ) ) ;
#16555 = DIRECTION ( 'NONE',  ( 0.000000000000000000, 0.000000000000000000, 1.000000000000000000 ) ) ;
#16556 = VECTOR ( 'NONE', #2182, 999.9999999999998863 ) ;
#16557 = VECTOR ( 'NONE', #25864, 1000.000000000000000 ) ;
#16558 = LINE ( 'NONE', #7195, #29081 ) ;
#16559 = CARTESIAN_POINT ( 'NONE',  ( 13.48130249190479191, 27.93180293473185927, 7.000000000000000000 ) ) ;
#16560 = EDGE_CURVE ( 'NONE', #33408, #37025, #27055, .T. ) ;
#16561 = CARTESIAN_POINT ( 'NONE',  ( 5.187504188494417079, 36.60991850771481637, 10.49999999999999467 ) ) ;
#16562 = DIRECTION ( 'NONE',  ( 0.000000000000000000, 0.000000000000000000, -1.000000000000000000 ) ) ;
#16563 = CARTESIAN_POINT ( 'NONE',  ( 12.01837422881150275, 21.26636931122159169, 13.00000000000000178 ) ) ;
#16564 = ORIENTED_EDGE ( 'NONE', *, *, #15247, .T. ) ;
#16565 = CYLINDRICAL_SURFACE ( 'NONE', #9784, 1.000000000000000888 ) ;
#16566 = LINE ( 'NONE', #1938, #13583 ) ;
#16567 = CARTESIAN_POINT ( 'NONE',  ( 27.13643189954879631, -23.62865347416715522, -9.322685417528527196 ) ) ;
#16568 = CARTESIAN_POINT ( 'NONE',  ( -22.37674264578614469, 24.85189042352228839, 7.000000000000000000 ) ) ;
#16569 = CARTESIAN_POINT ( 'NONE',  ( 9.331903152615748098, 11.35703883385568780, 7.500000000000000888 ) ) ;
#16570 = B_SPLINE_CURVE_WITH_KNOTS ( 'NONE', 3,
 ( #29185, #4801, #13535, #37574, #35884, #1761, #1152, #7434 ),
 .UNSPECIFIED., .F., .F.,
 ( 4, 2, 2, 4 ),
 ( 0.000000000000000000, 0.0004726692273637163929, 0.0007090038410455775167, 0.0009453384547274386405 ),
 .UNSPECIFIED. ) ;
#16571 = AXIS2_PLACEMENT_3D ( 'NONE', #20936, #17704, #29676 ) ;
#16572 = CARTESIAN_POINT ( 'NONE',  ( 13.24833755792088397, 23.29711900540358016, -15.39597941112752899 ) ) ;
#16573 = DIRECTION ( 'NONE',  ( -0.6691306063588671194, -0.7431448254773863615, 0.000000000000000000 ) ) ;
#16574 = ORIENTED_EDGE ( 'NONE', *, *, #18184, .F. ) ;
#16575 = CARTESIAN_POINT ( 'NONE',  ( -17.39674132288666897, 19.08569459991767658, -10.31070539419228993 ) ) ;
#16576 = CARTESIAN_POINT ( 'NONE',  ( -25.03753813966994102, -13.00734255224434577, 20.99999999999999645 ) ) ;
#16577 = CARTESIAN_POINT ( 'NONE',  ( 12.26911082574471479, -22.02329771041612716, -17.43940135948574621 ) ) ;
#16578 = CARTESIAN_POINT ( 'NONE',  ( 7.713869163865849643, 10.18146832927074996, 11.00000000000000000 ) ) ;
#16579 = CARTESIAN_POINT ( 'NONE',  ( 11.18323034263226035, 17.75715498309750728, -26.22476241273409059 ) ) ;
#16580 = ORIENTED_EDGE ( 'NONE', *, *, #5799, .F. ) ;
#16581 = CARTESIAN_POINT ( 'NONE',  ( 11.03438618020454065, 17.42870394567875181, -28.07707603705586052 ) ) ;
#16582 = EDGE_LOOP ( 'NONE', ( #29837, #17138, #30579, #39397 ) ) ;
#16583 = VECTOR ( 'NONE', #29566, 1000.000000000000000 ) ;
#16585 = CARTESIAN_POINT ( 'NONE',  ( 13.94482798346721175, 26.50521816028912525, 10.99999999999999289 ) ) ;
#16584 = CARTESIAN_POINT ( 'NONE',  ( -10.95814459664155294, 17.32538844660855659, -29.34778725072792938 ) ) ;
#16586 = CARTESIAN_POINT ( 'NONE',  ( -13.37288965632171056, -23.62230190449336931, -14.47666671991737708 ) ) ;
#16587 = EDGE_CURVE ( 'NONE', #3128, #9203, #16642, .T. ) ;
#16588 = CARTESIAN_POINT ( 'NONE',  ( -34.90171719354061253, -20.15051581687081139, 12.73282698324853079 ) ) ;
#16589 = CARTESIAN_POINT ( 'NONE',  ( -17.09558480960348703, -11.76928779124230928, -27.71295030018220018 ) ) ;
#16590 = CARTESIAN_POINT ( 'NONE',  ( -7.011761754585625006, -25.08926108585034243, -6.920918333007429091 ) ) ;
#16591 = CARTESIAN_POINT ( 'NONE',  ( 15.45857095869342146, 25.00809084266443350, -8.779209621340882563 ) ) ;
#16593 = EDGE_CURVE ( 'NONE', #31286, #4629, #25096, .T. ) ;
#16592 = ORIENTED_EDGE ( 'NONE', *, *, #27775, .F. ) ;
#16594 = CARTESIAN_POINT ( 'NONE',  ( 19.41139689652032274, 8.139058158844877156, -24.38516366816878289 ) ) ;
#16595 = DIRECTION ( 'NONE',  ( 0.000000000000000000, 0.000000000000000000, 1.000000000000000000 ) ) ;
#16596 = DIRECTION ( 'NONE',  ( -0.000000000000000000, -0.000000000000000000, -1.000000000000000000 ) ) ;
#16597 = CARTESIAN_POINT ( 'NONE',  ( 7.775297188276389271, 35.41132985342715500, 17.42190598798394063 ) ) ;
#16598 = VERTEX_POINT ( 'NONE', #7274 ) ;
#16599 = CARTESIAN_POINT ( 'NONE',  ( -25.03457601920170106, -3.132625777938056633, -19.07791454636011252 ) ) ;
#16600 = EDGE_CURVE ( 'NONE', #3128, #34232, #35521, .T. ) ;
#16601 = CYLINDRICAL_SURFACE ( 'NONE', #38410, 0.5000000000000002220 ) ;
#16602 = ORIENTED_EDGE ( 'NONE', *, *, #18565, .T. ) ;
#16603 = CARTESIAN_POINT ( 'NONE',  ( 23.54493052986456547, -14.21898406159490413, 20.99999999999999645 ) ) ;
#16604 = LINE ( 'NONE', #22681, #36221 ) ;
#16605 = CARTESIAN_POINT ( 'NONE',  ( 33.21478130368457471, -15.74274012923293498, -9.287806114988983452 ) ) ;
#16606 = CARTESIAN_POINT ( 'NONE',  ( 34.66557409316544636, -1.755032161644171085, 12.73282698324864803 ) ) ;
#16607 = ORIENTED_EDGE ( 'NONE', *, *, #16800, .T. ) ;
#16608 = ORIENTED_EDGE ( 'NONE', *, *, #39999, .T. ) ;
#16609 = DIRECTION ( 'NONE',  ( 0.000000000000000000, 0.000000000000000000, 1.000000000000000000 ) ) ;
#16610 = AXIS2_PLACEMENT_3D ( 'NONE', #33437, #17990, #30378 ) ;
#16611 = FACE_OUTER_BOUND ( 'NONE', #32335, .T. ) ;
#16612 = EDGE_CURVE ( 'NONE', #34166, #15690, #4238, .T. ) ;
#16613 = EDGE_CURVE ( 'NONE', #33185, #22962, #14186, .T. ) ;
#16614 = AXIS2_PLACEMENT_3D ( 'NONE', #37753, #3821, #34907 ) ;
#16615 = VECTOR ( 'NONE', #9491, 1000.000000000000000 ) ;
#16616 = DIRECTION ( 'NONE',  ( -8.659560562354955045E-17, 0.7071067811865489050, -0.7071067811865462405 ) ) ;
#16617 = ORIENTED_EDGE ( 'NONE', *, *, #4457, .T. ) ;
#16618 = CARTESIAN_POINT ( 'NONE',  ( -0.3972110264143895453, 20.50537081352338475, -29.21185317353639022 ) ) ;
#16619 = CYLINDRICAL_SURFACE ( 'NONE', #36020, 1.000000000000000000 ) ;
#16620 = VECTOR ( 'NONE', #23722, 1000.000000000000000 ) ;
#16621 = CARTESIAN_POINT ( 'NONE',  ( 12.67417846324118180, 14.47720745114811258, 7.000000000000000000 ) ) ;
#16622 = DIRECTION ( 'NONE',  ( 0.6724985119639532716, 0.2185080122244073830, -0.7071067811865523467 ) ) ;
#16623 = CARTESIAN_POINT ( 'NONE',  ( -10.44103466624267185, 32.57396620494226624, 7.000000000000000000 ) ) ;
#16624 = CYLINDRICAL_SURFACE ( 'NONE', #16459, 6.000000000000005329 ) ;
#16625 = CARTESIAN_POINT ( 'NONE',  ( 14.29899370898130506, 28.88346223184144890, -7.751924271491758667 ) ) ;
#16626 = DIRECTION ( 'NONE',  ( 0.9781476007338042455, -0.2079116908177656431, 0.000000000000000000 ) ) ;
#16627 = EDGE_LOOP ( 'NONE', ( #3333, #1044, #34409, #21155 ) ) ;
#16629 = CARTESIAN_POINT ( 'NONE',  ( 9.356056665764066693, 26.06569820189703179, 10.49999999999999822 ) ) ;
#16628 = CARTESIAN_POINT ( 'NONE',  ( -19.02631976647747436, 12.44553799571251851, -16.97951980596597821 ) ) ;
#16630 = CARTESIAN_POINT ( 'NONE',  ( 2.166144593658585471, 42.50000000000004974, 11.00000000000000000 ) ) ;
#16631 = CARTESIAN_POINT ( 'NONE',  ( 10.04937125551628618, -18.78011654068590630, -25.00484559559975395 ) ) ;
#16632 = DIRECTION ( 'NONE',  ( 0.5877852522924690293, -0.8090169943749504489, 0.000000000000000000 ) ) ;
#16633 = CARTESIAN_POINT ( 'NONE',  ( 15.21849957777671314, 26.45364063945018174, -7.826203491635935094 ) ) ;
#16634 = CARTESIAN_POINT ( 'NONE',  ( -37.49625565938783467, -14.69322820095472792, -14.45070082761207964 ) ) ;
#16635 = CYLINDRICAL_SURFACE ( 'NONE', #14842, 1.000000000000000000 ) ;
#16636 = EDGE_CURVE ( 'NONE', #12323, #36981, #26405, .T. ) ;
#16637 = CARTESIAN_POINT ( 'NONE',  ( -18.30114940672576296, -16.17431463582818552, -20.81536956475945743 ) ) ;
#16638 = CARTESIAN_POINT ( 'NONE',  ( 5.525540643850987088, -23.27048628860477208, -14.83466894819389559 ) ) ;
#16639 = CARTESIAN_POINT ( 'NONE',  ( 14.36253475959486536, 24.29084598106111059, -12.55734418687435472 ) ) ;
#16640 = EDGE_CURVE ( 'NONE', #25293, #37715, #13985, .T. ) ;
#16641 = CARTESIAN_POINT ( 'NONE',  ( 19.39710119862932558, 14.36785624656014271, -11.87024744276765809 ) ) ;
#16642 = LINE ( 'NONE', #35120, #19917 ) ;
#16643 = DIRECTION ( 'NONE',  ( -1.000000000000000000, 0.000000000000000000, 0.000000000000000000 ) ) ;
#16644 = ORIENTED_EDGE ( 'NONE', *, *, #8926, .F. ) ;
#16645 = CARTESIAN_POINT ( 'NONE',  ( -7.519639825678971157, 28.17713263649764244, -15.83309228201346741 ) ) ;
#16646 = ORIENTED_EDGE ( 'NONE', *, *, #3667, .F. ) ;
#16647 = AXIS2_PLACEMENT_3D ( 'NONE', #28312, #27918, #94 ) ;
#16648 = CARTESIAN_POINT ( 'NONE',  ( 14.97009266215789758, 21.42933399866903699, 10.59344459855564580 ) ) ;
#16649 = ORIENTED_EDGE ( 'NONE', *, *, #12994, .F. ) ;
#16650 = CARTESIAN_POINT ( 'NONE',  ( 30.63487244704973733, -0.03777629022359453581, -7.357755587464951397 ) ) ;
#16651 = DIRECTION ( 'NONE',  ( 0.6691306063588687847, 0.7431448254773848072, 0.000000000000000000 ) ) ;
#16652 = CARTESIAN_POINT ( 'NONE',  ( -30.17922767059062394, -0.7536324250866187624, 17.42190598798393708 ) ) ;
#16653 = ORIENTED_EDGE ( 'NONE', *, *, #38334, .F. ) ;
#16654 = CARTESIAN_POINT ( 'NONE',  ( -25.77377119570790143, 0.4699378652983322580, -16.45710013214238288 ) ) ;
#16655 = EDGE_LOOP ( 'NONE', ( #37048, #38889, #22541, #32741 ) ) ;
#16656 = CARTESIAN_POINT ( 'NONE',  ( 29.08655274285753833, -6.911406729420680684, -14.90707277284040977 ) ) ;
#16657 = ORIENTED_EDGE ( 'NONE', *, *, #38570, .T. ) ;
#16658 = SHAPE_DEFINITION_REPRESENTATION ( #6427, #15382 ) ;
#16659 = CARTESIAN_POINT ( 'NONE',  ( 1.947644445291113025, 40.50000000000006395, 11.00000000000000178 ) ) ;
#16660 = DIRECTION ( 'NONE',  ( -0.4067366430757888840, 0.9135454576426059736, 0.000000000000000000 ) ) ;
#16661 = CARTESIAN_POINT ( 'NONE',  ( -0.4999999999999995559, 37.00000000000000711, 11.00000000000000000 ) ) ;
#16662 = CARTESIAN_POINT ( 'NONE',  ( 9.543723562658483317, 28.97375833662212941, 19.66345542862530138 ) ) ;
#16663 = DIRECTION ( 'NONE',  ( 1.000000000000000000, 0.000000000000000000, 0.000000000000000000 ) ) ;
#16664 = ORIENTED_EDGE ( 'NONE', *, *, #12942, .T. ) ;
#16665 =( NAMED_UNIT ( * ) SI_UNIT ( $, .STERADIAN. ) SOLID_ANGLE_UNIT ( ) );
#16666 = CARTESIAN_POINT ( 'NONE',  ( 3.503793317224327186, 8.420815634768674229, 7.499999999999990230 ) ) ;
#16667 = CARTESIAN_POINT ( 'NONE',  ( 17.34253826607184479, 27.32041144404033162, 23.00000000000000000 ) ) ;
#16668 = ADVANCED_FACE ( 'NONE', ( #38365 ), #6303, .T. ) ;
#16669 = B_SPLINE_CURVE_WITH_KNOTS ( 'NONE', 3,
 ( #1424, #26200, #38595, #32915, #36155, #27403 ),
 .UNSPECIFIED., .F., .F.,
 ( 4, 2, 4 ),
 ( 0.000000000000000000, 0.4999999999999988898, 1.000000000000000000 ),
 .UNSPECIFIED. ) ;
#16670 = CARTESIAN_POINT ( 'NONE',  ( -0.3762682982559537037, 25.43444280220171194, 6.000000000000000000 ) ) ;
#16671 = CARTESIAN_POINT ( 'NONE',  ( 17.61609821162914713, 19.90481306378846682, -7.394926759373131375 ) ) ;
#16672 = VECTOR ( 'NONE', #9248, 999.9999999999998863 ) ;
#16673 = CARTESIAN_POINT ( 'NONE',  ( 6.371632084311922739, 19.71237340112613268, -27.83441168883466688 ) ) ;
#16674 = VECTOR ( 'NONE', #35021, 1000.000000000000000 ) ;
#16675 = ORIENTED_EDGE ( 'NONE', *, *, #683, .T. ) ;
#16676 = DIRECTION ( 'NONE',  ( -0.6459741880212513943, 0.2876062384759537349, -0.7071067811865459074 ) ) ;
#16677 = CARTESIAN_POINT ( 'NONE',  ( -1.000000000000000000, 37.00000000000000711, 10.50000000000000178 ) ) ;
#16678 = CARTESIAN_POINT ( 'NONE',  ( 10.87541234147110636, -18.92597107710026449, -23.77079982040127248 ) ) ;
#16679 = CARTESIAN_POINT ( 'NONE',  ( -2.109373541296176935, 27.06550157850341876, 20.99999999999999289 ) ) ;
#16680 = DIRECTION ( 'NONE',  ( 1.000000000000000000, 0.000000000000000000, 0.000000000000000000 ) ) ;
#16681 = ORIENTED_EDGE ( 'NONE', *, *, #10390, .F. ) ;
#16682 = CARTESIAN_POINT ( 'NONE',  ( -14.29267867992720298, 24.46646551869955388, -12.55102490079049282 ) ) ;
#16683 = CARTESIAN_POINT ( 'NONE',  ( -32.86149060640480712, -21.03113892363543869, 15.72805884748907879 ) ) ;
#16684 = CARTESIAN_POINT ( 'NONE',  ( 14.59266630479183036, -26.14775508231291923, -8.302069403805344194 ) ) ;
#16685 = CARTESIAN_POINT ( 'NONE',  ( 0.5000000000000001110, 33.00000000000000000, 11.00000000000000000 ) ) ;
#16686 = ORIENTED_EDGE ( 'NONE', *, *, #21798, .T. ) ;
#16687 = VERTEX_POINT ( 'NONE', #23532 ) ;
#16688 = CARTESIAN_POINT ( 'NONE',  ( -13.08275260916906113, 30.80677173799382018, -8.144048944713123461 ) ) ;
#16689 = DIRECTION ( 'NONE',  ( 0.000000000000000000, 0.000000000000000000, 1.000000000000000000 ) ) ;
#16690 = FACE_BOUND ( 'NONE', #12948, .T. ) ;
#16691 = CARTESIAN_POINT ( 'NONE',  ( -23.45153049914467047, -5.794994276869281258, -20.93761132930348268 ) ) ;
#16692 = CARTESIAN_POINT ( 'NONE',  ( -13.55123249967971510, 16.06769038696092622, 7.165319362607849740 ) ) ;
#16693 = EDGE_LOOP ( 'NONE', ( #18533, #37783, #3422, #36973 ) ) ;
#16694 = CARTESIAN_POINT ( 'NONE',  ( 20.47484565207173546, 1.015995796922180006, -29.35120656865814937 ) ) ;
#16695 = CARTESIAN_POINT ( 'NONE',  ( -6.935776944912362296, 22.65328985282726393, 12.00000000000000000 ) ) ;
#16696 = DIRECTION ( 'NONE',  ( 1.000000000000000000, 0.000000000000000000, 0.000000000000000000 ) ) ;
#16697 = ADVANCED_FACE ( 'NONE', ( #23337 ), #19267, .T. ) ;
#16698 = EDGE_LOOP ( 'NONE', ( #22109, #34809 ) ) ;
#16699 = CARTESIAN_POINT ( 'NONE',  ( -30.61903234434311827, -0.02130004668534590459, -7.357831981613901284 ) ) ;
#16700 = DIRECTION ( 'NONE',  ( 1.000000000000000000, 0.000000000000000000, 0.000000000000000000 ) ) ;
#16701 = ORIENTED_EDGE ( 'NONE', *, *, #39444, .T. ) ;
#16702 = CARTESIAN_POINT ( 'NONE',  ( 20.61746273054656342, -1.604345479211515491, -27.95458587662992400 ) ) ;
#16703 = CIRCLE ( 'NONE', #39395, 0.9999999999999994449 ) ;
#16704 = AXIS2_PLACEMENT_3D ( 'NONE', #14391, #11548, #5044 ) ;
#16705 = DIRECTION ( 'NONE',  ( 0.000000000000000000, 0.000000000000000000, 1.000000000000000000 ) ) ;
#16706 = CARTESIAN_POINT ( 'NONE',  ( 24.08250333996883441, -26.67951267124112746, 16.30093088680228774 ) ) ;
#16707 = ORIENTED_EDGE ( 'NONE', *, *, #13854, .F. ) ;
#16708 = CARTESIAN_POINT ( 'NONE',  ( 1.782755275185735400, 38.97445513318768207, 15.72805884748939853 ) ) ;
#16709 = VECTOR ( 'NONE', #10251, 1000.000000000000000 ) ;
#16710 = CARTESIAN_POINT ( 'NONE',  ( -16.60464863831923310, -22.41657912772977213, 19.66345542862528717 ) ) ;
#16711 = FACE_OUTER_BOUND ( 'NONE', #21398, .T. ) ;
#16712 = CARTESIAN_POINT ( 'NONE',  ( 4.439345875601470759, 26.26892473594527289, 21.00000000000000355 ) ) ;
#16713 = VECTOR ( 'NONE', #3176, 1000.000000000000114 ) ;
#16714 = FACE_OUTER_BOUND ( 'NONE', #26132, .T. ) ;
#16715 = EDGE_CURVE ( 'NONE', #6329, #4036, #18648, .T. ) ;
#16716 = DIRECTION ( 'NONE',  ( 0.000000000000000000, 0.000000000000000000, 1.000000000000000000 ) ) ;
#16717 = CYLINDRICAL_SURFACE ( 'NONE', #19086, 1.000000000000000000 ) ;
#16718 = ADVANCED_FACE ( 'NONE', ( #4442 ), #19473, .T. ) ;
#16719 = CARTESIAN_POINT ( 'NONE',  ( 29.73172958077877581, -1.192874570370699328, 17.92354375535250810 ) ) ;
#16720 = CARTESIAN_POINT ( 'NONE',  ( -19.17173663826903862, 7.846818401146893329, -26.59525583229557810 ) ) ;
#16721 = EDGE_CURVE ( 'NONE', #39914, #28188, #8259, .T. ) ;
#16722 = CARTESIAN_POINT ( 'NONE',  ( 20.67276675977905498, -26.96143717380833849, -7.241510599420801775 ) ) ;
#16723 = CARTESIAN_POINT ( 'NONE',  ( -13.13294332834922251, 16.07239217250488750, 10.49999999999999822 ) ) ;
#16724 = VERTEX_POINT ( 'NONE', #33296 ) ;
#16725 = CARTESIAN_POINT ( 'NONE',  ( 15.28171370150459829, 26.81318960135283902, -6.883740541788177403 ) ) ;
#16726 = AXIS2_PLACEMENT_3D ( 'NONE', #15845, #9352, #5695 ) ;
#16727 = ORIENTED_EDGE ( 'NONE', *, *, #10369, .T. ) ;
#16729 = AXIS2_PLACEMENT_3D ( 'NONE', #9052, #40116, #12293 ) ;
#16728 = CARTESIAN_POINT ( 'NONE',  ( -11.84261757144468596, 17.09703652377666927, -26.89487436953058008 ) ) ;
#16730 = CARTESIAN_POINT ( 'NONE',  ( -21.56514238326832000, -22.66165022683772889, 19.66345542862498519 ) ) ;
#16731 = CARTESIAN_POINT ( 'NONE',  ( -1.590043107810761525, 12.61456814725308817, 10.50000000000001066 ) ) ;
#16732 = CARTESIAN_POINT ( 'NONE',  ( 11.23528749269386395, 17.71942187280074421, -26.23031324771008244 ) ) ;
#16733 = ORIENTED_EDGE ( 'NONE', *, *, #12085, .T. ) ;
#16734 = CARTESIAN_POINT ( 'NONE',  ( 27.44116408010769703, -15.12913582886689134, -14.73136720375602415 ) ) ;
#16735 = DIRECTION ( 'NONE',  ( 0.000000000000000000, 0.000000000000000000, 1.000000000000000000 ) ) ;
#16736 = VERTEX_POINT ( 'NONE', #30640 ) ;
#16737 = AXIS2_PLACEMENT_3D ( 'NONE', #36347, #8511, #27198 ) ;
#16739 = CARTESIAN_POINT ( 'NONE',  ( 6.572794801194151049, 16.58182897866491956, 7.000000000000000000 ) ) ;
#16738 = CARTESIAN_POINT ( 'NONE',  ( -15.23746052738172096, 27.38211562678985445, -5.000000000000001776 ) ) ;
#16740 = CARTESIAN_POINT ( 'NONE',  ( -16.15831973348936401, -26.82997807573334725, -6.405446087739315786 ) ) ;
#16741 = DIRECTION ( 'NONE',  ( 0.3090169943749573878, 0.9510565162951503115, 0.000000000000000000 ) ) ;
#16742 = AXIS2_PLACEMENT_3D ( 'NONE', #6387, #11901, #107 ) ;
#16743 = ORIENTED_EDGE ( 'NONE', *, *, #7884, .T. ) ;
#16744 = CARTESIAN_POINT ( 'NONE',  ( -18.70070976566389831, -8.421454915599365876, -30.00000000000000711 ) ) ;
#16745 = CARTESIAN_POINT ( 'NONE',  ( -12.96835034737378045, -23.58818813561633831, -14.49844098154287053 ) ) ;
#16746 = CARTESIAN_POINT ( 'NONE',  ( 0.5000000000000001110, 37.00000000000000711, 7.000000000000000000 ) ) ;
#16747 = CARTESIAN_POINT ( 'NONE',  ( 17.09040934979314841, 20.79557903151203746, -8.349269920398814548 ) ) ;
#16748 = ORIENTED_EDGE ( 'NONE', *, *, #38451, .T. ) ;
#16749 = CARTESIAN_POINT ( 'NONE',  ( 20.78981288118261261, 4.511901260326916407, -24.21075109639451384 ) ) ;
#16750 = DIRECTION ( 'NONE',  ( -1.000000000000000000, 0.000000000000000000, 0.000000000000000000 ) ) ;
#16751 = EDGE_CURVE ( 'NONE', #11294, #33679, #37457, .T. ) ;
#16752 = CARTESIAN_POINT ( 'NONE',  ( -18.76090689389218014, -16.22676322417297001, 23.00000000000000000 ) ) ;
#16753 = ADVANCED_FACE ( 'NONE', ( #17455 ), #25131, .T. ) ;
#16754 = VERTEX_POINT ( 'NONE', #33093 ) ;
#16755 = CARTESIAN_POINT ( 'NONE',  ( -24.04802182397615340, 0.2326015010894557367, -19.46165338998660133 ) ) ;
#16756 = CARTESIAN_POINT ( 'NONE',  ( 20.49706908807578287, 0.3883427504116042650, -30.00000000000000355 ) ) ;
#16757 = CARTESIAN_POINT ( 'NONE',  ( 18.04765032505117972, -21.12132759291071693, 20.25080042701545580 ) ) ;
#16758 = VERTEX_POINT ( 'NONE', #30236 ) ;
#16759 = CARTESIAN_POINT ( 'NONE',  ( 6.155076441694338207, 21.71698211341367113, -30.00000000000000000 ) ) ;
#16760 = CARTESIAN_POINT ( 'NONE',  ( -6.762317648414995830, 29.93445088906605989, 10.49999999999999822 ) ) ;
#16761 = AXIS2_PLACEMENT_3D ( 'NONE', #39178, #26589, #17056 ) ;
#16762 = VECTOR ( 'NONE', #23031, 1000.000000000000000 ) ;
#16763 = DIRECTION ( 'NONE',  ( 0.000000000000000000, 0.000000000000000000, 1.000000000000000000 ) ) ;
#16764 = CARTESIAN_POINT ( 'NONE',  ( -30.90412082983252873, -0.04211290444285954726, 0.000000000000000000 ) ) ;
#16765 = AXIS2_PLACEMENT_3D ( 'NONE', #15605, #37140, #18853 ) ;
#16766 = ADVANCED_FACE ( 'NONE', ( #8897 ), #8902, .T. ) ;
#16767 = FACE_OUTER_BOUND ( 'NONE', #17800, .T. ) ;
#16768 = CARTESIAN_POINT ( 'NONE',  ( -1.229437847141422901, 24.50739181907689712, 12.00000000000000000 ) ) ;
#16769 = LINE ( 'NONE', #1320, #8783 ) ;
#16770 = ORIENTED_EDGE ( 'NONE', *, *, #34881, .F. ) ;
#16771 = CARTESIAN_POINT ( 'NONE',  ( 10.10646936306337729, 32.94553861768082470, 10.49999999999999645 ) ) ;
#16772 = CARTESIAN_POINT ( 'NONE',  ( -8.118377661053489902, 10.47536095541709322, 7.000000000000000000 ) ) ;
#16773 = CARTESIAN_POINT ( 'NONE',  ( 24.52772961496341608, -22.70861085562849624, -12.04500047335969271 ) ) ;
#16774 = LINE ( 'NONE', #25492, #3074 ) ;
#16775 = DIRECTION ( 'NONE',  ( -0.6691306063588670083, -0.7431448254773863615, 0.000000000000000000 ) ) ;
#16776 = CARTESIAN_POINT ( 'NONE',  ( 13.48825381686340741, 24.00059731804531538, -14.41398086289930269 ) ) ;
#16777 = DIRECTION ( 'NONE',  ( 0.6691306063588678965, 0.7431448254773855844, 0.000000000000000000 ) ) ;
#16778 = ORIENTED_EDGE ( 'NONE', *, *, #1565, .T. ) ;
#16779 = CARTESIAN_POINT ( 'NONE',  ( -16.15633541497567194, 17.24146705615139652, -16.81735594647537013 ) ) ;
#16780 = DIRECTION ( 'NONE',  ( 0.000000000000000000, 0.000000000000000000, 1.000000000000000000 ) ) ;
#16781 = CARTESIAN_POINT ( 'NONE',  ( 14.25957742305259046, -25.05340746124562301, -11.60179240159362912 ) ) ;
#16782 = DIRECTION ( 'NONE',  ( 0.000000000000000000, 0.000000000000000000, 1.000000000000000000 ) ) ;
#16783 = CARTESIAN_POINT ( 'NONE',  ( 11.01382701200410352, 17.34314758767475695, -28.70727912091412293 ) ) ;
#16784 = ORIENTED_EDGE ( 'NONE', *, *, #10143, .F. ) ;
#16785 = CARTESIAN_POINT ( 'NONE',  ( 12.92727378465670895, 21.65459399332963386, -17.43760083564437124 ) ) ;
#16786 = ORIENTED_EDGE ( 'NONE', *, *, #3444, .F. ) ;
#16788 = CARTESIAN_POINT ( 'NONE',  ( 14.39395135575595042, 26.65114718998425047, 10.68306085400107719 ) ) ;
#16787 = CARTESIAN_POINT ( 'NONE',  ( -14.90130370912292967, 25.90675389883749347, -9.703026954905764612 ) ) ;
#16789 = CARTESIAN_POINT ( 'NONE',  ( -14.00737455831331069, -24.60610348959216864, -12.55177947858446785 ) ) ;
#16790 = CARTESIAN_POINT ( 'NONE',  ( -18.84783625459284906, -29.28148485008969715, 12.14047268033134763 ) ) ;
#16791 = VECTOR ( 'NONE', #34120, 999.9999999999998863 ) ;
#16792 = CIRCLE ( 'NONE', #39491, 1.000000000000000000 ) ;
#16793 = CARTESIAN_POINT ( 'NONE',  ( -17.22654052972206173, -11.11309616262812838, -30.00000000000001421 ) ) ;
#16794 = CARTESIAN_POINT ( 'NONE',  ( -1.866162468650815365, -20.97895390888915301, -24.40979417473883473 ) ) ;
#16795 = CARTESIAN_POINT ( 'NONE',  ( 15.30672036741259490, 24.25326656399939296, -10.20631967863550749 ) ) ;
#16796 = VERTEX_POINT ( 'NONE', #21287 ) ;
#16797 = CARTESIAN_POINT ( 'NONE',  ( 23.15824302559796521, 9.164155139735443711, -8.398248912862177562 ) ) ;
#16798 = CARTESIAN_POINT ( 'NONE',  ( 28.32385402320780798, -24.64261966148930583, -4.999999999999998224 ) ) ;
#16799 = CARTESIAN_POINT ( 'NONE',  ( 2.510240364580639039, -24.77672057670806183, -5.000000000000004441 ) ) ;
#16800 = EDGE_CURVE ( 'NONE', #37976, #37515, #29826, .T. ) ;
#16801 = CARTESIAN_POINT ( 'NONE',  ( 14.97058623676931077, 26.66112013780997003, 16.87380292611441135 ) ) ;
#16802 = CIRCLE ( 'NONE', #27836, 1.000000000000000888 ) ;
#16803 = ORIENTED_EDGE ( 'NONE', *, *, #23455, .F. ) ;
#16804 = CARTESIAN_POINT ( 'NONE',  ( -31.17348492595634113, -2.327576281512217626, -10.48814752622052104 ) ) ;
#16805 = CARTESIAN_POINT ( 'NONE',  ( -14.06669941890059761, 14.65883224165446208, 19.99202127657103389 ) ) ;
#16806 = ORIENTED_EDGE ( 'NONE', *, *, #6027, .T. ) ;
#16807 = DIRECTION ( 'NONE',  ( 1.000000000000000000, 0.000000000000000000, 0.000000000000000000 ) ) ;
#16808 = DIRECTION ( 'NONE',  ( -0.000000000000000000, -0.000000000000000000, -1.000000000000000000 ) ) ;
#16809 = CARTESIAN_POINT ( 'NONE',  ( 11.41267482483262619, 26.20820393249957192, 6.000000000000000000 ) ) ;
#16810 = CARTESIAN_POINT ( 'NONE',  ( 34.95664498758854677, -15.33017443246186495, -4.999999999999996447 ) ) ;
#16811 = CARTESIAN_POINT ( 'NONE',  ( 36.93643098903794453, -14.76343610888346092, 12.73282698324853257 ) ) ;
#16812 = ORIENTED_EDGE ( 'NONE', *, *, #2222, .T. ) ;
#16813 = DIRECTION ( 'NONE',  ( -0.000000000000000000, -0.000000000000000000, 1.000000000000000000 ) ) ;
#16814 = CARTESIAN_POINT ( 'NONE',  ( -15.43632923247374755, 26.71034459555102103, -5.000000000000004441 ) ) ;
#16815 = EDGE_CURVE ( 'NONE', #11229, #26705, #23732, .T. ) ;
#16816 = VECTOR ( 'NONE', #14581, 1000.000000000000000 ) ;
#16817 = LINE ( 'NONE', #5017, #11690 ) ;
#16818 = ORIENTED_EDGE ( 'NONE', *, *, #12792, .F. ) ;
#16819 = EDGE_CURVE ( 'NONE', #36134, #36348, #31585, .T. ) ;
#16820 = CARTESIAN_POINT ( 'NONE',  ( -1.871070526050384597, 37.10316175800964800, -8.844908016778285642 ) ) ;
#16821 = CYLINDRICAL_SURFACE ( 'NONE', #17874, 0.4999999999999997780 ) ;
#16822 = CARTESIAN_POINT ( 'NONE',  ( 17.34253826607184479, 27.32041144404033162, 11.00000000000000000 ) ) ;
#16823 = ADVANCED_FACE ( 'NONE', ( #36331 ), #11350, .T. ) ;
#16824 = VECTOR ( 'NONE', #38795, 1000.000000000000114 ) ;
#16825 = CARTESIAN_POINT ( 'NONE',  ( 12.83926296998458128, 26.67172942406175906, 7.000000000000000000 ) ) ;
#16826 = LINE ( 'NONE', #19869, #30783 ) ;
#16827 = CARTESIAN_POINT ( 'NONE',  ( -14.91782843052412488, 20.93207305098534832, 7.000000000000000000 ) ) ;
#16828 = CARTESIAN_POINT ( 'NONE',  ( 14.18620732935935003, 29.69268515973297440, -6.373436630974609329 ) ) ;
#16829 = FACE_OUTER_BOUND ( 'NONE', #852, .T. ) ;
#16830 = ORIENTED_EDGE ( 'NONE', *, *, #14892, .T. ) ;
#16831 = ADVANCED_FACE ( 'NONE', ( #39570 ), #24336, .F. ) ;
#16833 = FACE_OUTER_BOUND ( 'NONE', #366, .T. ) ;
#16832 = CARTESIAN_POINT ( 'NONE',  ( -20.14604714284210729, 14.61654826405655072, -6.936879617510046891 ) ) ;
#16834 = CARTESIAN_POINT ( 'NONE',  ( -14.11133924723972655, 27.61078317377209501, 10.59344459855564757 ) ) ;
#16835 = CARTESIAN_POINT ( 'NONE',  ( 15.53709981414127483, -26.75515487142352100, -5.473964991478021069 ) ) ;
#16836 = CARTESIAN_POINT ( 'NONE',  ( 12.80736835487433289, 15.68301270189216545, 7.499999999999997335 ) ) ;
#16837 = CARTESIAN_POINT ( 'NONE',  ( 11.27293877700655678, 18.06695805791709830, -25.00947300646876670 ) ) ;
#16838 = CARTESIAN_POINT ( 'NONE',  ( -20.90924525106831666, -8.502318254486386451, -30.00000000000000711 ) ) ;
#16839 = CARTESIAN_POINT ( 'NONE',  ( 0.000000000000000000, 22.50000000000000355, 7.000000000000000000 ) ) ;
#16840 = CARTESIAN_POINT ( 'NONE',  ( -25.39332128722019988, -23.88597321859529288, -10.24008034875545370 ) ) ;
#16841 = CARTESIAN_POINT ( 'NONE',  ( 6.121139850082340850, -20.67279834681676576, -23.15975327329053002 ) ) ;
#16842 = CARTESIAN_POINT ( 'NONE',  ( 15.45245795801566935, 26.38988594971563728, -6.417325671787477148 ) ) ;
#16843 = CARTESIAN_POINT ( 'NONE',  ( 17.10314071577965933, 11.30215440122589499, -29.42840768176305133 ) ) ;
#16844 = CARTESIAN_POINT ( 'NONE',  ( 10.16520467992603294, 20.33931832809677331, 6.000000000000000000 ) ) ;
#16845 = CARTESIAN_POINT ( 'NONE',  ( -20.38753357181593628, -16.19769905861789994, 21.00000000000001421 ) ) ;
#16847 = VERTEX_POINT ( 'NONE', #8699 ) ;
#16846 = EDGE_CURVE ( 'NONE', #22802, #23608, #24131, .T. ) ;
#16848 = CARTESIAN_POINT ( 'NONE',  ( -5.336011467082187210, 20.01953256073105081, -27.79733467733078456 ) ) ;
#16849 = EDGE_CURVE ( 'NONE', #16537, #19499, #26777, .T. ) ;
#16850 = ORIENTED_EDGE ( 'NONE', *, *, #19505, .T. ) ;
#16851 = CARTESIAN_POINT ( 'NONE',  ( -11.78982961964231535, -21.49398613183140228, -18.46362487464430302 ) ) ;
#16852 = EDGE_CURVE ( 'NONE', #35202, #13016, #34213, .T. ) ;
#16853 = VECTOR ( 'NONE', #37104, 1000.000000000000114 ) ;
#16854 = DIRECTION ( 'NONE',  ( -1.000000000000000000, 0.000000000000000000, 0.000000000000000000 ) ) ;
#16855 = ORIENTED_EDGE ( 'NONE', *, *, #19639, .F. ) ;
#16856 = CARTESIAN_POINT ( 'NONE',  ( 26.53299061067440334, 0.2339631145021888736, -15.44550104827009740 ) ) ;
#16857 = CARTESIAN_POINT ( 'NONE',  ( -7.929471891321299815, 25.60217271033470965, 7.000000000000000000 ) ) ;
#16858 = CARTESIAN_POINT ( 'NONE',  ( -8.411683849014160330, 19.76687823897114882, 9.000000000000001776 ) ) ;
#16859 = AXIS2_PLACEMENT_3D ( 'NONE', #14814, #32912, #32712 ) ;
#16860 = VERTEX_POINT ( 'NONE', #33499 ) ;
#16861 = CARTESIAN_POINT ( 'NONE',  ( -30.08539553338631123, 0.1183567654270563652, -8.769032276601203435 ) ) ;
#16862 = ORIENTED_EDGE ( 'NONE', *, *, #22710, .T. ) ;
#16863 = CARTESIAN_POINT ( 'NONE',  ( 20.28784519644407425, -4.806164102564737028, -27.11309778525960468 ) ) ;
#16864 = VERTEX_POINT ( 'NONE', #20894 ) ;
#16865 = CARTESIAN_POINT ( 'NONE',  ( 3.900486991066165476, 40.17991855518013011, 11.55979286843954412 ) ) ;
#16866 = CARTESIAN_POINT ( 'NONE',  ( -8.412270287199726582, 10.07085245822961994, 7.000000000000000000 ) ) ;
#16867 = DIRECTION ( 'NONE',  ( 1.000000000000000000, 0.000000000000000000, 0.000000000000000000 ) ) ;
#16868 = EDGE_CURVE ( 'NONE', #29585, #17337, #17857, .T. ) ;
#16869 = CARTESIAN_POINT ( 'NONE',  ( -7.884092257453602315, 32.87438847863548119, 18.87996532025784546 ) ) ;
#16870 = CARTESIAN_POINT ( 'NONE',  ( -1.642021030515208979, 12.37003124706962787, 10.75000000000001421 ) ) ;
#16871 = ORIENTED_EDGE ( 'NONE', *, *, #33612, .T. ) ;
#16872 = ADVANCED_FACE ( 'NONE', ( #17658 ), #18247, .F. ) ;
#16873 =( NAMED_UNIT ( * ) PLANE_ANGLE_UNIT ( ) SI_UNIT ( $, .RADIAN. ) );
#16874 = CARTESIAN_POINT ( 'NONE',  ( -17.09830543661136559, -11.32827756084940951, -30.00000000000001776 ) ) ;
#16875 = CARTESIAN_POINT ( 'NONE',  ( 8.917734535019441466, 14.47043272369397116, 6.000000000000000000 ) ) ;
#16876 = CYLINDRICAL_SURFACE ( 'NONE', #28584, 6.000000000000014211 ) ;
#16877 = CARTESIAN_POINT ( 'NONE',  ( 18.89396845472720088, 16.74745873269439400, -8.388403218796401717 ) ) ;
#16879 = VECTOR ( 'NONE', #23969, 1000.000000000000227 ) ;
#16878 = CARTESIAN_POINT ( 'NONE',  ( 9.653912746977081127, 30.01279398118651542, -13.05665368966775475 ) ) ;
#16880 = ORIENTED_EDGE ( 'NONE', *, *, #11766, .T. ) ;
#16881 = DIRECTION ( 'NONE',  ( 1.000000000000000000, 0.000000000000000000, 0.000000000000000000 ) ) ;
#16882 = CARTESIAN_POINT ( 'NONE',  ( 7.929471891321336230, 25.60217271033461373, 7.000000000000000000 ) ) ;
#16883 = CARTESIAN_POINT ( 'NONE',  ( 10.59539299448435479, -18.54736905940730551, -24.94025571391961194 ) ) ;
#16884 = CARTESIAN_POINT ( 'NONE',  ( 18.23649648353767461, -16.09146789626181118, 20.99999999999999645 ) ) ;
#16885 = VECTOR ( 'NONE', #26351, 1000.000000000000000 ) ;
#16886 = CARTESIAN_POINT ( 'NONE',  ( 1.000000000000000222, 36.50000000000000711, 10.50000000000000000 ) ) ;
#16887 = VERTEX_POINT ( 'NONE', #39966 ) ;
#16888 = CARTESIAN_POINT ( 'NONE',  ( -11.04584868602368353, 17.42116418599707117, -28.07775973395273539 ) ) ;
#16889 = CARTESIAN_POINT ( 'NONE',  ( -31.71434132860544963, -22.43226626709165572, 15.72805884748934524 ) ) ;
#16890 = CARTESIAN_POINT ( 'NONE',  ( 9.384463268206888031, -18.58243950274592393, -26.85571026258529059 ) ) ;
#16891 = CARTESIAN_POINT ( 'NONE',  ( -3.100643064501314328, 15.70406341247269211, 6.000000000000000000 ) ) ;
#16892 = ORIENTED_EDGE ( 'NONE', *, *, #3040, .T. ) ;
#16893 = ORIENTED_EDGE ( 'NONE', *, *, #11180, .T. ) ;
#16894 = CARTESIAN_POINT ( 'NONE',  ( -11.17084153242268485, 24.05774765238854940, -17.12906072756529596 ) ) ;
#16895 = CARTESIAN_POINT ( 'NONE',  ( -17.08966009880722936, -22.85233454443725165, -15.10154554499656854 ) ) ;
#16896 = CARTESIAN_POINT ( 'NONE',  ( -12.51373512357471363, 14.69784138864699230, 10.94387467463490893 ) ) ;
#16897 = VECTOR ( 'NONE', #25989, 1000.000000000000000 ) ;
#16898 = CARTESIAN_POINT ( 'NONE',  ( -21.87366440923314315, -5.401708001756898803, -23.22369624925320508 ) ) ;
#16899 = CYLINDRICAL_SURFACE ( 'NONE', #19555, 1.000000000000000000 ) ;
#16900 = EDGE_LOOP ( 'NONE', ( #30681, #39483, #16418, #38369 ) ) ;
#16901 = CARTESIAN_POINT ( 'NONE',  ( 28.72940827134124575, 0.2944283357868948681, -11.60603752271954292 ) ) ;
#16902 = CARTESIAN_POINT ( 'NONE',  ( -11.16521142134453726, 24.66068167190384841, 12.00000000000000000 ) ) ;
#16903 = CARTESIAN_POINT ( 'NONE',  ( -9.892954722048921568, 20.95745441963943634, 10.00000000000000000 ) ) ;
#16904 = UNCERTAINTY_MEASURE_WITH_UNIT (LENGTH_MEASURE( 1.000000000000000082E-05 ), #13606, 'distance_accuracy_value', 'NONE');
#16905 = ORIENTED_EDGE ( 'NONE', *, *, #22636, .F. ) ;
#16906 = CARTESIAN_POINT ( 'NONE',  ( -23.32189782144615009, 0.5388808099659079254, -20.54027897587359064 ) ) ;
#16907 = CARTESIAN_POINT ( 'NONE',  ( 0.000000000000000000, 22.50000000000000355, 7.000000000000000000 ) ) ;
#16908 = ORIENTED_EDGE ( 'NONE', *, *, #34833, .F. ) ;
#16909 = CARTESIAN_POINT ( 'NONE',  ( 22.68321730624148813, -1.879180904300666199, -22.42295850830599235 ) ) ;
#16910 = CARTESIAN_POINT ( 'NONE',  ( -3.494943660522439099, 10.76222879119470832, 13.00000000000000178 ) ) ;
#16911 = CARTESIAN_POINT ( 'NONE',  ( 29.03912765165501142, -24.78940378269167866, 15.72805884748905747 ) ) ;
#16912 = EDGE_LOOP ( 'NONE', ( #17812, #24668 ) ) ;
#16913 = CARTESIAN_POINT ( 'NONE',  ( 9.968062119477529848, 35.61660815598495589, 15.72805884748939498 ) ) ;
#16914 = CIRCLE ( 'NONE', #1983, 1.000000000000000888 ) ;
#16915 = CARTESIAN_POINT ( 'NONE',  ( 11.32166530370859547, -20.22988973179433003, 19.99202127657019901 ) ) ;
#16916 = DIRECTION ( 'NONE',  ( -0.6916548014802318400, -0.1470157664651949581, -0.7071067811865421326 ) ) ;
#16917 = CARTESIAN_POINT ( 'NONE',  ( -5.000428297553742851, 29.07988060316462864, 20.69868183039781329 ) ) ;
#16918 = DIRECTION ( 'NONE',  ( 1.000000000000000000, 0.000000000000000000, 0.000000000000000000 ) ) ;
#16919 = DIRECTION ( 'NONE',  ( 0.8090169943749504489, 0.5877852522924690293, -0.000000000000000000 ) ) ;
#16920 = CARTESIAN_POINT ( 'NONE',  ( 5.831757820639368539, 35.44601310684239337, -9.755031229041589924 ) ) ;
#16921 = LINE ( 'NONE', #10617, #13246 ) ;
#16922 = CARTESIAN_POINT ( 'NONE',  ( 27.61482536617424444, 3.986323854220331420, 15.72805884749758931 ) ) ;
#16923 = VECTOR ( 'NONE', #40140, 1000.000000000000000 ) ;
#16924 = CARTESIAN_POINT ( 'NONE',  ( -18.40039352423243457, 9.187127761490295086, -28.29769893192780827 ) ) ;
#16925 = CARTESIAN_POINT ( 'NONE',  ( 20.17145048931689644, -26.36706761496765949, -9.037115501373188309 ) ) ;
#16926 = CYLINDRICAL_SURFACE ( 'NONE', #26841, 1.000000000000000000 ) ;
#16927 = DIRECTION ( 'NONE',  ( -0.8660254037844432595, -0.4999999999999921729, 0.000000000000000000 ) ) ;
#16928 = EDGE_LOOP ( 'NONE', ( #38571, #6585, #15296, #38105 ) ) ;
#16929 = CARTESIAN_POINT ( 'NONE',  ( 11.03496570447431147, 17.67526184817850066, -26.82193291291117276 ) ) ;
#16930 = EDGE_LOOP ( 'NONE', ( #17456, #40060, #35558 ) ) ;
#16931 = CARTESIAN_POINT ( 'NONE',  ( -13.28422579199402520, 19.31593456181959212, -19.64488464522398203 ) ) ;
#16932 = CARTESIAN_POINT ( 'NONE',  ( -28.78203904708374949, -16.61731799165967871, 19.99202127657103034 ) ) ;
#16933 = FACE_OUTER_BOUND ( 'NONE', #20570, .T. ) ;
#16934 = CARTESIAN_POINT ( 'NONE',  ( 11.09155550310888394, 17.39098317871841459, -28.08047184062978374 ) ) ;
#16935 = ORIENTED_EDGE ( 'NONE', *, *, #3867, .F. ) ;
#16936 = CARTESIAN_POINT ( 'NONE',  ( 18.32281867441876599, -9.405883636210713661, -28.44593439518221345 ) ) ;
#16937 = AXIS2_PLACEMENT_3D ( 'NONE', #36053, #32813, #30709 ) ;
#16938 = EDGE_LOOP ( 'NONE', ( #3042, #28835 ) ) ;
#16940 = CARTESIAN_POINT ( 'NONE',  ( -14.97009266215794199, 21.42933399866948463, 10.63089969389957545 ) ) ;
#16939 = CARTESIAN_POINT ( 'NONE',  ( -14.38234336660450019, 25.38722357239544891, -11.56793431969083130 ) ) ;
#16941 = CARTESIAN_POINT ( 'NONE',  ( -10.22076385035975932, -18.36610753837789289, -26.18274680826524303 ) ) ;
#16942 = DIRECTION ( 'NONE',  ( 1.000000000000000000, 0.000000000000000000, 0.000000000000000000 ) ) ;
#16943 = VERTEX_POINT ( 'NONE', #11945 ) ;
#16944 = CARTESIAN_POINT ( 'NONE',  ( -23.64546601257486103, -9.782033131034459927, -19.68101090808202613 ) ) ;
#16945 = CARTESIAN_POINT ( 'NONE',  ( -13.77000343459438803, -24.97058995738720455, -11.61570562419389141 ) ) ;
#16946 = CARTESIAN_POINT ( 'NONE',  ( -10.78894649379783388, 21.72623886970244911, 13.00000000000000178 ) ) ;
#16947 = CARTESIAN_POINT ( 'NONE',  ( 16.72342278700635987, 21.93126413797296692, -7.859335597179046395 ) ) ;
#16948 = VERTEX_POINT ( 'NONE', #12144 ) ;
#16949 = CARTESIAN_POINT ( 'NONE',  ( 24.35141779062506018, 2.949667068470618325, -16.65809308903522634 ) ) ;
#16950 = ADVANCED_FACE ( 'NONE', ( #36734 ), #24533, .F. ) ;
#16951 = LINE ( 'NONE', #10240, #16762 ) ;
#16952 = CARTESIAN_POINT ( 'NONE',  ( -39.59914439355408433, -10.88071517532302757, 23.00000000000187583 ) ) ;
#16953 = EDGE_LOOP ( 'NONE', ( #21391, #22305, #20717, #33011 ) ) ;
#16954 = CARTESIAN_POINT ( 'NONE',  ( -20.53768214670897407, 0.6048634969346144974, -28.69806880511274016 ) ) ;
#16955 = CARTESIAN_POINT ( 'NONE',  ( 31.60127994866165224, -0.7964638025070724936, -5.469550557027236692 ) ) ;
#16956 = CIRCLE ( 'NONE', #18259, 1.000000000000000888 ) ;
#16957 = EDGE_CURVE ( 'NONE', #25929, #21181, #9656, .T. ) ;
#16958 = CARTESIAN_POINT ( 'NONE',  ( 25.82842257350687021, -22.71926374633472534, 18.87996532025747953 ) ) ;
#16959 = CIRCLE ( 'NONE', #26693, 6.000000000000003553 ) ;
#16960 = ORIENTED_EDGE ( 'NONE', *, *, #31843, .T. ) ;
#16961 = CARTESIAN_POINT ( 'NONE',  ( -20.56897251348186728, 2.201150519725052046, -27.52994173289911473 ) ) ;
#16962 = EDGE_CURVE ( 'NONE', #14392, #18018, #29018, .T. ) ;
#16963 = CARTESIAN_POINT ( 'NONE',  ( -30.41237130417910706, 3.314011747244090422, -13.58461195433496371 ) ) ;
#16964 = LINE ( 'NONE', #913, #23842 ) ;
#16965 = CARTESIAN_POINT ( 'NONE',  ( 9.541469607472739867, 17.40487552589537401, 12.00000000000000000 ) ) ;
#16966 = CARTESIAN_POINT ( 'NONE',  ( -8.917741276437942233, 30.52956727630665057, 12.00000000000000000 ) ) ;
#16967 = DIRECTION ( 'NONE',  ( 0.5000000000000043299, 0.8660254037844361541, 0.000000000000000000 ) ) ;
#16968 = CARTESIAN_POINT ( 'NONE',  ( 13.94482798346721175, 26.50521816028912525, 11.00000000000000000 ) ) ;
#16969 = ORIENTED_EDGE ( 'NONE', *, *, #9017, .F. ) ;
#16970 = EDGE_CURVE ( 'NONE', #12750, #26235, #9297, .T. ) ;
#16971 = CARTESIAN_POINT ( 'NONE',  ( 8.910254037844364206, 17.93301270189218855, 10.50000000000000000 ) ) ;
#16972 = EDGE_CURVE ( 'NONE', #29281, #18489, #28370, .T. ) ;
#16973 = CARTESIAN_POINT ( 'NONE',  ( 3.829842517468933671, 8.490119531707911449, 10.66666666666666075 ) ) ;
#16974 = CARTESIAN_POINT ( 'NONE',  ( 27.36121244743086578, -25.22392150776288133, -4.999999999999999112 ) ) ;
#16975 = DIRECTION ( 'NONE',  ( 0.000000000000000000, 0.000000000000000000, -1.000000000000000000 ) ) ;
#16976 = DIRECTION ( 'NONE',  ( 0.000000000000000000, 0.000000000000000000, 1.000000000000000000 ) ) ;
#16977 = CARTESIAN_POINT ( 'NONE',  ( 10.65171411591334127, 17.77866102667491788, -27.41507814813356347 ) ) ;
#16978 = CARTESIAN_POINT ( 'NONE',  ( 12.77090408390491305, 15.39748370681878775, 6.000000000000000000 ) ) ;
#16979 = ORIENTED_EDGE ( 'NONE', *, *, #20086, .T. ) ;
#16980 = AXIS2_PLACEMENT_3D ( 'NONE', #4265, #7715, #14213 ) ;
#16981 = CARTESIAN_POINT ( 'NONE',  ( -17.26788437172030299, 20.57138498279865857, -7.871131841751277669 ) ) ;
#16982 = CARTESIAN_POINT ( 'NONE',  ( -24.28032989564857047, -12.76774640304084052, 20.99999999999999645 ) ) ;
#16983 = CIRCLE ( 'NONE', #15030, 15.00000000000000000 ) ;
#16984 = CARTESIAN_POINT ( 'NONE',  ( 14.87191199626541582, -25.96639945386176151, -9.239640580059129249 ) ) ;
#16985 = CARTESIAN_POINT ( 'NONE',  ( -4.118678732975735279, 7.827785988993307242, 13.00000000000000178 ) ) ;
#16986 = CARTESIAN_POINT ( 'NONE',  ( 15.34748833658096956, 26.58512746428727525, -6.887971585101123395 ) ) ;
#16987 = EDGE_LOOP ( 'NONE', ( #22342, #5624, #2320, #11367, #8350, #23792, #16440 ) ) ;
#16988 = CARTESIAN_POINT ( 'NONE',  ( 11.17889170011724254, 17.76029153187228005, -26.22429826898334326 ) ) ;
#16989 = EDGE_LOOP ( 'NONE', ( #17339, #32315, #22977, #38982 ) ) ;
#16991 = CARTESIAN_POINT ( 'NONE',  ( 36.48557158514975640, -11.24999999999995559, 10.00000000000000000 ) ) ;
#16990 = CARTESIAN_POINT ( 'NONE',  ( -15.37572116813434775, 26.83420713582532002, -5.945198187637174669 ) ) ;
#16992 = CARTESIAN_POINT ( 'NONE',  ( -9.564252382813446474, -18.27657358539217825, -28.07775981309165658 ) ) ;
#16993 = CARTESIAN_POINT ( 'NONE',  ( -32.84658669524019103, -23.46788009898594041, 11.55979286843917819 ) ) ;
#16994 = CARTESIAN_POINT ( 'NONE',  ( -16.89362134160771944, -11.62925611732713804, -29.21493252340928848 ) ) ;
#16995 = CARTESIAN_POINT ( 'NONE',  ( -6.662515794070015041, -20.56860814960122852, -23.12314935263888316 ) ) ;
#16996 = CARTESIAN_POINT ( 'NONE',  ( 15.47267297930532592, 24.57749586628517235, -9.256576209186675896 ) ) ;
#16997 = ORIENTED_EDGE ( 'NONE', *, *, #969, .T. ) ;
#16998 = CARTESIAN_POINT ( 'NONE',  ( 21.96684812253698738, 7.874168224664914284, -15.89034991468182412 ) ) ;
#16999 = CARTESIAN_POINT ( 'NONE',  ( 1.871201846650637046, 31.30332840660451765, 12.00000000000000000 ) ) ;
#17000 = VECTOR ( 'NONE', #27628, 1000.000000000000000 ) ;
#17001 = FACE_OUTER_BOUND ( 'NONE', #33210, .T. ) ;
#17002 = CARTESIAN_POINT ( 'NONE',  ( 1.000000000000000000, 37.00000000000000711, 10.50000000000000178 ) ) ;
#17003 = ORIENTED_EDGE ( 'NONE', *, *, #20230, .F. ) ;
#17004 = CARTESIAN_POINT ( 'NONE',  ( -26.65769201652798870, -1.128111410740069376, -16.27386567072153412 ) ) ;
#17005 = EDGE_CURVE ( 'NONE', #2692, #17841, #21875, .T. ) ;
#17006 = CARTESIAN_POINT ( 'NONE',  ( -10.34254640628522992, 25.37474234118948502, 19.99202127657103389 ) ) ;
#17007 = ORIENTED_EDGE ( 'NONE', *, *, #13952, .T. ) ;
#17008 = FACE_OUTER_BOUND ( 'NONE', #1722, .T. ) ;
#17009 = DIRECTION ( 'NONE',  ( 1.000000000000000000, 0.000000000000000000, 0.000000000000000000 ) ) ;
#17010 = B_SPLINE_CURVE_WITH_KNOTS ( 'NONE', 3,
 ( #37333, #21491, #18453, #18652, #3008, #30843, #40175, #37135, #3602, #19437, #16198, #22280, #28582, #12941, #37535, #10501, #25135, #756 ),
 .UNSPECIFIED., .F., .F.,
 ( 4, 2, 2, 2, 2, 2, 2, 2, 4 ),
 ( 0.000000000000000000, 0.1249999999999998335, 0.2499999999999996669, 0.3749999999999995004, 0.4999999999999993339, 0.6249999999999994449, 0.7499999999999996669, 0.8749999999999997780, 1.000000000000000000 ),
 .UNSPECIFIED. ) ;
#17011 = DIRECTION ( 'NONE',  ( 0.000000000000000000, 0.000000000000000000, 1.000000000000000000 ) ) ;
#17012 = CARTESIAN_POINT ( 'NONE',  ( 19.09512323183120941, -9.087989146580193633, -26.26778683489222033 ) ) ;
#17013 = CARTESIAN_POINT ( 'NONE',  ( 37.03648387062805369, -7.065924075331559528, 12.14047268033105098 ) ) ;
#17014 = VERTEX_POINT ( 'NONE', #9499 ) ;
#17015 = DIRECTION ( 'NONE',  ( 1.000000000000000000, 0.000000000000000000, 0.000000000000000000 ) ) ;
#17016 = DIRECTION ( 'NONE',  ( 0.000000000000000000, 0.000000000000000000, 1.000000000000000000 ) ) ;
#17017 = FACE_OUTER_BOUND ( 'NONE', #36101, .T. ) ;
#17018 = DIRECTION ( 'NONE',  ( 0.000000000000000000, 0.000000000000000000, -1.000000000000000000 ) ) ;
#17019 = CARTESIAN_POINT ( 'NONE',  ( -0.5717484631679848883, 29.10109329946823209, -16.62448788259939647 ) ) ;
#17020 = DIRECTION ( 'NONE',  ( -0.7032331762533995390, -0.07391278520355930304, -0.7071067811865530128 ) ) ;
#17021 = EDGE_CURVE ( 'NONE', #30083, #17070, #33888, .T. ) ;
#17022 = DIRECTION ( 'NONE',  ( 0.000000000000000000, 0.000000000000000000, 1.000000000000000000 ) ) ;
#17023 = CIRCLE ( 'NONE', #21535, 0.5000000000000004441 ) ;
#17024 = ADVANCED_FACE ( 'NONE', ( #22270 ), #2435, .T. ) ;
#17025 = DIRECTION ( 'NONE',  ( 1.000000000000000000, 0.000000000000000000, 0.000000000000000000 ) ) ;
#17026 = PLANE ( 'NONE',  #10005 ) ;
#17027 = DIRECTION ( 'NONE',  ( 0.000000000000000000, 0.000000000000000000, 1.000000000000000000 ) ) ;
#17028 = CARTESIAN_POINT ( 'NONE',  ( 13.89517812676522190, 27.95167899239444154, -10.04991680958497291 ) ) ;
#17029 = CARTESIAN_POINT ( 'NONE',  ( -12.53339520833721110, 14.68649063341707972, 10.94611345180490680 ) ) ;
#17030 = ORIENTED_EDGE ( 'NONE', *, *, #34050, .T. ) ;
#17031 = VECTOR ( 'NONE', #34925, 999.9999999999998863 ) ;
#17033 = CARTESIAN_POINT ( 'NONE',  ( -12.14070168820776274, 14.52831216351308541, 10.66666666666666430 ) ) ;
#17032 = CARTESIAN_POINT ( 'NONE',  ( -20.04575374383065878, 13.19209304670532568, -11.88046426404956257 ) ) ;
#17034 = CARTESIAN_POINT ( 'NONE',  ( -0.9658050764552030820, 37.18846563620834189, 10.49999999999999822 ) ) ;
#17035 = CARTESIAN_POINT ( 'NONE',  ( 15.48339541183756296, -26.71562014373387939, -5.945909248297312821 ) ) ;
#17036 = CARTESIAN_POINT ( 'NONE',  ( 8.694801740383951483, 1.741858881503470569, 11.00000000000000000 ) ) ;
#17037 = CARTESIAN_POINT ( 'NONE',  ( 14.01165143047478878, 23.97925642646874422, -13.50911357394699408 ) ) ;
#17038 = CARTESIAN_POINT ( 'NONE',  ( -11.10756861982300947, 19.59949212537556562, -20.90349153980999830 ) ) ;
#17039 = B_SPLINE_CURVE_WITH_KNOTS ( 'NONE', 3,
 ( #30332, #27672, #24031, #14691 ),
 .UNSPECIFIED., .F., .F.,
 ( 4, 4 ),
 ( 0.000000000000000000, 1.000000000000000000 ),
 .UNSPECIFIED. ) ;
#17040 = DIRECTION ( 'NONE',  ( -0.000000000000000000, 0.000000000000000000, -1.000000000000000000 ) ) ;
#17041 = CARTESIAN_POINT ( 'NONE',  ( -27.28398544816837301, -24.17053003994573501, -8.444893248965209764 ) ) ;
#17042 = AXIS2_PLACEMENT_3D ( 'NONE', #25442, #31947, #29107 ) ;
#17043 = CARTESIAN_POINT ( 'NONE',  ( 2.765300921622650066, -20.42095854668841781, -28.28989953578760819 ) ) ;
#17044 = CARTESIAN_POINT ( 'NONE',  ( 15.23366524578394454, 25.71175763003608594, -8.771869565430169047 ) ) ;
#17045 = CARTESIAN_POINT ( 'NONE',  ( 20.95229438974030955, 12.90995417087104435, -7.918639165910762223 ) ) ;
#17046 = CYLINDRICAL_SURFACE ( 'NONE', #28990, 1.000000000000000888 ) ;
#17047 = VERTEX_POINT ( 'NONE', #12339 ) ;
#17048 = CARTESIAN_POINT ( 'NONE',  ( -5.786258051655946311, 33.33688689327384935, -12.01593827444259510 ) ) ;
#17049 = ORIENTED_EDGE ( 'NONE', *, *, #5045, .F. ) ;
#17050 = ADVANCED_FACE ( 'NONE', ( #6241 ), #24727, .T. ) ;
#17051 = DIRECTION ( 'NONE',  ( 0.5254827454987599511, 0.4731467892558155475, -0.7071067811865464625 ) ) ;
#17052 = ORIENTED_EDGE ( 'NONE', *, *, #10865, .T. ) ;
#17053 = CARTESIAN_POINT ( 'NONE',  ( -0.3582326297815359162, 33.31072022568110924, 13.00000000000000178 ) ) ;
#17054 = AXIS2_PLACEMENT_3D ( 'NONE', #4906, #33153, #20354 ) ;
#17055 = EDGE_CURVE ( 'NONE', #27384, #1404, #28056, .T. ) ;
#17056 = DIRECTION ( 'NONE',  ( -1.000000000000000000, 0.000000000000000000, 0.000000000000000000 ) ) ;
#17057 = ORIENTED_EDGE ( 'NONE', *, *, #7889, .F. ) ;
#17058 = CARTESIAN_POINT ( 'NONE',  ( -30.46048998099726290, 0.1440795296772170719, -7.358614350216769573 ) ) ;
#17059 = ORIENTED_EDGE ( 'NONE', *, *, #16715, .F. ) ;
#17060 = CARTESIAN_POINT ( 'NONE',  ( 26.21350394291775388, -7.054572422158140732, -17.77726368305027194 ) ) ;
#17061 = CIRCLE ( 'NONE', #22227, 0.5000000000000004441 ) ;
#17062 = EDGE_LOOP ( 'NONE', ( #19037, #27726 ) ) ;
#17063 = DIRECTION ( 'NONE',  ( 0.000000000000000000, 0.000000000000000000, 1.000000000000000000 ) ) ;
#17064 = CARTESIAN_POINT ( 'NONE',  ( 19.48557158514982746, -11.25000000000009415, -0.000000000000000000 ) ) ;
#17065 = ORIENTED_EDGE ( 'NONE', *, *, #1452, .T. ) ;
#17066 = LINE ( 'NONE', #29042, #35901 ) ;
#17067 = DIRECTION ( 'NONE',  ( 1.000000000000000000, 0.000000000000000000, 0.000000000000000000 ) ) ;
#17068 = CARTESIAN_POINT ( 'NONE',  ( 13.41665185498674973, 27.84207739518157609, 17.92354375535403577 ) ) ;
#17069 = CARTESIAN_POINT ( 'NONE',  ( -11.56932667689144267, 32.06810925246628585, 10.49999999999999822 ) ) ;
#17070 = VERTEX_POINT ( 'NONE', #24932 ) ;
#17071 = VECTOR ( 'NONE', #8777, 1000.000000000000000 ) ;
#17072 = DIRECTION ( 'NONE',  ( 0.000000000000000000, 0.000000000000000000, 1.000000000000000000 ) ) ;
#17073 = LINE ( 'NONE', #35757, #97 ) ;
#17074 = ADVANCED_FACE ( 'NONE', ( #12539 ), #18445, .F. ) ;
#17075 = DIRECTION ( 'NONE',  ( 1.000000000000000000, 0.000000000000000000, 0.000000000000000000 ) ) ;
#17076 = EDGE_CURVE ( 'NONE', #2950, #31370, #34675, .T. ) ;
#17077 = CARTESIAN_POINT ( 'NONE',  ( 18.30429174972384843, 17.59035370715124103, -9.358262485240686601 ) ) ;
#17078 = AXIS2_PLACEMENT_3D ( 'NONE', #39399, #11580, #36363 ) ;
#17079 = CARTESIAN_POINT ( 'NONE',  ( 11.69942483974685921, 33.41113235942790993, -5.889308325164201108 ) ) ;
#17080 = ORIENTED_EDGE ( 'NONE', *, *, #2442, .T. ) ;
#17081 = LINE ( 'NONE', #1234, #28738 ) ;
#17082 = DIRECTION ( 'NONE',  ( 0.000000000000000000, 0.000000000000000000, -1.000000000000000000 ) ) ;
#17083 = CIRCLE ( 'NONE', #33304, 15.00000000000000000 ) ;
#17084 = CARTESIAN_POINT ( 'NONE',  ( 13.44501532575884717, -23.11853366065025739, -15.40642888925075127 ) ) ;
#17085 = PLANE ( 'NONE',  #29503 ) ;
#17086 = DIRECTION ( 'NONE',  ( -0.4156269377774634011, 0.5720614028176739252, -0.7071067811865500152 ) ) ;
#17087 = VERTEX_POINT ( 'NONE', #16191 ) ;
#17088 = CARTESIAN_POINT ( 'NONE',  ( -15.01279892861110987, 25.98643013970960780, -9.237413099304763620 ) ) ;
#17089 = VECTOR ( 'NONE', #9563, 1000.000000000000000 ) ;
#17090 = CARTESIAN_POINT ( 'NONE',  ( -18.93291711864322480, -26.86907612099998133, 16.87380292611481991 ) ) ;
#17091 = CARTESIAN_POINT ( 'NONE',  ( 14.88344483570274335, -26.39785593533024155, -7.359431359455702371 ) ) ;
#17092 = CARTESIAN_POINT ( 'NONE',  ( 0.2474667741973399226, 28.36888560440311480, 12.00000000000000000 ) ) ;
#17093 = VERTEX_POINT ( 'NONE', #34282 ) ;
#17094 = ORIENTED_EDGE ( 'NONE', *, *, #1920, .T. ) ;
#17095 = CARTESIAN_POINT ( 'NONE',  ( -9.677466622934531415, 26.64163155314981068, -15.96543401049129507 ) ) ;
#17096 = CARTESIAN_POINT ( 'NONE',  ( 4.155936879284735319, 47.29106893214565588, 9.500000000000000000 ) ) ;
#17097 = ADVANCED_FACE ( 'NONE', ( #15389 ), #20597, .T. ) ;
#17098 = AXIS2_PLACEMENT_3D ( 'NONE', #17835, #27359, #2386 ) ;
#17099 = FACE_BOUND ( 'NONE', #34930, .T. ) ;
#17100 = CARTESIAN_POINT ( 'NONE',  ( -28.07610024992567332, -6.064277111074432014, -15.90283520499208691 ) ) ;
#17101 = LINE ( 'NONE', #35984, #29308 ) ;
#17102 = ORIENTED_EDGE ( 'NONE', *, *, #367, .F. ) ;
#17103 = CARTESIAN_POINT ( 'NONE',  ( 27.64211024490576207, 0.3180281332077250500, -13.52072714143753096 ) ) ;
#17104 = EDGE_CURVE ( 'NONE', #31085, #26783, #6436, .T. ) ;
#17105 = CARTESIAN_POINT ( 'NONE',  ( -10.73132186042470160, 32.83534196859154974, 10.82238861112338490 ) ) ;
#17106 = DIRECTION ( 'NONE',  ( -0.5720614028176844723, -0.4156269377774491347, -0.7071067811865499042 ) ) ;
#17107 = CARTESIAN_POINT ( 'NONE',  ( -2.046188276595982014, 8.063706679521100540, 10.49999999999999822 ) ) ;
#17108 = ORIENTED_EDGE ( 'NONE', *, *, #40024, .T. ) ;
#17109 = CARTESIAN_POINT ( 'NONE',  ( -29.60645524828415276, 0.03829841260466283065, -10.17951810148429637 ) ) ;
#17110 = FACE_OUTER_BOUND ( 'NONE', #7869, .T. ) ;
#17111 = ORIENTED_EDGE ( 'NONE', *, *, #35746, .T. ) ;
#17112 = CARTESIAN_POINT ( 'NONE',  ( 21.44822029382961404, -1.048543745050170450, -24.81695474169817928 ) ) ;
#17113 = CIRCLE ( 'NONE', #39133, 1.000000000000000000 ) ;
#17114 = EDGE_CURVE ( 'NONE', #23396, #24869, #11594, .T. ) ;
#17115 = CARTESIAN_POINT ( 'NONE',  ( 32.21892379115691796, -22.89377427927269792, 14.53008259254040269 ) ) ;
#17116 = ORIENTED_EDGE ( 'NONE', *, *, #20058, .T. ) ;
#17117 = STYLED_ITEM ( 'NONE', ( #11966 ), #19702 ) ;
#17118 = CARTESIAN_POINT ( 'NONE',  ( -5.109761443619218468, 37.66877327392096220, 16.30093088680190760 ) ) ;
#17119 = CARTESIAN_POINT ( 'NONE',  ( 11.06125417662034316, -21.75993793940401133, 19.27171037444025359 ) ) ;
#17120 = CARTESIAN_POINT ( 'NONE',  ( -9.031213237790245429, -0.7484781929866335393, 9.500000000000000000 ) ) ;
#17121 = CARTESIAN_POINT ( 'NONE',  ( 5.712781365378005738, 28.53852268908861589, 20.69868183039781329 ) ) ;
#17122 = CIRCLE ( 'NONE', #13858, 1.000000000000000888 ) ;
#17123 = FACE_OUTER_BOUND ( 'NONE', #38664, .T. ) ;
#17124 = ORIENTED_EDGE ( 'NONE', *, *, #27301, .T. ) ;
#17125 = DIRECTION ( 'NONE',  ( 1.000000000000000000, 0.000000000000000000, 0.000000000000000000 ) ) ;
#17126 = ADVANCED_FACE ( 'NONE', ( #12934 ), #14762, .T. ) ;
#17127 = EDGE_CURVE ( 'NONE', #6337, #28188, #25922, .T. ) ;
#17128 = CARTESIAN_POINT ( 'NONE',  ( 4.995981679244292373, 37.69300919626899571, -5.860311672130957383 ) ) ;
#17129 = DIRECTION ( 'NONE',  ( -0.4067366430758047602, -0.9135454576425988682, 7.055756032835973512E-16 ) ) ;
#17130 = VECTOR ( 'NONE', #1681, 1000.000000000000000 ) ;
#17131 = CARTESIAN_POINT ( 'NONE',  ( 20.03472765055001759, 11.56705540218561268, 17.92354375535250810 ) ) ;
#17132 = CARTESIAN_POINT ( 'NONE',  ( 13.75932650634318399, -16.19533518725610577, -25.84441635423754136 ) ) ;
#17133 = CYLINDRICAL_SURFACE ( 'NONE', #29475, 0.5000000000000006661 ) ;
#17134 = DIRECTION ( 'NONE',  ( 1.000000000000000000, 0.000000000000000000, 0.000000000000000000 ) ) ;
#17135 = CARTESIAN_POINT ( 'NONE',  ( -9.294006203984645609, 33.46401007850805343, 6.000000000000000000 ) ) ;
#17136 = CARTESIAN_POINT ( 'NONE',  ( 12.87995330630399060, 21.73368077170972512, -17.42658506456785261 ) ) ;
#17137 = VECTOR ( 'NONE', #24509, 1000.000000000000000 ) ;
#17138 = ORIENTED_EDGE ( 'NONE', *, *, #32251, .F. ) ;
#17139 = CARTESIAN_POINT ( 'NONE',  ( -11.48487407195851695, 17.12429978707877254, -28.10317327323546976 ) ) ;
#17140 = CARTESIAN_POINT ( 'NONE',  ( -19.10349291421378837, -22.04058051679151831, 19.99202127657131101 ) ) ;
#17141 = CARTESIAN_POINT ( 'NONE',  ( -14.03291393139908649, 26.53383901973369774, 10.99387789255785641 ) ) ;
#17142 = CARTESIAN_POINT ( 'NONE',  ( 13.24447573026784397, 22.17338430882927724, -16.44949393079923894 ) ) ;
#17143 = EDGE_LOOP ( 'NONE', ( #32402, #369, #27199, #4943 ) ) ;
#17144 = CARTESIAN_POINT ( 'NONE',  ( 17.87465767731121957, -11.31086339180266798, -26.25773876253557759 ) ) ;
#17145 = ORIENTED_EDGE ( 'NONE', *, *, #17641, .F. ) ;
#17147 = DIRECTION ( 'NONE',  ( -0.000000000000000000, -0.000000000000000000, 1.000000000000000000 ) ) ;
#17146 = CARTESIAN_POINT ( 'NONE',  ( -12.74236390228968041, 21.95782657198702736, -17.39615765752699517 ) ) ;
#17148 = CARTESIAN_POINT ( 'NONE',  ( -11.66927690283585228, -19.78180214246283697, -21.50613042839750833 ) ) ;
#17149 = DIRECTION ( 'NONE',  ( 0.000000000000000000, 0.000000000000000000, -1.000000000000000000 ) ) ;
#17150 =( REPRESENTATION_RELATIONSHIP ('NONE','NONE', #15382, #33787 ) REPRESENTATION_RELATIONSHIP_WITH_TRANSFORMATION ( #5653 )SHAPE_REPRESENTATION_RELATIONSHIP( ) );
#17151 = AXIS2_PLACEMENT_3D ( 'NONE', #36305, #14360, #36897 ) ;
#17152 = ORIENTED_EDGE ( 'NONE', *, *, #27047, .T. ) ;
#17153 = CARTESIAN_POINT ( 'NONE',  ( -21.02740630788312259, -8.711873245778782859, -23.03796868434001865 ) ) ;
#17154 = CARTESIAN_POINT ( 'NONE',  ( -12.62124997321451048, -23.07266609165860771, -15.47605775495894243 ) ) ;
#17155 = CARTESIAN_POINT ( 'NONE',  ( 39.51968005975199105, -13.07391886567316774, 22.99999999999999645 ) ) ;
#17156 = CARTESIAN_POINT ( 'NONE',  ( 13.79761723546635643, 16.77350094813697368, -23.03736194697137307 ) ) ;
#17157 = ORIENTED_EDGE ( 'NONE', *, *, #17566, .T. ) ;
#17158 = CARTESIAN_POINT ( 'NONE',  ( 27.31048934271396433, 3.779197449542496035, -6.904998494663478148 ) ) ;
#17159 = EDGE_CURVE ( 'NONE', #12954, #22450, #35482, .T. ) ;
#17160 = FACE_OUTER_BOUND ( 'NONE', #14403, .T. ) ;
#17161 = CARTESIAN_POINT ( 'NONE',  ( -23.05386822411328041, -7.747535282638268406, 23.00000000000000000 ) ) ;
#17162 = ORIENTED_EDGE ( 'NONE', *, *, #21242, .F. ) ;
#17163 = CARTESIAN_POINT ( 'NONE',  ( -21.30018192981278347, 0.6028086581825573553, -24.99559268264187750 ) ) ;
#17164 = CARTESIAN_POINT ( 'NONE',  ( 28.75502359630104721, -0.3820146305305825440, -12.49841367032799866 ) ) ;
#17165 = AXIS2_PLACEMENT_3D ( 'NONE', #38143, #10516, #16218 ) ;
#17166 = CARTESIAN_POINT ( 'NONE',  ( 29.15792305772562898, -20.09428552990231509, 18.87996532025821494 ) ) ;
#17167 = ORIENTED_EDGE ( 'NONE', *, *, #4437, .T. ) ;
#17168 = CARTESIAN_POINT ( 'NONE',  ( -28.09305766860465425, 2.631505933142144649, -7.850560883495491638 ) ) ;
#17169 = CARTESIAN_POINT ( 'NONE',  ( 15.29245034862073460, 32.56469986092002955, -13.99876745781544685 ) ) ;
#17170 = VECTOR ( 'NONE', #22057, 1000.000000000000000 ) ;
#17171 = CARTESIAN_POINT ( 'NONE',  ( 1.623731701744046241, 25.43444280220171194, 12.00000000000000000 ) ) ;
#17172 = FACE_OUTER_BOUND ( 'NONE', #38201, .T. ) ;
#17173 = AXIS2_PLACEMENT_3D ( 'NONE', #20571, #29149, #32965 ) ;
#17174 = FACE_OUTER_BOUND ( 'NONE', #10217, .T. ) ;
#17175 = CARTESIAN_POINT ( 'NONE',  ( 14.64210930126480115, 24.20081211342298744, 12.00000000000000000 ) ) ;
#17176 = CARTESIAN_POINT ( 'NONE',  ( -7.713869163866016621, 10.18146832927085121, 7.500000000000000888 ) ) ;
#17177 = VERTEX_POINT ( 'NONE', #23083 ) ;
#17178 = CARTESIAN_POINT ( 'NONE',  ( -24.40045231895073385, 6.107632861236318433, -11.80004717437143746 ) ) ;
#17179 = DIRECTION ( 'NONE',  ( -1.224646799147351235E-16, 1.000000000000000000, 0.000000000000000000 ) ) ;
#17180 = CARTESIAN_POINT ( 'NONE',  ( 16.72075857324119141, 7.444561356925491147, 7.000000000000000000 ) ) ;
#17181 = CARTESIAN_POINT ( 'NONE',  ( 27.56730585349385620, -23.98784956095697396, -8.441368152517451762 ) ) ;
#17182 = EDGE_CURVE ( 'NONE', #32385, #18932, #28976, .T. ) ;
#17183 = FACE_OUTER_BOUND ( 'NONE', #9437, .T. ) ;
#17184 = CARTESIAN_POINT ( 'NONE',  ( -14.86556419889030778, 20.43481210330130082, 10.59344459855562270 ) ) ;
#17185 = CARTESIAN_POINT ( 'NONE',  ( 15.26389162175653880, 27.29890105065966921, -4.999999999999999112 ) ) ;
#17186 = CARTESIAN_POINT ( 'NONE',  ( -5.982165713378355676, 28.55918256678905820, 9.000000000000001776 ) ) ;
#17187 = VERTEX_POINT ( 'NONE', #32645 ) ;
#17188 = CARTESIAN_POINT ( 'NONE',  ( -17.31869546780055558, 18.97017784545571573, -10.80183007974773624 ) ) ;
#17189 = CARTESIAN_POINT ( 'NONE',  ( -25.22909892406959997, -10.52103384677036502, 20.99999999999999645 ) ) ;
#17190 = CARTESIAN_POINT ( 'NONE',  ( 15.33814677726094189, -26.70409432335911859, -5.000000000000000888 ) ) ;
#17191 = DIRECTION ( 'NONE',  ( -1.000000000000000000, 0.000000000000000000, 0.000000000000000000 ) ) ;
#17192 = CARTESIAN_POINT ( 'NONE',  ( 11.08133522239378088, 17.49689473911582027, -27.44844487583075221 ) ) ;
#17193 = ORIENTED_EDGE ( 'NONE', *, *, #10144, .T. ) ;
#17194 = CARTESIAN_POINT ( 'NONE',  ( 11.03000241580673979, 17.43158562307755943, -28.07681393002727077 ) ) ;
#17195 = ORIENTED_EDGE ( 'NONE', *, *, #9642, .F. ) ;
#17197 = DIRECTION ( 'NONE',  ( 0.000000000000000000, 0.000000000000000000, -1.000000000000000000 ) ) ;
#17196 = CARTESIAN_POINT ( 'NONE',  ( -15.30416065479365351, 26.73672882626205194, -6.885395080861467676 ) ) ;
#17198 = CARTESIAN_POINT ( 'NONE',  ( -11.14927767355199784, -20.47484563554826664, -20.54567832761641100 ) ) ;
#17199 = CARTESIAN_POINT ( 'NONE',  ( -36.53368004180960327, -5.154483866377498558, 11.00000000000028955 ) ) ;
#17200 = CARTESIAN_POINT ( 'NONE',  ( -29.68001125634650705, -19.19152806808636313, -11.07052693527171705 ) ) ;
#17201 = CARTESIAN_POINT ( 'NONE',  ( -6.807649496723200855, -24.62777695444815151, -9.837064774307107129 ) ) ;
#17202 = CARTESIAN_POINT ( 'NONE',  ( 15.77104256730297749, 25.16267426227344828, -6.891571856456937262 ) ) ;
#17203 = ORIENTED_EDGE ( 'NONE', *, *, #40153, .T. ) ;
#17204 = CARTESIAN_POINT ( 'NONE',  ( 24.02933105728603991, 8.309275822838595005, -5.000000000000000000 ) ) ;
#17205 = CARTESIAN_POINT ( 'NONE',  ( -18.68939205906154655, 29.94303747981212993, 11.00000000000000178 ) ) ;
#17206 = CARTESIAN_POINT ( 'NONE',  ( 0.5000000000000000000, 37.04625217320466390, 10.99999999999999645 ) ) ;
#17207 = CARTESIAN_POINT ( 'NONE',  ( 8.935770203493859754, 22.34671014717335780, 13.00000000000000178 ) ) ;
#17208 = AXIS2_PLACEMENT_3D ( 'NONE', #6804, #37506, #37304 ) ;
#17209 = EDGE_LOOP ( 'NONE', ( #155, #26559, #7918, #24622 ) ) ;
#17210 = CARTESIAN_POINT ( 'NONE',  ( -20.53668341592966939, -1.131593473639494807, -28.63651727350685050 ) ) ;
#17211 = VECTOR ( 'NONE', #7665, 1000.000000000000000 ) ;
#17212 = CARTESIAN_POINT ( 'NONE',  ( -16.18987435794524288, 9.347228318705029793, 20.25080042701566541 ) ) ;
#17213 = CARTESIAN_POINT ( 'NONE',  ( 19.90456025098515624, -17.02442174103823191, 20.99999999999999645 ) ) ;
#17214 = DIRECTION ( 'NONE',  ( -1.000000000000000000, 0.000000000000000000, 0.000000000000000000 ) ) ;
#17215 = EDGE_CURVE ( 'NONE', #27796, #24757, #33617, .T. ) ;
#17216 = FACE_OUTER_BOUND ( 'NONE', #16010, .T. ) ;
#17217 = CARTESIAN_POINT ( 'NONE',  ( 34.23814126792781565, -17.55187814006816538, -4.999999999999996447 ) ) ;
#17218 = CARTESIAN_POINT ( 'NONE',  ( 28.24711154207343000, -27.09388640670305293, 11.00000000000010481 ) ) ;
#17219 = ORIENTED_EDGE ( 'NONE', *, *, #18087, .T. ) ;
#17220 = DIRECTION ( 'NONE',  ( -0.000000000000000000, -0.000000000000000000, -1.000000000000000000 ) ) ;
#17221 = AXIS2_PLACEMENT_3D ( 'NONE', #3427, #19464, #34315 ) ;
#17222 = DIRECTION ( 'NONE',  ( 1.000000000000000000, 0.000000000000000000, 0.000000000000000000 ) ) ;
#17223 = ORIENTED_EDGE ( 'NONE', *, *, #28496, .F. ) ;
#17224 = CARTESIAN_POINT ( 'NONE',  ( 0.4114189264675333080, 38.49512827994399800, -5.435433640322397508 ) ) ;
#17225 = CARTESIAN_POINT ( 'NONE',  ( -14.99497092072327220, 22.09096420981882503, 7.202682876670051471 ) ) ;
#17226 = EDGE_CURVE ( 'NONE', #26836, #13142, #22472, .T. ) ;
#17227 = CARTESIAN_POINT ( 'NONE',  ( -2.118678732975735279, 7.827785988993307242, 13.00000000000000178 ) ) ;
#17228 = CIRCLE ( 'NONE', #12021, 0.5000000000000000000 ) ;
#17229 = DIRECTION ( 'NONE',  ( -0.000000000000000000, -0.000000000000000000, -1.000000000000000000 ) ) ;
#17231 = DIRECTION ( 'NONE',  ( -0.000000000000000000, 1.000000000000000000, -0.000000000000000000 ) ) ;
#17230 = PRODUCT_DEFINITION ( 'UNKNOWN', '', #6074, #36631 ) ;
#17232 = DIRECTION ( 'NONE',  ( 0.000000000000000000, 0.000000000000000000, 1.000000000000000000 ) ) ;
#17233 = CARTESIAN_POINT ( 'NONE',  ( 12.88278855606390394, 23.95175969909016089, -15.32450620224983950 ) ) ;
#17235 = VECTOR ( 'NONE', #18619, 1000.000000000000000 ) ;
#17234 = CARTESIAN_POINT ( 'NONE',  ( 11.77090408390491305, 15.39748370681878775, 6.000000000000000000 ) ) ;
#17236 = ORIENTED_EDGE ( 'NONE', *, *, #34105, .F. ) ;
#17239 = FACE_OUTER_BOUND ( 'NONE', #19428, .T. ) ;
#17238 = CIRCLE ( 'NONE', #34102, 0.5000000000000013323 ) ;
#17237 = CARTESIAN_POINT ( 'NONE',  ( -19.45999784437984914, 12.76325622095678725, -14.91856487225177474 ) ) ;
#17240 = EDGE_CURVE ( 'NONE', #3455, #12932, #24495, .T. ) ;
#17241 = CARTESIAN_POINT ( 'NONE',  ( 9.427394655428274817, 11.06314620770945290, 7.500000000000000888 ) ) ;
#17242 = CARTESIAN_POINT ( 'NONE',  ( 15.52090202525632279, -26.75102145164868972, -5.474045156224585540 ) ) ;
#17243 = EDGE_CURVE ( 'NONE', #2054, #18869, #38794, .T. ) ;
#17244 = DIRECTION ( 'NONE',  ( -0.4067366430757888840, 0.9135454576426059736, 0.000000000000000000 ) ) ;
#17245 = CARTESIAN_POINT ( 'NONE',  ( 14.82688042600062239, 25.65053735475629182, -10.17772289843519573 ) ) ;
#17246 = CARTESIAN_POINT ( 'NONE',  ( -18.07620401364299667, 24.68088026512193522, -5.000000000000000000 ) ) ;
#17247 = CARTESIAN_POINT ( 'NONE',  ( -3.476907992048017260, 18.63850621467409496, 13.00000000000000178 ) ) ;
#17248 = CARTESIAN_POINT ( 'NONE',  ( -19.89493131341646048, -18.69241546286294309, -17.73959074223588317 ) ) ;
#17249 = CARTESIAN_POINT ( 'NONE',  ( 2.901613786040809551, -20.88678771515551702, -24.38864445180290375 ) ) ;
#17250 = CARTESIAN_POINT ( 'NONE',  ( 12.54845838944650183, 20.28352347061387917, -19.52372391363399728 ) ) ;
#17251 = CARTESIAN_POINT ( 'NONE',  ( 18.20215074981739889, 13.29937655356881265, -17.99813131470672900 ) ) ;
#17252 = CARTESIAN_POINT ( 'NONE',  ( -1.693998953219646442, 12.12549434688617822, 10.00000000000000000 ) ) ;
#17253 = VERTEX_POINT ( 'NONE', #26334 ) ;
#17254 = CARTESIAN_POINT ( 'NONE',  ( -4.991427726885995675, 21.31633811110100041, -24.36793799711855968 ) ) ;
#17255 = ORIENTED_EDGE ( 'NONE', *, *, #996, .F. ) ;
#17256 = DIRECTION ( 'NONE',  ( 1.000000000000000000, 0.000000000000000000, 0.000000000000000000 ) ) ;
#17257 = ORIENTED_EDGE ( 'NONE', *, *, #11017, .T. ) ;
#17258 = DIRECTION ( 'NONE',  ( 0.000000000000000000, 0.000000000000000000, 1.000000000000000000 ) ) ;
#17259 = EDGE_CURVE ( 'NONE', #12080, #39537, #4800, .T. ) ;
#17260 = DIRECTION ( 'NONE',  ( -0.000000000000000000, -0.000000000000000000, -1.000000000000000000 ) ) ;
#17261 = EDGE_CURVE ( 'NONE', #1450, #35955, #38728, .T. ) ;
#17262 = ORIENTED_EDGE ( 'NONE', *, *, #21542, .T. ) ;
#17263 = AXIS2_PLACEMENT_3D ( 'NONE', #25410, #6715, #28266 ) ;
#17264 = CARTESIAN_POINT ( 'NONE',  ( -30.68739395818431959, 0.1797671858537340517, -4.999999999999999112 ) ) ;
#17265 = VERTEX_POINT ( 'NONE', #22672 ) ;
#17266 = CARTESIAN_POINT ( 'NONE',  ( 33.70584737762637673, -11.25103427847470172, -9.773660813979208939 ) ) ;
#17267 = AXIS2_PLACEMENT_3D ( 'NONE', #20622, #2723, #5368 ) ;
#17268 = VECTOR ( 'NONE', #20737, 1000.000000000000114 ) ;
#17269 = CIRCLE ( 'NONE', #10116, 57.99999999999995026 ) ;
#17270 = ORIENTED_EDGE ( 'NONE', *, *, #2196, .F. ) ;
#17271 = ITEM_DEFINED_TRANSFORMATION ( 'NONE', 'NONE', #37847,  #24238 ) ;
#17272 = CARTESIAN_POINT ( 'NONE',  ( 1.494936919103933226, 34.23777120880591696, 13.00000000000000178 ) ) ;
#17273 = ORIENTED_EDGE ( 'NONE', *, *, #24715, .T. ) ;
#17274 = DIRECTION ( 'NONE',  ( 0.000000000000000000, 0.000000000000000000, -1.000000000000000000 ) ) ;
#17275 = CARTESIAN_POINT ( 'NONE',  ( 3.863783140547853712E-14, -86.77689918168233874, -0.000000000000000000 ) ) ;
#17276 = CARTESIAN_POINT ( 'NONE',  ( -10.52847790146128126, 31.43738312353774234, 18.42518152272106491 ) ) ;
#17277 = CARTESIAN_POINT ( 'NONE',  ( 12.99377146717206344, 26.19620116591418224, 10.00000000000000000 ) ) ;
#17278 = ORIENTED_EDGE ( 'NONE', *, *, #16213, .T. ) ;
#17279 = SHAPE_REPRESENTATION_RELATIONSHIP ( 'NONE' , 'NONE' ,  #12760, #19702 ) ;
#17280 = DIRECTION ( 'NONE',  ( 0.6724985119639563802, -0.2185080122244180134, 0.7071067811865461294 ) ) ;
#17281 = FACE_OUTER_BOUND ( 'NONE', #13090, .T. ) ;
#17282 = CARTESIAN_POINT ( 'NONE',  ( 14.06524961900336734, 27.71236540882597410, 7.000000000000000000 ) ) ;
#17283 = EDGE_CURVE ( 'NONE', #8510, #24176, #21304, .T. ) ;
#17284 = CARTESIAN_POINT ( 'NONE',  ( 19.07008944147191443, 16.95185708702321747, -5.480395098389816866 ) ) ;
#17285 = CARTESIAN_POINT ( 'NONE',  ( 8.205360533218383878, 25.51929248090862501, -17.85775526361365806 ) ) ;
#17286 = ORIENTED_EDGE ( 'NONE', *, *, #2330, .F. ) ;
#17287 = CARTESIAN_POINT ( 'NONE',  ( 12.30736835487432757, 14.81698729810772441, 11.00000000000000000 ) ) ;
#17288 = FACE_OUTER_BOUND ( 'NONE', #31417, .T. ) ;
#17289 = CARTESIAN_POINT ( 'NONE',  ( 9.937768194491171769, -17.93102150851172993, -30.00000000000000000 ) ) ;
#17290 = DIRECTION ( 'NONE',  ( -0.000000000000000000, -0.000000000000000000, -1.000000000000000000 ) ) ;
#17291 = VECTOR ( 'NONE', #34767, 1000.000000000000000 ) ;
#17292 = FACE_OUTER_BOUND ( 'NONE', #16987, .T. ) ;
#17293 = ORIENTED_EDGE ( 'NONE', *, *, #38456, .T. ) ;
#17294 = CARTESIAN_POINT ( 'NONE',  ( -15.28567255210324838, 26.54645022884873384, -7.357307290646502018 ) ) ;
#17295 = CIRCLE ( 'NONE', #16647, 1.000000000000000000 ) ;
#17296 = CARTESIAN_POINT ( 'NONE',  ( -33.65490896085638184, -21.61118400457242572, 13.92931973827790770 ) ) ;
#17297 = CARTESIAN_POINT ( 'NONE',  ( 9.195945848978588799, -18.32167064559432035, -30.00000000000000000 ) ) ;
#17298 = DIRECTION ( 'NONE',  ( -1.000000000000000000, 0.000000000000000000, 0.000000000000000000 ) ) ;
#17299 = ORIENTED_EDGE ( 'NONE', *, *, #29729, .T. ) ;
#17300 = ORIENTED_EDGE ( 'NONE', *, *, #37180, .T. ) ;
#17301 = CARTESIAN_POINT ( 'NONE',  ( -7.104430329252444665, 19.30332660575202297, -28.55946829698027045 ) ) ;
#17302 = CARTESIAN_POINT ( 'NONE',  ( -13.05736835487441994, 16.11602540378456183, 10.49999999999999822 ) ) ;
#17303 = CARTESIAN_POINT ( 'NONE',  ( 1.000000000000000666, 33.00000000000000000, 10.50000000000000000 ) ) ;
#17304 = CARTESIAN_POINT ( 'NONE',  ( -20.91604292039119173, -3.820787406694753585, -25.84273227370559312 ) ) ;
#17305 = CARTESIAN_POINT ( 'NONE',  ( -9.665073660138979506, 25.11464168560200605, 10.49999999999999112 ) ) ;
#17306 = EDGE_LOOP ( 'NONE', ( #37110, #30445, #22213 ) ) ;
#17307 = CARTESIAN_POINT ( 'NONE',  ( 27.69998584925471619, 0.2404071644066830549, -13.51635162220101627 ) ) ;
#17308 = CARTESIAN_POINT ( 'NONE',  ( 3.118671991557230516, 37.17221401100731981, 6.000000000000000000 ) ) ;
#17309 = DIRECTION ( 'NONE',  ( 0.000000000000000000, 0.000000000000000000, 1.000000000000000000 ) ) ;
#17310 = DIRECTION ( 'NONE',  ( 0.5720614028176818078, -0.4156269377774653440, -0.7071067811865424657 ) ) ;
#17311 = ORIENTED_EDGE ( 'NONE', *, *, #12543, .T. ) ;
#17312 = CARTESIAN_POINT ( 'NONE',  ( -30.72389070028295777, -0.02887358500283720292, -6.887897371773664013 ) ) ;
#17313 = CARTESIAN_POINT ( 'NONE',  ( -9.160254037844421049, 18.36602540378452630, 10.49999999999999822 ) ) ;
#17315 = EDGE_CURVE ( 'NONE', #18367, #33916, #26113, .T. ) ;
#17314 = ORIENTED_EDGE ( 'NONE', *, *, #13603, .T. ) ;
#17316 = CARTESIAN_POINT ( 'NONE',  ( 33.22294079836321856, -4.074934819707171307, -8.143877639058281659 ) ) ;
#17317 = CARTESIAN_POINT ( 'NONE',  ( 33.17211272335703143, -21.25822893968285854, 15.13084544680211430 ) ) ;
#17318 = ORIENTED_EDGE ( 'NONE', *, *, #30794, .F. ) ;
#17319 = CARTESIAN_POINT ( 'NONE',  ( -14.97435799694009795, 30.45328679654753756, 15.13084544680204147 ) ) ;
#17320 = CARTESIAN_POINT ( 'NONE',  ( 5.409649191045219574, -22.50706359516090060, 18.42518152272108978 ) ) ;
#17321 = DIRECTION ( 'NONE',  ( 0.6691306063588671194, 0.7431448254773861395, 0.000000000000000000 ) ) ;
#17322 = CARTESIAN_POINT ( 'NONE',  ( -2.374005179830599666, 29.54744178790028997, 20.82122704794079837 ) ) ;
#17323 = CIRCLE ( 'NONE', #40001, 1.000000000000000888 ) ;
#17324 = AXIS2_PLACEMENT_3D ( 'NONE', #11647, #33394, #10839 ) ;
#17325 = CARTESIAN_POINT ( 'NONE',  ( 13.01837422881150452, 21.26636931122159169, 13.00000000000000178 ) ) ;
#17326 = ORIENTED_EDGE ( 'NONE', *, *, #24297, .T. ) ;
#17327 = DIRECTION ( 'NONE',  ( 0.000000000000000000, 0.000000000000000000, 1.000000000000000000 ) ) ;
#17328 = EDGE_CURVE ( 'NONE', #38307, #38835, #17411, .T. ) ;
#17329 = CARTESIAN_POINT ( 'NONE',  ( 3.355814016059087468, 25.38759446419620147, -19.67824355085762278 ) ) ;
#17330 = CARTESIAN_POINT ( 'NONE',  ( -6.064571727552472424, 31.45661825943146894, 6.000000000000000000 ) ) ;
#17331 = EDGE_CURVE ( 'NONE', #34177, #18996, #5703, .T. ) ;
#17332 = CARTESIAN_POINT ( 'NONE',  ( 8.859192577249610068, 12.20922670554003631, 20.99999999999999645 ) ) ;
#17333 = CARTESIAN_POINT ( 'NONE',  ( 18.63134831210867404, -25.78775970246520188, -10.44478608498117289 ) ) ;
#17334 = CARTESIAN_POINT ( 'NONE',  ( 9.340438144417392508, 38.00965938232019425, 11.00000000000005329 ) ) ;
#17335 = CARTESIAN_POINT ( 'NONE',  ( 2.525645716490518389, 8.212903943950921715, 9.500000000000000000 ) ) ;
#17336 = CARTESIAN_POINT ( 'NONE',  ( 2.444768620639813594, 7.712926687590050179, 10.49999999999999822 ) ) ;
#17337 = VERTEX_POINT ( 'NONE', #33053 ) ;
#17338 = CARTESIAN_POINT ( 'NONE',  ( 15.37925838865456996, 26.91354363167639363, -5.473566364682137753 ) ) ;
#17339 = ORIENTED_EDGE ( 'NONE', *, *, #14981, .T. ) ;
#17340 = CARTESIAN_POINT ( 'NONE',  ( -14.94814311929064132, 25.28441830965897807, -10.18638070629203618 ) ) ;
#17341 = EDGE_CURVE ( 'NONE', #12427, #1970, #8289, .T. ) ;
#17342 = CARTESIAN_POINT ( 'NONE',  ( -17.81343984362097643, -22.72844136247609015, 19.66345542862531559 ) ) ;
#17343 = DIRECTION ( 'NONE',  ( 0.000000000000000000, 0.000000000000000000, 1.000000000000000000 ) ) ;
#17344 = CARTESIAN_POINT ( 'NONE',  ( 14.87527538485814027, 25.50334810396817176, -10.18232127768725626 ) ) ;
#17345 = ORIENTED_EDGE ( 'NONE', *, *, #12296, .T. ) ;
#17346 = CARTESIAN_POINT ( 'NONE',  ( 21.26206063148141467, -12.57871523600208441, -20.68868112704091189 ) ) ;
#17347 = ORIENTED_EDGE ( 'NONE', *, *, #17852, .T. ) ;
#17349 = LINE ( 'NONE', #35626, #36768 ) ;
#17348 = CARTESIAN_POINT ( 'NONE',  ( -14.44959290368749016, 27.62540214084364010, -9.158983685620894377 ) ) ;
#17350 = CARTESIAN_POINT ( 'NONE',  ( -10.42186838066264087, -18.08256185635291047, -26.76705096067638934 ) ) ;
#17351 = PLANE ( 'NONE',  #8207 ) ;
#17352 = CONICAL_SURFACE ( 'NONE', #14761, 1.000000000000005995, 0.7853981633974537191 ) ;
#17353 = VECTOR ( 'NONE', #37326, 1000.000000000000000 ) ;
#17354 = ORIENTED_EDGE ( 'NONE', *, *, #9753, .F. ) ;
#17355 = CARTESIAN_POINT ( 'NONE',  ( -19.46103219778806093, -6.726610151890429989, -28.47929083369243131 ) ) ;
#17356 = CARTESIAN_POINT ( 'NONE',  ( -14.92665030077538724, -26.52727164316652164, -6.417579119027339907 ) ) ;
#17357 = DIRECTION ( 'NONE',  ( 1.000000000000000000, 0.000000000000000000, 0.000000000000000000 ) ) ;
#17358 = CARTESIAN_POINT ( 'NONE',  ( 13.23034956895627268, 15.71535633465425619, -28.78767767912723130 ) ) ;
#17359 = ORIENTED_EDGE ( 'NONE', *, *, #38303, .T. ) ;
#17360 = CARTESIAN_POINT ( 'NONE',  ( 20.35897324780223272, 3.107494928291200331, -28.17405716974139196 ) ) ;
#17361 = FACE_OUTER_BOUND ( 'NONE', #30117, .T. ) ;
#17362 = CARTESIAN_POINT ( 'NONE',  ( -31.08218589456736680, -27.68808744833886948, 11.00000000000000000 ) ) ;
#17363 = EDGE_CURVE ( 'NONE', #21424, #14474, #1798, .T. ) ;
#17364 = ORIENTED_EDGE ( 'NONE', *, *, #38848, .T. ) ;
#17365 = EDGE_CURVE ( 'NONE', #16528, #1872, #19975, .T. ) ;
#17366 = CARTESIAN_POINT ( 'NONE',  ( -30.52913824356789618, -0.1914677198932651925, -8.288054658077042447 ) ) ;
#17367 = EDGE_CURVE ( 'NONE', #8916, #29799, #32954, .T. ) ;
#17368 = CARTESIAN_POINT ( 'NONE',  ( 31.23646475641210429, -0.5774691780063523350, -6.872549786655949511 ) ) ;
#17369 = CIRCLE ( 'NONE', #14766, 6.000000000000000888 ) ;
#17370 = CARTESIAN_POINT ( 'NONE',  ( 31.82690166321389924, -6.837813000313431644, 18.87996532025749374 ) ) ;
#17371 = ORIENTED_EDGE ( 'NONE', *, *, #16819, .F. ) ;
#17372 = CARTESIAN_POINT ( 'NONE',  ( -23.62278170705122449, 1.244602331402794304, -19.58093624668523347 ) ) ;
#17373 = CARTESIAN_POINT ( 'NONE',  ( -22.40982762235195835, 2.618079236897030704, -21.24786896499725231 ) ) ;
#17374 = CARTESIAN_POINT ( 'NONE',  ( 75.15099915297797395, 43.38844959084117647, 0.000000000000000000 ) ) ;
#17375 = DIRECTION ( 'NONE',  ( -0.9510565162951507556, 0.3090169943749560000, 0.000000000000000000 ) ) ;
#17376 = EDGE_CURVE ( 'NONE', #7792, #28710, #11503, .T. ) ;
#17377 = CIRCLE ( 'NONE', #37454, 1.000000000000000000 ) ;
#17378 = VECTOR ( 'NONE', #16595, 1000.000000000000000 ) ;
#17379 = DIRECTION ( 'NONE',  ( -0.6691306063588671194, -0.7431448254773861395, 0.000000000000000000 ) ) ;
#17380 = DIRECTION ( 'NONE',  ( 0.000000000000000000, 0.000000000000000000, 1.000000000000000000 ) ) ;
#17381 = EDGE_CURVE ( 'NONE', #4180, #29868, #6953, .T. ) ;
#17382 = LINE ( 'NONE', #30159, #36692 ) ;
#17383 = ORIENTED_EDGE ( 'NONE', *, *, #13517, .F. ) ;
#17384 = CARTESIAN_POINT ( 'NONE',  ( -21.96241518972654205, 5.878577984738289963, -18.91332339141946051 ) ) ;
#17385 = DIRECTION ( 'NONE',  ( -0.000000000000000000, -0.000000000000000000, -1.000000000000000000 ) ) ;
#17386 = DIRECTION ( 'NONE',  ( -0.000000000000000000, -0.000000000000000000, -1.000000000000000000 ) ) ;
#17387 = CARTESIAN_POINT ( 'NONE',  ( 16.73034041975913766, -16.38034227348617478, -22.03442445900950375 ) ) ;
#17388 = CIRCLE ( 'NONE', #27747, 1.000000000000000888 ) ;
#17389 = DIRECTION ( 'NONE',  ( 0.000000000000000000, 0.000000000000000000, 1.000000000000000000 ) ) ;
#17390 = CARTESIAN_POINT ( 'NONE',  ( -14.55889214498793471, 20.02072497456995137, 10.49999999999999822 ) ) ;
#17391 = CARTESIAN_POINT ( 'NONE',  ( 10.70229295774111478, 17.48483442551455269, -30.00000000000000000 ) ) ;
#17392 = AXIS2_PLACEMENT_3D ( 'NONE', #8248, #20654, #5205 ) ;
#17393 = EDGE_LOOP ( 'NONE', ( #10103, #5172, #9594, #31794 ) ) ;
#17394 = CARTESIAN_POINT ( 'NONE',  ( -15.84802793396828235, 21.63412679409943706, -11.70048637574523553 ) ) ;
#17395 = CARTESIAN_POINT ( 'NONE',  ( -0.5000000000000003331, 36.50000000000000711, 9.500000000000000000 ) ) ;
#17396 = CARTESIAN_POINT ( 'NONE',  ( 9.656026013581104905, -18.45733997954168260, -26.83334999707987834 ) ) ;
#17397 = LINE ( 'NONE', #20637, #11396 ) ;
#17398 = CARTESIAN_POINT ( 'NONE',  ( 12.40569181072914873, 20.47107099798277119, -19.49903299958157632 ) ) ;
#17399 = ORIENTED_EDGE ( 'NONE', *, *, #2043, .F. ) ;
#17400 = CARTESIAN_POINT ( 'NONE',  ( 10.98647152928299597, 17.30743895948370081, -30.00000000000000000 ) ) ;
#17401 = EDGE_LOOP ( 'NONE', ( #9869, #25721, #39592, #24778, #9187 ) ) ;
#17403 = CARTESIAN_POINT ( 'NONE',  ( -10.18324708981896087, 16.78440424842446532, 12.00000000000000000 ) ) ;
#17402 = CARTESIAN_POINT ( 'NONE',  ( -10.94140927258908746, 17.38955668528554810, -28.70426223197859628 ) ) ;
#17404 = CARTESIAN_POINT ( 'NONE',  ( -9.982340082043387852, -18.80733487794834247, -25.01271746743459801 ) ) ;
#17405 = CARTESIAN_POINT ( 'NONE',  ( -24.65531199400788509, -28.60128534115780141, 10.99999999999993427 ) ) ;
#17406 = CARTESIAN_POINT ( 'NONE',  ( -30.31686021207967840, -19.60108723602752079, -10.17585211697064551 ) ) ;
#17407 = CARTESIAN_POINT ( 'NONE',  ( -8.528322800344751542, -23.99199305410463978, -12.74934014457994813 ) ) ;
#17408 = CARTESIAN_POINT ( 'NONE',  ( 12.64274550584182677, 19.31738184857981722, -20.62888840247773459 ) ) ;
#17409 = VERTEX_POINT ( 'NONE', #23687 ) ;
#17410 = CARTESIAN_POINT ( 'NONE',  ( 19.41880252833811227, 6.610239277501288591, -30.00000000000000355 ) ) ;
#17411 = LINE ( 'NONE', #21239, #19297 ) ;
#17412 = LINE ( 'NONE', #17815, #24461 ) ;
#17413 = CYLINDRICAL_SURFACE ( 'NONE', #28387, 1.000000000000000000 ) ;
#17414 = ORIENTED_EDGE ( 'NONE', *, *, #22684, .T. ) ;
#17415 = CARTESIAN_POINT ( 'NONE',  ( -30.59866543348816847, -1.498850244747759852, -10.54007705693969399 ) ) ;
#17416 = AXIS2_PLACEMENT_3D ( 'NONE', #800, #16042, #34533 ) ;
#17417 = AXIS2_PLACEMENT_3D ( 'NONE', #17764, #30139, #36636 ) ;
#17418 = CARTESIAN_POINT ( 'NONE',  ( -23.61737546510163810, -7.194424252576709478, 20.99999999999999645 ) ) ;
#17419 = CARTESIAN_POINT ( 'NONE',  ( 24.96922983059882384, -9.289877593706156844, 20.99999999999995026 ) ) ;
#17420 = CYLINDRICAL_SURFACE ( 'NONE', #29100, 1.000000000000000000 ) ;
#17421 = EDGE_CURVE ( 'NONE', #27843, #3881, #8854, .T. ) ;
#17422 = VECTOR ( 'NONE', #6450, 1000.000000000000000 ) ;
#17423 = CARTESIAN_POINT ( 'NONE',  ( 4.096822963000107620, 8.035697679810645866, 7.000000000000000000 ) ) ;
#17425 = VECTOR ( 'NONE', #28830, 1000.000000000000000 ) ;
#17424 = CARTESIAN_POINT ( 'NONE',  ( 6.651296319737278750, 27.81603774131160023, 9.000000000000001776 ) ) ;
#17426 = ORIENTED_EDGE ( 'NONE', *, *, #6115, .F. ) ;
#17427 = CARTESIAN_POINT ( 'NONE',  ( 14.99905852611806267, 22.33194247983193392, 7.000000000000000000 ) ) ;
#17428 = CARTESIAN_POINT ( 'NONE',  ( 6.557822374958319323, 35.99981354310111215, 10.49999999999999822 ) ) ;
#17429 = CARTESIAN_POINT ( 'NONE',  ( -9.160254037844421049, 18.36602540378452630, 10.49999999999999822 ) ) ;
#17430 = CARTESIAN_POINT ( 'NONE',  ( 0.3823767728919280073, 35.39900042147797876, -11.06749343438611177 ) ) ;
#17431 = CYLINDRICAL_SURFACE ( 'NONE', #37951, 1.000000000000000888 ) ;
#17432 = DIRECTION ( 'NONE',  ( 0.5877852522924791323, 0.8090169943749430104, 0.000000000000000000 ) ) ;
#17433 = DIRECTION ( 'NONE',  ( 1.000000000000000000, 0.000000000000000000, 0.000000000000000000 ) ) ;
#17434 = DIRECTION ( 'NONE',  ( -1.000000000000000000, 0.000000000000000000, 0.000000000000000000 ) ) ;
#17435 = DIRECTION ( 'NONE',  ( 0.6459741880212536147, -0.2876062384759530688, -0.7071067811865442421 ) ) ;
#17436 = VECTOR ( 'NONE', #23740, 1000.000000000000114 ) ;
#17437 = CARTESIAN_POINT ( 'NONE',  ( 9.576129340711554860, 18.19128242950044694, -28.64815163939478637 ) ) ;
#17438 = DIRECTION ( 'NONE',  ( 0.000000000000000000, 0.000000000000000000, 1.000000000000000000 ) ) ;
#17439 = VECTOR ( 'NONE', #26834, 1000.000000000000114 ) ;
#17440 = VERTEX_POINT ( 'NONE', #20853 ) ;
#17442 = CARTESIAN_POINT ( 'NONE',  ( -14.81329996725647469, 19.93755115561707569, 10.50000000000000000 ) ) ;
#17441 = CARTESIAN_POINT ( 'NONE',  ( -19.02768546262373661, 16.45169234481391385, -8.391276880365140300 ) ) ;
#17443 = CARTESIAN_POINT ( 'NONE',  ( -0.9438746746332824511, 37.23829181892411810, 10.49999999999999822 ) ) ;
#17444 = CARTESIAN_POINT ( 'NONE',  ( 14.63889446902708791, -25.46407214954848897, -10.65228754373935516 ) ) ;
#17445 = LINE ( 'NONE', #29818, #970 ) ;
#17446 = CARTESIAN_POINT ( 'NONE',  ( 14.01698243316408465, 23.96616428142242583, -13.51035568235244888 ) ) ;
#17447 = AXIS2_PLACEMENT_3D ( 'NONE', #2617, #18064, #15206 ) ;
#17448 = CARTESIAN_POINT ( 'NONE',  ( 16.84920187454417828, 29.09530251867925443, -5.000000000000000000 ) ) ;
#17449 = DIRECTION ( 'NONE',  ( 0.000000000000000000, 0.000000000000000000, 1.000000000000000000 ) ) ;
#17450 = CIRCLE ( 'NONE', #26413, 1.000000000000000888 ) ;
#17451 = CARTESIAN_POINT ( 'NONE',  ( -24.43528513514284484, -21.68118427706984619, -12.95374139831338844 ) ) ;
#17452 = CARTESIAN_POINT ( 'NONE',  ( 4.888870946759487524, -21.71378906137520559, -20.01250066659168070 ) ) ;
#17453 = CARTESIAN_POINT ( 'NONE',  ( 15.12975596931773303, 25.61721673019504664, -9.242751917011917229 ) ) ;
#17454 = CARTESIAN_POINT ( 'NONE',  ( 20.13608159894178229, 13.64158595004140118, -10.38155476756366546 ) ) ;
#17455 = FACE_OUTER_BOUND ( 'NONE', #38430, .T. ) ;
#17456 = ORIENTED_EDGE ( 'NONE', *, *, #12269, .T. ) ;
#17457 = CARTESIAN_POINT ( 'NONE',  ( -4.687651652602798258, 27.18500950432644814, -17.67400160435538936 ) ) ;
#17458 = ORIENTED_EDGE ( 'NONE', *, *, #18958, .F. ) ;
#17459 = DIRECTION ( 'NONE',  ( -0.3090169943749573878, -0.9510565162951503115, 0.000000000000000000 ) ) ;
#17460 = ORIENTED_EDGE ( 'NONE', *, *, #13359, .T. ) ;
#17461 = CARTESIAN_POINT ( 'NONE',  ( 0.2474667741973399226, 28.36888560440311480, 6.000000000000000000 ) ) ;
#17462 = ADVANCED_FACE ( 'NONE', ( #11899 ), #24288, .T. ) ;
#17463 = CARTESIAN_POINT ( 'NONE',  ( -6.082607396026893376, 23.58034083595207875, 6.000000000000000000 ) ) ;
#17464 = ORIENTED_EDGE ( 'NONE', *, *, #22636, .T. ) ;
#17465 = CARTESIAN_POINT ( 'NONE',  ( -29.21513571016266653, 0.4812426229608742778, -10.19062845617733792 ) ) ;
#17466 = ORIENTED_EDGE ( 'NONE', *, *, #31958, .T. ) ;
#17467 = CARTESIAN_POINT ( 'NONE',  ( 35.42524632062607282, -11.88397916807875809, -5.867122752966118959 ) ) ;
#17468 = CIRCLE ( 'NONE', #11598, 1.000000000000000000 ) ;
#17469 = CIRCLE ( 'NONE', #37577, 1.000000000000002665 ) ;
#17470 = EDGE_CURVE ( 'NONE', #35629, #7370, #31443, .T. ) ;
#17471 = ORIENTED_EDGE ( 'NONE', *, *, #789, .T. ) ;
#17472 = CARTESIAN_POINT ( 'NONE',  ( -0.4999999999999998890, 37.26099332938164110, 10.94611345180490503 ) ) ;
#17473 = VERTEX_POINT ( 'NONE', #38928 ) ;
#17474 = EDGE_CURVE ( 'NONE', #28046, #18302, #8041, .T. ) ;
#17475 = AXIS2_PLACEMENT_3D ( 'NONE', #8160, #39239, #24400 ) ;
#17476 = DIRECTION ( 'NONE',  ( 0.000000000000000000, 0.000000000000000000, 1.000000000000000000 ) ) ;
#17477 = CARTESIAN_POINT ( 'NONE',  ( 18.69515074622676565, 22.45407711375075976, 10.99999999997785949 ) ) ;
#17478 = DIRECTION ( 'NONE',  ( 1.000000000000000000, 0.000000000000000000, 0.000000000000000000 ) ) ;
#17479 = ORIENTED_EDGE ( 'NONE', *, *, #10548, .F. ) ;
#17480 = CARTESIAN_POINT ( 'NONE',  ( -9.201548168576545450, 26.54122646004472585, 10.50000000000000533 ) ) ;
#17481 = DIRECTION ( 'NONE',  ( 1.000000000000000000, 3.469446951953587368E-15, 0.000000000000000000 ) ) ;
#17482 = FACE_OUTER_BOUND ( 'NONE', #9515, .T. ) ;
#17483 = CARTESIAN_POINT ( 'NONE',  ( 18.65259608150544324, 16.46909145568280763, -10.35352517064599809 ) ) ;
#17484 = CARTESIAN_POINT ( 'NONE',  ( 7.508979622877860471, 21.09273152055256162, -23.33378713927033843 ) ) ;
#17485 = EDGE_LOOP ( 'NONE', ( #27333, #26528, #33116, #3006 ) ) ;
#17486 = CYLINDRICAL_SURFACE ( 'NONE', #18375, 1.000000000000000888 ) ;
#17487 = CARTESIAN_POINT ( 'NONE',  ( -9.303655249773276736, 10.73386218874833631, 7.500000000000000888 ) ) ;
#17488 = ADVANCED_FACE ( 'NONE', ( #32848 ), #5000, .T. ) ;
#17489 = EDGE_CURVE ( 'NONE', #14625, #26936, #40059, .T. ) ;
#17490 = CARTESIAN_POINT ( 'NONE',  ( 12.85713553451835622, -22.56248978612570966, -16.42156014717959067 ) ) ;
#17491 = DIRECTION ( 'NONE',  ( 1.000000000000000000, 0.000000000000000000, 0.000000000000000000 ) ) ;
#17492 = B_SPLINE_CURVE_WITH_KNOTS ( 'NONE', 3,
 ( #23752, #33516, #36948, #30050 ),
 .UNSPECIFIED., .F., .F.,
 ( 4, 4 ),
 ( 0.9333335856709981115, 1.000000000000000000 ),
 .UNSPECIFIED. ) ;
#17493 = CARTESIAN_POINT ( 'NONE',  ( 18.07620401364302865, 24.68088026512193167, -13.58461195433497082 ) ) ;
#17495 = AXIS2_PLACEMENT_3D ( 'NONE', #36265, #36854, #17978 ) ;
#17494 = CARTESIAN_POINT ( 'NONE',  ( -11.67752460253681335, 18.91976605311634074, -22.73368238245046058 ) ) ;
#17496 = CARTESIAN_POINT ( 'NONE',  ( -31.02271782694906932, -24.34398845624585306, 13.92931973827809067 ) ) ;
#17497 = CARTESIAN_POINT ( 'NONE',  ( 13.68001087461786014, -26.27761246146546625, -5.946931794816848083 ) ) ;
#17498 = CARTESIAN_POINT ( 'NONE',  ( -13.28503138821885798, 15.53523575316151017, 7.000000000000000000 ) ) ;
#17499 = EDGE_LOOP ( 'NONE', ( #4990, #22601, #11847, #33122 ) ) ;
#17500 = EDGE_LOOP ( 'NONE', ( #16608, #36785, #38473, #24579 ) ) ;
#17501 = AXIS2_PLACEMENT_3D ( 'NONE', #35145, #29251, #7298 ) ;
#17502 = CARTESIAN_POINT ( 'NONE',  ( -11.09189806811868451, 30.64568619558879092, -11.25123976201009768 ) ) ;
#17503 = DIRECTION ( 'NONE',  ( 0.9945218953682730678, -0.1045284632676569680, 0.000000000000000000 ) ) ;
#17504 = DIRECTION ( 'NONE',  ( 1.000000000000000000, 0.000000000000000000, 0.000000000000000000 ) ) ;
#17505 = CARTESIAN_POINT ( 'NONE',  ( -25.24817616836305234, -4.671370533674584991, -18.94551454778549271 ) ) ;
#17506 = FACE_OUTER_BOUND ( 'NONE', #34242, .T. ) ;
#17507 = ORIENTED_EDGE ( 'NONE', *, *, #8812, .F. ) ;
#17508 = CARTESIAN_POINT ( 'NONE',  ( 21.70043827152030147, 0.7738983909411112361, -23.85944868390605933 ) ) ;
#17509 = CARTESIAN_POINT ( 'NONE',  ( -3.503793317224517700, 8.420815634768727520, 11.00000000000000000 ) ) ;
#17510 = CARTESIAN_POINT ( 'NONE',  ( -12.82065967939308493, 40.99677499958261961, 11.00000000000000000 ) ) ;
#17511 = CARTESIAN_POINT ( 'NONE',  ( 7.330070799514983193, 27.28854476845134513, 13.00000000000000178 ) ) ;
#17512 = VERTEX_POINT ( 'NONE', #8454 ) ;
#17513 = CARTESIAN_POINT ( 'NONE',  ( -30.78169477786137165, -0.02024540836640525976, -6.417008053751995789 ) ) ;
#17514 = EDGE_CURVE ( 'NONE', #22657, #34540, #5401, .T. ) ;
#17515 = DIRECTION ( 'NONE',  ( 1.000000000000000000, 0.000000000000000000, 0.000000000000000000 ) ) ;
#17516 = ORIENTED_EDGE ( 'NONE', *, *, #73, .F. ) ;
#17517 = CARTESIAN_POINT ( 'NONE',  ( 23.42190877138765970, -2.678843437355377333, -21.21129800221541473 ) ) ;
#17518 = CARTESIAN_POINT ( 'NONE',  ( 35.97875289183331660, -7.317948980263661696, 15.13084544680216759 ) ) ;
#17519 = ORIENTED_EDGE ( 'NONE', *, *, #19699, .F. ) ;
#17520 = CARTESIAN_POINT ( 'NONE',  ( -13.95035364761271346, 31.96289125330682168, 15.13084544680213561 ) ) ;
#17521 = CARTESIAN_POINT ( 'NONE',  ( -5.356921161177144342, -23.13411080437162326, 17.92354375535250810 ) ) ;
#17522 = CARTESIAN_POINT ( 'NONE',  ( -22.37798348102460722, 33.25980436007204588, 7.499999999999993783 ) ) ;
#17523 = CARTESIAN_POINT ( 'NONE',  ( -1.790359260782678597, 30.61752677313652882, 20.69868183039780973 ) ) ;
#17524 = AXIS2_PLACEMENT_3D ( 'NONE', #38806, #30066, #14629 ) ;
#17525 = CARTESIAN_POINT ( 'NONE',  ( 0.000000000000000000, 22.50000000000000355, 7.000000000000000000 ) ) ;
#17526 = ORIENTED_EDGE ( 'NONE', *, *, #1172, .F. ) ;
#17527 = CARTESIAN_POINT ( 'NONE',  ( -6.367390439426523052, 24.26983560722021238, 20.94377226548377635 ) ) ;
#17528 = LINE ( 'NONE', #20572, #38986 ) ;
#17529 = VECTOR ( 'NONE', #9719, 1000.000000000000000 ) ;
#17530 = CARTESIAN_POINT ( 'NONE',  ( 7.126104678631604905, 36.82515065381944197, -4.999999999999999112 ) ) ;
#17531 = DIRECTION ( 'NONE',  ( -0.9781476007338069101, -0.2079116908177532641, 0.000000000000000000 ) ) ;
#17532 = CARTESIAN_POINT ( 'NONE',  ( 11.82346474098068789, 13.60361205941433660, 20.69868183039785947 ) ) ;
#17533 = EDGE_CURVE ( 'NONE', #36946, #12832, #14749, .T. ) ;
#17534 = CARTESIAN_POINT ( 'NONE',  ( 12.70332137780860648, -16.96759668345817929, -25.93924617538274546 ) ) ;
#17535 = FACE_OUTER_BOUND ( 'NONE', #27228, .T. ) ;
#17536 = CARTESIAN_POINT ( 'NONE',  ( -13.10100158616367061, 15.51348347676449357, 10.87262190630137226 ) ) ;
#17537 = DIRECTION ( 'NONE',  ( 0.000000000000000000, 0.000000000000000000, 1.000000000000000000 ) ) ;
#17538 = ORIENTED_EDGE ( 'NONE', *, *, #37427, .F. ) ;
#17539 = CARTESIAN_POINT ( 'NONE',  ( 10.89778913317478626, 17.36343269013392643, -29.34648515220084164 ) ) ;
#17540 = ORIENTED_EDGE ( 'NONE', *, *, #1108, .T. ) ;
#17541 = CARTESIAN_POINT ( 'NONE',  ( -11.48506209758023466, 17.53631524467423120, -26.25656942401292682 ) ) ;
#17542 = CARTESIAN_POINT ( 'NONE',  ( -31.47522604700202109, -16.54376571344602809, 18.87996532025822205 ) ) ;
#17543 = CARTESIAN_POINT ( 'NONE',  ( -13.98881638187866550, 26.51951085733906410, 10.99999999999999289 ) ) ;
#17544 = CARTESIAN_POINT ( 'NONE',  ( 15.33365340323996051, 26.38076590146513922, -7.358350115893553145 ) ) ;
#17545 = ORIENTED_EDGE ( 'NONE', *, *, #31114, .F. ) ;
#17546 = CARTESIAN_POINT ( 'NONE',  ( 29.89701346908697488, -18.95835593754587123, -11.06832977680900498 ) ) ;
#17547 = EDGE_LOOP ( 'NONE', ( #10956, #26398, #6449 ) ) ;
#17549 = DIRECTION ( 'NONE',  ( 0.000000000000000000, 0.000000000000000000, 1.000000000000000000 ) ) ;
#17548 = CARTESIAN_POINT ( 'NONE',  ( -10.65603027360134902, 17.51308114404589844, -29.99999999999999289 ) ) ;
#17550 = CARTESIAN_POINT ( 'NONE',  ( -18.07817403047586780, -26.86642225889332281, -7.745473075693468878 ) ) ;
#17551 = B_SPLINE_CURVE_WITH_KNOTS ( 'NONE', 3,
 ( #15084, #24229, #8798, #5741, #30131, #18148, #18336, #2892, #37020, #17552, #29926 ),
 .UNSPECIFIED., .F., .F.,
 ( 4, 1, 1, 1, 1, 1, 1, 1, 4 ),
 ( 0.000000000000000000, 0.1249999999999998612, 0.2499999999999997224, 0.3749999999999995559, 0.5000000000000000000, 0.6250000000000004441, 0.7500000000000003331, 0.8750000000000001110, 1.000000000000000000 ),
 .UNSPECIFIED. ) ;
#17552 = CARTESIAN_POINT ( 'NONE',  ( 16.84920187454417828, 29.09530251867925443, -5.000000000000000000 ) ) ;
#17553 = EDGE_LOOP ( 'NONE', ( #3326, #33541, #28433, #31644 ) ) ;
#17554 = CARTESIAN_POINT ( 'NONE',  ( -19.53919056584213365, -7.419766065029655522, -27.01108906676794064 ) ) ;
#17555 = CARTESIAN_POINT ( 'NONE',  ( -11.80268877440303932, -22.03891725494794684, -17.47952885073186380 ) ) ;
#17556 = LINE ( 'NONE', #26883, #37174 ) ;
#17557 = ORIENTED_EDGE ( 'NONE', *, *, #30446, .F. ) ;
#17558 = CARTESIAN_POINT ( 'NONE',  ( 28.40256726208064819, 1.176742560656635961, -10.68423771036775349 ) ) ;
#17559 = CARTESIAN_POINT ( 'NONE',  ( 13.30736835487433289, 15.68301270189216545, 11.00000000000000000 ) ) ;
#17560 = DIRECTION ( 'NONE',  ( 1.000000000000000000, 0.000000000000000000, 0.000000000000000000 ) ) ;
#17561 = VECTOR ( 'NONE', #28739, 1000.000000000000000 ) ;
#17562 = ORIENTED_EDGE ( 'NONE', *, *, #4376, .F. ) ;
#17563 = CARTESIAN_POINT ( 'NONE',  ( -21.28582742437048125, 0.7081099580931202730, -25.00715929252305614 ) ) ;
#17564 = EDGE_CURVE ( 'NONE', #5349, #29941, #8651, .T. ) ;
#17565 = CARTESIAN_POINT ( 'NONE',  ( 26.94956399649580447, -0.4151258792086239269, -15.36823525240014021 ) ) ;
#17566 = EDGE_CURVE ( 'NONE', #15223, #4851, #31627, .T. ) ;
#17567 = CARTESIAN_POINT ( 'NONE',  ( 32.58967084635737166, -11.00843821516718180, 18.87996532025784191 ) ) ;
#17568 = ORIENTED_EDGE ( 'NONE', *, *, #370, .T. ) ;
#17569 = EDGE_CURVE ( 'NONE', #7663, #11410, #14105, .T. ) ;
#17570 = CARTESIAN_POINT ( 'NONE',  ( -26.58565005577111506, 1.039147901724387646, -14.52972379629277278 ) ) ;
#17571 = CARTESIAN_POINT ( 'NONE',  ( -33.62187204924172335, 0.04418559750806146796, -5.000000000000000000 ) ) ;
#17572 = DIRECTION ( 'NONE',  ( -1.000000000000000000, 0.000000000000000000, 0.000000000000000000 ) ) ;
#17573 = AXIS2_PLACEMENT_3D ( 'NONE', #10209, #22592, #1072 ) ;
#17574 = ADVANCED_FACE ( 'NONE', ( #34234 ), #31377, .T. ) ;
#17575 = CARTESIAN_POINT ( 'NONE',  ( -32.33143948541797386, 1.358872982501903248, 11.00000000000000000 ) ) ;
#17576 = AXIS2_PLACEMENT_3D ( 'NONE', #19652, #4418, #13757 ) ;
#17577 = CARTESIAN_POINT ( 'NONE',  ( -1.854038262753995303, 7.614540224935766766, 7.102637441331452806 ) ) ;
#17578 = CARTESIAN_POINT ( 'NONE',  ( -0.4999999999999998890, 37.00000000000000711, 7.500000000000000888 ) ) ;
#17579 = DIRECTION ( 'NONE',  ( 1.000000000000000000, 0.000000000000000000, 0.000000000000000000 ) ) ;
#17580 = VERTEX_POINT ( 'NONE', #12884 ) ;
#17581 = CARTESIAN_POINT ( 'NONE',  ( -24.65099977277350618, 5.218662007276516412, -12.76667628574117330 ) ) ;
#17582 = LINE ( 'NONE', #29954, #824 ) ;
#17583 = DIRECTION ( 'NONE',  ( 0.000000000000000000, 0.000000000000000000, 1.000000000000000000 ) ) ;
#17584 = CARTESIAN_POINT ( 'NONE',  ( 23.98745773934783188, -24.95113523879620487, -9.823517314964597347 ) ) ;
#17585 = ADVANCED_FACE ( 'NONE', ( #18793 ), #34247, .T. ) ;
#17586 = VECTOR ( 'NONE', #2627, 1000.000000000000000 ) ;
#17587 = EDGE_CURVE ( 'NONE', #10001, #25752, #35549, .T. ) ;
#17588 = DIRECTION ( 'NONE',  ( 1.000000000000000000, 0.000000000000000000, 0.000000000000000000 ) ) ;
#17589 = DIRECTION ( 'NONE',  ( 0.000000000000000000, 0.000000000000000000, 1.000000000000000000 ) ) ;
#17590 = EDGE_CURVE ( 'NONE', #27094, #6329, #18672, .T. ) ;
#17591 = CARTESIAN_POINT ( 'NONE',  ( 13.29767035538005970, 23.20272292486270516, -15.40656767438932384 ) ) ;
#17592 = CARTESIAN_POINT ( 'NONE',  ( 5.121747905603605489, -25.93120163663720845, 14.53008259254011136 ) ) ;
#17593 = VERTEX_POINT ( 'NONE', #37673 ) ;
#17594 = CARTESIAN_POINT ( 'NONE',  ( -15.42899087826043036, 19.21586207912160305, -15.69889121110926844 ) ) ;
#17595 = CARTESIAN_POINT ( 'NONE',  ( -23.31768133719846503, -16.68166585059926632, 20.94377226548377990 ) ) ;
#17596 = CARTESIAN_POINT ( 'NONE',  ( 2.587660364795204782, 9.681887955242936883, 12.00000000000000000 ) ) ;
#17597 = CARTESIAN_POINT ( 'NONE',  ( 12.41340058665741175, 20.46094404086849750, -19.50037637990314821 ) ) ;
#17598 = ORIENTED_EDGE ( 'NONE', *, *, #20812, .F. ) ;
#17599 = CARTESIAN_POINT ( 'NONE',  ( -14.57109471128386602, 21.97402451295043591, 10.49999999999999822 ) ) ;
#17600 = VERTEX_POINT ( 'NONE', #5989 ) ;
#17602 = DIRECTION ( 'NONE',  ( 1.000000000000000000, 0.000000000000000000, 0.000000000000000000 ) ) ;
#17601 = CARTESIAN_POINT ( 'NONE',  ( -11.82408859876377250, 19.45482954233215622, -21.60399388538399634 ) ) ;
#17603 = CARTESIAN_POINT ( 'NONE',  ( -12.29769356462352903, -22.02265038325488433, -17.43646041213484565 ) ) ;
#17604 = CARTESIAN_POINT ( 'NONE',  ( -29.88800841291100596, -25.99212743942916148, 12.14047268033113269 ) ) ;
#17605 = VECTOR ( 'NONE', #38847, 1000.000000000000000 ) ;
#17606 = CARTESIAN_POINT ( 'NONE',  ( -32.63711378803102292, -17.08632674381000172, -9.283697192344297022 ) ) ;
#17607 = CARTESIAN_POINT ( 'NONE',  ( -6.123308122133267695, -19.62006737319780569, -30.00000000000000711 ) ) ;
#17608 = DIRECTION ( 'NONE',  ( 1.000000000000000000, 0.000000000000000000, 0.000000000000000000 ) ) ;
#17609 = CARTESIAN_POINT ( 'NONE',  ( 12.54359778609175891, 18.68447145445714597, -21.72596103221125929 ) ) ;
#17610 = VERTEX_POINT ( 'NONE', #504 ) ;
#17611 = CARTESIAN_POINT ( 'NONE',  ( 22.44265844834124124, 7.045391211222152172, -15.86482432176597790 ) ) ;
#17612 = VECTOR ( 'NONE', #3704, 1000.000000000000000 ) ;
#17613 = CARTESIAN_POINT ( 'NONE',  ( -1.693998953219646664, 12.12549434688617644, 10.50000000000000000 ) ) ;
#17614 = CARTESIAN_POINT ( 'NONE',  ( -3.295881626406751419, 9.398963235502531433, 10.00000000000000000 ) ) ;
#17615 = CARTESIAN_POINT ( 'NONE',  ( -14.31603901957233660, 19.98981538725089990, 7.500000000000004441 ) ) ;
#17616 = ORIENTED_EDGE ( 'NONE', *, *, #7856, .T. ) ;
#17617 = CARTESIAN_POINT ( 'NONE',  ( -22.04621557984713220, -1.995498420971771436, -23.53374920157571637 ) ) ;
#17618 = EDGE_CURVE ( 'NONE', #14728, #24748, #9593, .T. ) ;
#17619 = CARTESIAN_POINT ( 'NONE',  ( 28.94423758251556222, 0.03876896675481636412, -11.59331513696461258 ) ) ;
#17620 = EDGE_CURVE ( 'NONE', #2436, #9639, #5039, .T. ) ;
#17621 = DIRECTION ( 'NONE',  ( 1.000000000000000000, 0.000000000000000000, 0.000000000000000000 ) ) ;
#17622 = ADVANCED_FACE ( 'NONE', ( #18397 ), #15737, .F. ) ;
#17623 = CARTESIAN_POINT ( 'NONE',  ( 19.27923728834097616, -17.06979480964821860, 20.99999999999999645 ) ) ;
#17624 = LINE ( 'NONE', #20255, #7670 ) ;
#17625 = VECTOR ( 'NONE', #3418, 1000.000000000000000 ) ;
#17626 = DIRECTION ( 'NONE',  ( -0.000000000000000000, -0.000000000000000000, -1.000000000000000000 ) ) ;
#17627 = EDGE_CURVE ( 'NONE', #4137, #24512, #11543, .T. ) ;
#17628 = ORIENTED_EDGE ( 'NONE', *, *, #468, .F. ) ;
#17629 = DIRECTION ( 'NONE',  ( 0.000000000000000000, 0.000000000000000000, 1.000000000000000000 ) ) ;
#17630 = AXIS2_PLACEMENT_3D ( 'NONE', #16875, #26400, #29254 ) ;
#17631 = DIRECTION ( 'NONE',  ( 0.000000000000000000, 0.000000000000000000, 1.000000000000000000 ) ) ;
#17632 = CARTESIAN_POINT ( 'NONE',  ( 75.15099915297797395, 43.38844959084117647, 0.000000000000000000 ) ) ;
#17633 = CARTESIAN_POINT ( 'NONE',  ( 0.2238614515109842162, 21.14277272035508659, -26.25630678787392824 ) ) ;
#17634 = CIRCLE ( 'NONE', #27353, 60.00000000000014211 ) ;
#17635 = CARTESIAN_POINT ( 'NONE',  ( -7.133890061153694617, 30.26901619224549833, 11.00000000000000000 ) ) ;
#17636 = CARTESIAN_POINT ( 'NONE',  ( 11.41267482483262619, 26.20820393249957192, 13.00000000000000178 ) ) ;
#17637 = FACE_OUTER_BOUND ( 'NONE', #14072, .T. ) ;
#17638 = DIRECTION ( 'NONE',  ( 1.000000000000000000, 0.000000000000000000, 0.000000000000000000 ) ) ;
#17639 = CARTESIAN_POINT ( 'NONE',  ( -0.5000000000000005551, 33.00000000000000000, 10.50000000000000000 ) ) ;
#17640 = FACE_OUTER_BOUND ( 'NONE', #12473, .T. ) ;
#17641 = EDGE_CURVE ( 'NONE', #34341, #31582, #3543, .T. ) ;
#17642 = CARTESIAN_POINT ( 'NONE',  ( 14.77883339423700448, 28.03561339302072497, -7.318319975446966552 ) ) ;
#17643 = DIRECTION ( 'NONE',  ( 0.000000000000000000, 0.000000000000000000, 1.000000000000000000 ) ) ;
#17644 = ORIENTED_EDGE ( 'NONE', *, *, #17772, .T. ) ;
#17646 = CARTESIAN_POINT ( 'NONE',  ( 9.441034666242805073, 32.57396620494213124, 7.000000000000000000 ) ) ;
#17645 = CARTESIAN_POINT ( 'NONE',  ( -18.07518878564494713, 14.05505073002865579, -16.95006174505777707 ) ) ;
#17647 = CARTESIAN_POINT ( 'NONE',  ( -13.90768907780708474, 27.88359266870287456, 10.49999999999999822 ) ) ;
#17648 = CIRCLE ( 'NONE', #9184, 1.000000000000000888 ) ;
#17649 = CARTESIAN_POINT ( 'NONE',  ( 13.39743745724321045, -23.62495958482203307, -14.47428836996529000 ) ) ;
#17650 = CARTESIAN_POINT ( 'NONE',  ( -14.11133924723978161, 27.61078317377194224, 10.49999999999999822 ) ) ;
#17651 = CARTESIAN_POINT ( 'NONE',  ( 13.47602490618416304, 22.84703953731449744, -15.44714390386671710 ) ) ;
#17652 = CARTESIAN_POINT ( 'NONE',  ( -20.66458278928016057, 17.76169105511799273, -5.000000000000000888 ) ) ;
#17653 = CARTESIAN_POINT ( 'NONE',  ( 35.72300735678889794, -23.12593625888495552, 11.00000000000000178 ) ) ;
#17654 = CARTESIAN_POINT ( 'NONE',  ( -27.48658736596179963, -21.56671790654684884, -11.09299434450578659 ) ) ;
#17655 = CARTESIAN_POINT ( 'NONE',  ( 1.801982192410312766, -24.64865591106047660, -7.429003440711998252 ) ) ;
#17656 = CARTESIAN_POINT ( 'NONE',  ( 13.10586528640805604, 21.36746738750283114, -17.46679796181676281 ) ) ;
#17657 = CARTESIAN_POINT ( 'NONE',  ( 17.51797765111094307, 10.67563444151121033, -29.99999999999999645 ) ) ;
#17658 = FACE_OUTER_BOUND ( 'NONE', #9971, .T. ) ;
#17659 = VERTEX_POINT ( 'NONE', #21632 ) ;
#17660 = CARTESIAN_POINT ( 'NONE',  ( -4.727343333413158710, 20.18853994959099651, -27.77675044586279895 ) ) ;
#17661 = ORIENTED_EDGE ( 'NONE', *, *, #17240, .T. ) ;
#17662 = CIRCLE ( 'NONE', #35153, 19.99999999999993605 ) ;
#17663 = CARTESIAN_POINT ( 'NONE',  ( -3.992867117591420545, 8.524771480177605554, 10.50000000000000533 ) ) ;
#17664 = ORIENTED_EDGE ( 'NONE', *, *, #12103, .T. ) ;
#17665 = EDGE_CURVE ( 'NONE', #25752, #34344, #6193, .T. ) ;
#17666 = PLANE ( 'NONE',  #14092 ) ;
#17667 = CARTESIAN_POINT ( 'NONE',  ( 11.14716901145161643, 12.46304090461738667, 12.00000000000000000 ) ) ;
#17668 = VERTEX_POINT ( 'NONE', #105 ) ;
#17669 = CARTESIAN_POINT ( 'NONE',  ( -20.52066404987779791, 0.9821139164781407249, -28.71129986131551703 ) ) ;
#17670 = ORIENTED_EDGE ( 'NONE', *, *, #31486, .T. ) ;
#17671 = CARTESIAN_POINT ( 'NONE',  ( 27.05781474705212375, -9.043496247948464628, -16.72532308214699270 ) ) ;
#17672 = ORIENTED_EDGE ( 'NONE', *, *, #31617, .F. ) ;
#17673 = AXIS2_PLACEMENT_3D ( 'NONE', #14191, #33098, #16854 ) ;
#17674 = CARTESIAN_POINT ( 'NONE',  ( 8.339609403135803234, 11.87216320208440123, 10.50000000000000000 ) ) ;
#17675 = VERTEX_POINT ( 'NONE', #24881 ) ;
#17676 = CYLINDRICAL_SURFACE ( 'NONE', #35934, 6.000000000000002665 ) ;
#17677 = CARTESIAN_POINT ( 'NONE',  ( 6.354454053420413473, 35.54304081427980577, 11.00000000000000000 ) ) ;
#17678 = CIRCLE ( 'NONE', #8579, 0.5000000000000015543 ) ;
#17679 = LINE ( 'NONE', #23957, #16206 ) ;
#17680 = ORIENTED_EDGE ( 'NONE', *, *, #1376, .F. ) ;
#17681 =( NAMED_UNIT ( * ) PLANE_ANGLE_UNIT ( ) SI_UNIT ( $, .RADIAN. ) );
#17682 = DIRECTION ( 'NONE',  ( 1.000000000000000000, 0.000000000000000000, 0.000000000000000000 ) ) ;
#17683 = CARTESIAN_POINT ( 'NONE',  ( -2.568190708544567435, 12.82247983807085490, 10.50000000000001066 ) ) ;
#17684 = CARTESIAN_POINT ( 'NONE',  ( -4.671003766000858981, 24.36559561389090689, 23.00000000000000000 ) ) ;
#17685 = CARTESIAN_POINT ( 'NONE',  ( 15.29022352314591870, 13.67480013622697044, -30.00000000000001066 ) ) ;
#17686 = CARTESIAN_POINT ( 'NONE',  ( 7.754350537738645244, 21.81137704913313868, -22.19334008859113538 ) ) ;
#17687 = ORIENTED_EDGE ( 'NONE', *, *, #32474, .F. ) ;
#17688 = CARTESIAN_POINT ( 'NONE',  ( -22.36636065667467221, 10.81625050891080164, -5.966924272146592045 ) ) ;
#17689 = CYLINDRICAL_SURFACE ( 'NONE', #2802, 0.4999999999999995559 ) ;
#17690 = AXIS2_PLACEMENT_3D ( 'NONE', #22197, #31351, #34799 ) ;
#17691 = CARTESIAN_POINT ( 'NONE',  ( -2.143544478356564031, 7.864861742947466539, 10.49999999999999822 ) ) ;
#17692 = EDGE_CURVE ( 'NONE', #18996, #34177, #27104, .T. ) ;
#17693 = CARTESIAN_POINT ( 'NONE',  ( 10.12794487532474719, -18.74775046445166993, -24.99559475216551263 ) ) ;
#17694 = DIRECTION ( 'NONE',  ( 0.000000000000000000, 0.000000000000000000, 1.000000000000000000 ) ) ;
#17695 = CARTESIAN_POINT ( 'NONE',  ( 18.07620401364302865, 24.68088026512193522, -5.000000000000000000 ) ) ;
#17696 = CARTESIAN_POINT ( 'NONE',  ( -14.52552742914873640, 24.99026629062174365, -11.59761377287194151 ) ) ;
#17697 = CARTESIAN_POINT ( 'NONE',  ( 13.56094288467416753, -26.09349823019973869, -7.365016121655886039 ) ) ;
#17698 = AXIS2_PLACEMENT_3D ( 'NONE', #2350, #35871, #36278 ) ;
#17699 = DIRECTION ( 'NONE',  ( -0.4731467892558186561, 0.5254827454987605062, -0.7071067811865437980 ) ) ;
#17700 = ADVANCED_FACE ( 'NONE', ( #9843 ), #37490, .T. ) ;
#17701 = ORIENTED_EDGE ( 'NONE', *, *, #2542, .F. ) ;
#17702 = ORIENTED_EDGE ( 'NONE', *, *, #5399, .T. ) ;
#17703 = CARTESIAN_POINT ( 'NONE',  ( -8.754768201593860155, 24.05476072843883983, -18.96584428646194098 ) ) ;
#17704 = DIRECTION ( 'NONE',  ( 0.000000000000000000, -0.000000000000000000, 1.000000000000000000 ) ) ;
#17705 = CARTESIAN_POINT ( 'NONE',  ( -12.41469063302772113, 14.32475803611781728, 10.49999999999999822 ) ) ;
#17706 = CIRCLE ( 'NONE', #8615, 1.000000000000000000 ) ;
#17707 = CARTESIAN_POINT ( 'NONE',  ( -10.16122020288868733, 33.53402030034415304, 7.000000000000000000 ) ) ;
#17708 = ORIENTED_EDGE ( 'NONE', *, *, #33705, .T. ) ;
#17709 = CARTESIAN_POINT ( 'NONE',  ( 30.42199879797928119, 0.05422021819292949935, -7.828243430681267157 ) ) ;
#17710 = CARTESIAN_POINT ( 'NONE',  ( 6.980762143445867984, 14.59310681135549537, 10.49999999999999645 ) ) ;
#17711 = DIRECTION ( 'NONE',  ( 1.000000000000000000, 0.000000000000000000, 0.000000000000000000 ) ) ;
#17712 = B_SPLINE_CURVE_WITH_KNOTS ( 'NONE', 3,
 ( #6872, #36624, #8796, #21183, #30535, #12035 ),
 .UNSPECIFIED., .F., .F.,
 ( 4, 2, 4 ),
 ( 0.000000000000000000, 0.5000000000000000000, 1.000000000000000000 ),
 .UNSPECIFIED. ) ;
#17713 = ORIENTED_EDGE ( 'NONE', *, *, #29605, .T. ) ;
#17714 = CARTESIAN_POINT ( 'NONE',  ( -26.49304050658699339, 0.2940916338183011125, -15.45185423700121774 ) ) ;
#17715 = DIRECTION ( 'NONE',  ( -0.7886751345948098679, -0.2113248654051767539, 0.5773502691896337247 ) ) ;
#17716 = ORIENTED_EDGE ( 'NONE', *, *, #17331, .F. ) ;
#17717 = CARTESIAN_POINT ( 'NONE',  ( 20.99914968644306867, -2.977695377099063290, -25.90524470544396962 ) ) ;
#17718 = CARTESIAN_POINT ( 'NONE',  ( 32.86149060640417474, -21.03113892363574422, 15.72805884748937721 ) ) ;
#17719 = VERTEX_POINT ( 'NONE', #37477 ) ;
#17720 = CARTESIAN_POINT ( 'NONE',  ( -5.571153519069262039, 39.03845596069744062, 13.92931973827808534 ) ) ;
#17721 = ADVANCED_FACE ( 'NONE', ( #6581 ), #22220, .T. ) ;
#17722 = CARTESIAN_POINT ( 'NONE',  ( 11.87696897078051350, -16.96707895818725831, 20.82122704794063495 ) ) ;
#17723 = CARTESIAN_POINT ( 'NONE',  ( 13.87104230352200140, 20.53934056656866147, 9.500000000000000000 ) ) ;
#17724 = CARTESIAN_POINT ( 'NONE',  ( 5.506351411278700425, 29.74560631396668597, 20.50957957746029692 ) ) ;
#17725 = TOROIDAL_SURFACE ( 'NONE', #190, 1.000000000000000000, 0.5000000000000000000 ) ;
#17726 = CARTESIAN_POINT ( 'NONE',  ( 32.33143948541787438, 1.358872982501792226, 23.00000000000000000 ) ) ;
#17727 = ORIENTED_EDGE ( 'NONE', *, *, #15015, .T. ) ;
#17728 = CARTESIAN_POINT ( 'NONE',  ( 11.77090408390491305, 15.39748370681878775, 12.00000000000000000 ) ) ;
#17729 = CIRCLE ( 'NONE', #28744, 1.000000000000000000 ) ;
#17730 = FACE_OUTER_BOUND ( 'NONE', #8728, .T. ) ;
#17731 = CARTESIAN_POINT ( 'NONE',  ( 4.643464871730170529, 23.98615981536725883, -20.80716177970646541 ) ) ;
#17732 = AXIS2_PLACEMENT_3D ( 'NONE', #14724, #32822, #20628 ) ;
#17733 = CARTESIAN_POINT ( 'NONE',  ( -12.11431921870781281, -16.53859995802357474, -30.00000000000001066 ) ) ;
#17734 = CARTESIAN_POINT ( 'NONE',  ( 17.01074486384225892, 2.963432112715942868, 20.82122704794076995 ) ) ;
#17735 = EDGE_CURVE ( 'NONE', #8022, #25824, #7646, .T. ) ;
#17736 = CARTESIAN_POINT ( 'NONE',  ( 19.77033395158426288, -27.21289834263597740, -5.910049683774938778 ) ) ;
#17737 = DIRECTION ( 'NONE',  ( -1.000000000000000000, 0.000000000000000000, 0.000000000000000000 ) ) ;
#17738 = CARTESIAN_POINT ( 'NONE',  ( 23.80624316739448787, 27.22568555153026537, 7.500000000000000000 ) ) ;
#17739 = PLANE ( 'NONE',  #16167 ) ;
#17740 = EDGE_LOOP ( 'NONE', ( #34095, #16547, #8920, #29485 ) ) ;
#17741 = VECTOR ( 'NONE', #25898, 1000.000000000000114 ) ;
#17742 = CARTESIAN_POINT ( 'NONE',  ( 13.42936096295450099, 22.94210890876663456, -15.43620599078790434 ) ) ;
#17743 = VERTEX_POINT ( 'NONE', #28524 ) ;
#17744 = CARTESIAN_POINT ( 'NONE',  ( -12.53790509067911074, 19.44194302981471623, -20.61120958872907138 ) ) ;
#17745 = CARTESIAN_POINT ( 'NONE',  ( -33.29356883319611171, -10.99541271083418614, 18.42518152272184295 ) ) ;
#17746 = ADVANCED_FACE ( 'NONE', ( #13484 ), #16109, .T. ) ;
#17747 = CARTESIAN_POINT ( 'NONE',  ( 3.859984908523940828, 8.004988684046397296, 7.455686640544892718 ) ) ;
#17748 = CARTESIAN_POINT ( 'NONE',  ( 11.12672621128664296, 17.36766021414478089, -28.08254997068604553 ) ) ;
#17749 = EDGE_CURVE ( 'NONE', #6055, #19050, #35224, .T. ) ;
#17750 = ORIENTED_EDGE ( 'NONE', *, *, #10443, .F. ) ;
#17751 = CARTESIAN_POINT ( 'NONE',  ( 32.51966212229606867, -20.60195123665384287, -4.999999999999998224 ) ) ;
#17752 = ORIENTED_EDGE ( 'NONE', *, *, #23913, .T. ) ;
#17753 = CARTESIAN_POINT ( 'NONE',  ( -11.39209870729926166, 19.18961260050172513, -22.68434712264469155 ) ) ;
#17754 = VECTOR ( 'NONE', #8417, 1000.000000000000000 ) ;
#17755 = CARTESIAN_POINT ( 'NONE',  ( -10.28721823975710059, -17.89894537374451744, -28.03678530533794344 ) ) ;
#17756 = LINE ( 'NONE', #26878, #39925 ) ;
#17757 = COLOUR_RGB ( '', 0.09019608, 0.27058824, 0.51372549) ;
#17758 = ORIENTED_EDGE ( 'NONE', *, *, #11180, .F. ) ;
#17759 = CARTESIAN_POINT ( 'NONE',  ( -30.05994772858080921, -10.30773001763154539, -13.86984580451319538 ) ) ;
#17760 = CARTESIAN_POINT ( 'NONE',  ( -15.22509278422137768, -26.60142203870535127, -6.417211518553083138 ) ) ;
#17761 = CARTESIAN_POINT ( 'NONE',  ( -14.36830325120615903, 20.48707633493503621, 7.000000000000000000 ) ) ;
#17762 = ORIENTED_EDGE ( 'NONE', *, *, #23922, .F. ) ;
#17763 = CARTESIAN_POINT ( 'NONE',  ( 27.48662654444790476, 1.221943985062914795, -12.60017615557705462 ) ) ;
#17764 = CARTESIAN_POINT ( 'NONE',  ( 1.590043107810628298, 12.61456814725305442, 10.49999999999999467 ) ) ;
#17765 = CARTESIAN_POINT ( 'NONE',  ( -16.58691282011878698, -31.15705289669003264, 22.99999999999999289 ) ) ;
#17766 = ORIENTED_EDGE ( 'NONE', *, *, #27780, .T. ) ;
#17767 = CARTESIAN_POINT ( 'NONE',  ( -22.75659833837781676, 0.5252670190201254030, -21.60573177101157327 ) ) ;
#17768 = ORIENTED_EDGE ( 'NONE', *, *, #7689, .F. ) ;
#17769 = CARTESIAN_POINT ( 'NONE',  ( 21.02639339174489308, 0.1643985004216583778, -26.16791350077025058 ) ) ;
#17770 = CIRCLE ( 'NONE', #24205, 18.00000000000003553 ) ;
#17771 = CARTESIAN_POINT ( 'NONE',  ( 30.76885290917950044, -8.559665202947678964, 19.66345542862528006 ) ) ;
#17772 = EDGE_CURVE ( 'NONE', #2261, #26597, #36847, .T. ) ;
#17773 = ORIENTED_EDGE ( 'NONE', *, *, #4565, .F. ) ;
#17774 = CARTESIAN_POINT ( 'NONE',  ( -26.91927498037264499, 4.412534205184938330, -5.000000000000001776 ) ) ;
#17775 = ADVANCED_FACE ( 'NONE', ( #4549 ), #35033, .F. ) ;
#17776 = CARTESIAN_POINT ( 'NONE',  ( -10.52298572764586915, 33.18979484031245875, 7.381627713044575323 ) ) ;
#17777 = CARTESIAN_POINT ( 'NONE',  ( 14.79657804239838192, 20.03703012860012223, 7.381627713044574435 ) ) ;
#17778 = AXIS2_PLACEMENT_3D ( 'NONE', #7607, #26905, #14311 ) ;
#17779 = DIRECTION ( 'NONE',  ( 0.000000000000000000, 0.000000000000000000, 1.000000000000000000 ) ) ;
#17780 = FACE_OUTER_BOUND ( 'NONE', #11842, .T. ) ;
#17781 = VECTOR ( 'NONE', #34701, 1000.000000000000000 ) ;
#17782 = DIRECTION ( 'NONE',  ( 0.000000000000000000, 0.000000000000000000, 1.000000000000000000 ) ) ;
#17783 = CARTESIAN_POINT ( 'NONE',  ( 13.49038105676655164, 15.86602540378438064, 10.50000000000000000 ) ) ;
#17784 = VERTEX_POINT ( 'NONE', #19996 ) ;
#17785 = CARTESIAN_POINT ( 'NONE',  ( -23.75513742221500024, 6.044705833718418297, -13.79811425570447980 ) ) ;
#17786 = DIRECTION ( 'NONE',  ( 1.000000000000000000, 0.000000000000000000, 0.000000000000000000 ) ) ;
#17787 = DIRECTION ( 'NONE',  ( 0.000000000000000000, 0.000000000000000000, 1.000000000000000000 ) ) ;
#17788 = CARTESIAN_POINT ( 'NONE',  ( 15.71069447272513742, -14.48203284589343376, -25.69054009000548788 ) ) ;
#17789 = CARTESIAN_POINT ( 'NONE',  ( 9.593266739736579396, 18.11602540378440196, 10.50000000000000178 ) ) ;
#17790 = DIRECTION ( 'NONE',  ( 0.000000000000000000, 0.000000000000000000, 1.000000000000000000 ) ) ;
#17791 = EDGE_CURVE ( 'NONE', #36670, #19499, #16951, .T. ) ;
#17792 = CARTESIAN_POINT ( 'NONE',  ( 15.18466250546081220, 27.13099485538614175, -6.876955971306166759 ) ) ;
#17793 = CARTESIAN_POINT ( 'NONE',  ( 15.37000524125214440, -27.20210912714641793, 15.72805884748939498 ) ) ;
#17794 = ORIENTED_EDGE ( 'NONE', *, *, #5690, .T. ) ;
#17795 = AXIS2_PLACEMENT_3D ( 'NONE', #38387, #22943, #7502 ) ;
#17796 = CARTESIAN_POINT ( 'NONE',  ( -13.48553142464132115, 15.75358007923588843, -27.02007185819866208 ) ) ;
#17797 = CARTESIAN_POINT ( 'NONE',  ( -25.96434769773127726, -12.55439225991604779, 20.94377226548378346 ) ) ;
#17798 = DIRECTION ( 'NONE',  ( 0.000000000000000000, 0.000000000000000000, -1.000000000000000000 ) ) ;
#17799 = CARTESIAN_POINT ( 'NONE',  ( 13.77977818563562096, 23.37426034515904760, -14.47731727276712554 ) ) ;
#17800 = EDGE_LOOP ( 'NONE', ( #5141, #6057, #13785, #16294 ) ) ;
#17801 = CARTESIAN_POINT ( 'NONE',  ( 11.18323034263230120, 17.75715498309746820, -26.22476241273412256 ) ) ;
#17802 = ORIENTED_EDGE ( 'NONE', *, *, #21542, .F. ) ;
#17804 = CARTESIAN_POINT ( 'NONE',  ( 5.082600654608392610, 21.41965916404854298, 6.000000000000000000 ) ) ;
#17803 = CARTESIAN_POINT ( 'NONE',  ( -15.32605299005571808, 26.83348367465769968, -6.414615797237237516 ) ) ;
#17805 = CARTESIAN_POINT ( 'NONE',  ( -12.34719756161035242, -22.02191913002371848, -17.43064001291457288 ) ) ;
#17806 = LINE ( 'NONE', #39716, #32127 ) ;
#17807 = CARTESIAN_POINT ( 'NONE',  ( -17.55945971783640758, -10.59693620792911872, -29.21186350523559483 ) ) ;
#17808 = CIRCLE ( 'NONE', #18456, 0.5000000000000004441 ) ;
#17809 = CARTESIAN_POINT ( 'NONE',  ( -7.003108942385479097, -21.17426981051016810, -20.95153987240063742 ) ) ;
#17810 = DIRECTION ( 'NONE',  ( -0.7431448254773862505, 0.6691306063588671194, 0.000000000000000000 ) ) ;
#17811 = CARTESIAN_POINT ( 'NONE',  ( 12.01362727457946278, 17.13078155611268727, -26.30899361330535058 ) ) ;
#17812 = ORIENTED_EDGE ( 'NONE', *, *, #28935, .F. ) ;
#17813 = CARTESIAN_POINT ( 'NONE',  ( 25.09257354179462496, 6.456226081335884714, -7.888698583467808056 ) ) ;
#17814 = CARTESIAN_POINT ( 'NONE',  ( 12.37435565298211237, 15.93301270189216545, 7.499999999999997335 ) ) ;
#17815 = CARTESIAN_POINT ( 'NONE',  ( -9.221287281574667816, 10.65863771052209863, 11.00000000000000000 ) ) ;
#17816 = CARTESIAN_POINT ( 'NONE',  ( -13.22516817658055288, 40.70288237343638826, 7.000000000000000000 ) ) ;
#17817 = EDGE_LOOP ( 'NONE', ( #3003, #34780 ) ) ;
#17818 = CARTESIAN_POINT ( 'NONE',  ( -23.76582790367996267, -0.8399181250771553531, -20.35841962654769688 ) ) ;
#17819 = CIRCLE ( 'NONE', #3514, 0.5000000000000000000 ) ;
#17820 = CARTESIAN_POINT ( 'NONE',  ( 20.61369574458117171, 0.7924611088881369225, -28.07461411969941878 ) ) ;
#17821 = DIRECTION ( 'NONE',  ( 0.000000000000000000, 0.000000000000000000, 1.000000000000000000 ) ) ;
#17822 = CARTESIAN_POINT ( 'NONE',  ( 24.18603102892799583, -14.68777056910919576, 20.99999999999999645 ) ) ;
#17823 = CARTESIAN_POINT ( 'NONE',  ( 27.08779848459123585, 7.221796966026763798, -5.000000000000007105 ) ) ;
#17824 = EDGE_CURVE ( 'NONE', #39968, #28710, #19327, .T. ) ;
#17825 = CARTESIAN_POINT ( 'NONE',  ( 36.04785107591604287, -18.56329043283700031, 11.00000000000005862 ) ) ;
#17826 = VERTEX_POINT ( 'NONE', #1505 ) ;
#17827 = CARTESIAN_POINT ( 'NONE',  ( 10.47804177580207607, 33.28010392086025604, 7.000000000000000000 ) ) ;
#17828 = CARTESIAN_POINT ( 'NONE',  ( -13.77067693704740492, 28.44713853003868564, 7.000000000000000000 ) ) ;
#17829 = VERTEX_POINT ( 'NONE', #38678 ) ;
#17830 = CARTESIAN_POINT ( 'NONE',  ( 1.341253818658974861, 32.42268633335680050, -13.80665395263008399 ) ) ;
#17831 = CARTESIAN_POINT ( 'NONE',  ( 8.183240348400453001, 28.21559575157615996, 12.00000000000000000 ) ) ;
#17832 = CARTESIAN_POINT ( 'NONE',  ( 16.24129362380266883, 27.01431713449538918, 15.13084544680213206 ) ) ;
#17833 = CARTESIAN_POINT ( 'NONE',  ( 3.813962023474617435, 32.29559562678520024, 10.00000000000000000 ) ) ;
#17834 = LINE ( 'NONE', #32869, #27721 ) ;
#17835 = CARTESIAN_POINT ( 'NONE',  ( 3.863783140547853712E-14, -86.77689918168233874, -5.000000000000000000 ) ) ;
#17836 = EDGE_CURVE ( 'NONE', #1261, #12491, #26500, .T. ) ;
#17837 = CARTESIAN_POINT ( 'NONE',  ( 4.881458130668207218, -28.77689918168226413, 22.99999999999999645 ) ) ;
#17838 = AXIS2_PLACEMENT_3D ( 'NONE', #11780, #2836, #12177 ) ;
#17839 = CARTESIAN_POINT ( 'NONE',  ( 10.41341893350470293, 19.30400416985194667, -23.68959501837800019 ) ) ;
#17840 = CARTESIAN_POINT ( 'NONE',  ( -9.343266739736650450, 17.68301270189230578, 10.50000000000000000 ) ) ;
#17841 = VERTEX_POINT ( 'NONE', #26283 ) ;
#17843 = CARTESIAN_POINT ( 'NONE',  ( -5.034171952701849584, 35.03623199971308111, 10.50000000000000000 ) ) ;
#17842 = CARTESIAN_POINT ( 'NONE',  ( -17.18163521729151455, 14.39254400151518176, -19.00291312292943857 ) ) ;
#17844 = DIRECTION ( 'NONE',  ( 0.7431448254773961315, 0.6691306063588561281, 0.000000000000000000 ) ) ;
#17845 = EDGE_CURVE ( 'NONE', #13470, #2072, #31029, .T. ) ;
#17846 = CARTESIAN_POINT ( 'NONE',  ( 10.26099256397509407, -19.15184415471343016, -23.84939042261497377 ) ) ;
#17847 = DIRECTION ( 'NONE',  ( -0.000000000000000000, -0.000000000000000000, -1.000000000000000000 ) ) ;
#17848 = CARTESIAN_POINT ( 'NONE',  ( 15.00904765070272973, 25.99870026096500908, -9.236802632963790671 ) ) ;
#17849 = AXIS2_PLACEMENT_3D ( 'NONE', #31802, #530, #22449 ) ;
#17850 = CARTESIAN_POINT ( 'NONE',  ( 1.100969307443724343, 12.51061230184417816, 10.49999999999999467 ) ) ;
#17851 = FACE_OUTER_BOUND ( 'NONE', #12241, .T. ) ;
#17852 = EDGE_CURVE ( 'NONE', #13902, #26362, #35431, .T. ) ;
#17853 = CARTESIAN_POINT ( 'NONE',  ( -18.63416092258458434, -14.56412937407352715, -21.89936666682847743 ) ) ;
#17854 = CARTESIAN_POINT ( 'NONE',  ( 4.218053344389335990, -20.12689330800646204, -28.26382229294831561 ) ) ;
#17855 = CARTESIAN_POINT ( 'NONE',  ( 11.18139086956414729, 17.23420873180600665, -28.71418858328174295 ) ) ;
#17856 = CARTESIAN_POINT ( 'NONE',  ( 17.78547439015788001, 10.85037366618364274, -25.51180193807143581 ) ) ;
#17857 = LINE ( 'NONE', #30443, #3718 ) ;
#17858 = CARTESIAN_POINT ( 'NONE',  ( -4.188474181932830831, 20.68942421501040840, -26.33881144299988009 ) ) ;
#17859 = VERTEX_POINT ( 'NONE', #29334 ) ;
#17860 = CARTESIAN_POINT ( 'NONE',  ( -32.09165771328039085, 1.123514972298483627, 13.32518128616608699 ) ) ;
#17861 = EDGE_LOOP ( 'NONE', ( #23275, #22200, #33137, #22018 ) ) ;
#17862 = DIRECTION ( 'NONE',  ( -0.1470157664651945972, 0.6916548014802286204, -0.7071067811865454633 ) ) ;
#17863 = CARTESIAN_POINT ( 'NONE',  ( -8.412270287199728358, 10.07085245822961994, 10.63089969389956835 ) ) ;
#17864 = CARTESIAN_POINT ( 'NONE',  ( -21.25244676704415525, 0.9439152883838316521, -25.03239665970995631 ) ) ;
#17865 = EDGE_CURVE ( 'NONE', #15951, #5508, #8123, .T. ) ;
#17866 = CARTESIAN_POINT ( 'NONE',  ( 19.63120307387857011, -5.935663759831210307, -29.99999999999999289 ) ) ;
#17867 = EDGE_CURVE ( 'NONE', #6755, #37897, #8983, .T. ) ;
#17868 = AXIS2_PLACEMENT_3D ( 'NONE', #8542, #10999, #23383 ) ;
#17869 = ORIENTED_EDGE ( 'NONE', *, *, #32442, .T. ) ;
#17870 = DIRECTION ( 'NONE',  ( 0.5254827454987551771, -0.4731467892558188226, -0.7071067811865476838 ) ) ;
#17871 = ORIENTED_EDGE ( 'NONE', *, *, #37588, .T. ) ;
#17872 = CARTESIAN_POINT ( 'NONE',  ( -3.724378136954612284, 12.76962061027129458, 6.000000000000000000 ) ) ;
#17873 = LINE ( 'NONE', #23554, #35802 ) ;
#17874 = AXIS2_PLACEMENT_3D ( 'NONE', #13756, #5021, #35708 ) ;
#17875 = AXIS2_PLACEMENT_3D ( 'NONE', #28918, #8190, #16942 ) ;
#17876 = CARTESIAN_POINT ( 'NONE',  ( -3.607749162633401507, 7.931741834401821123, 10.49999999999999822 ) ) ;
#17877 = ORIENTED_EDGE ( 'NONE', *, *, #34223, .T. ) ;
#17878 = DIRECTION ( 'NONE',  ( -0.1045284632676569680, -0.9945218953682729568, 0.000000000000000000 ) ) ;
#17879 = DIRECTION ( 'NONE',  ( 0.8090169943749505599, 0.5877852522924689183, 0.000000000000000000 ) ) ;
#17880 = DIRECTION ( 'NONE',  ( 0.9945218953682731788, -0.1045284632676563297, 0.000000000000000000 ) ) ;
#17881 = CARTESIAN_POINT ( 'NONE',  ( 21.38147419243281178, -17.48660460948667250, -17.66603181204244066 ) ) ;
#17882 = EDGE_CURVE ( 'NONE', #3976, #29462, #15449, .T. ) ;
#17883 = CARTESIAN_POINT ( 'NONE',  ( 15.91426628502474294, 13.28120225394148157, -26.57843054152041518 ) ) ;
#17884 = CARTESIAN_POINT ( 'NONE',  ( 12.37861635401602456, 32.45732457598138154, -6.338864116293123629 ) ) ;
#17885 = ORIENTED_EDGE ( 'NONE', *, *, #16800, .F. ) ;
#17886 = CARTESIAN_POINT ( 'NONE',  ( -18.47830230920279959, 9.218715770337659876, -27.17425712858404907 ) ) ;
#17887 = CARTESIAN_POINT ( 'NONE',  ( 10.63499050845688920, 32.74860482968688302, 10.94611345180490503 ) ) ;
#17888 = CARTESIAN_POINT ( 'NONE',  ( -14.83015932036200013, 20.24775513186575537, 7.485646746502382598 ) ) ;
#17889 = ADVANCED_FACE ( 'NONE', ( #7184 ), #19582, .T. ) ;
#17890 = CARTESIAN_POINT ( 'NONE',  ( 11.54108096491583701, -20.40438889209876905, -20.49457141818385253 ) ) ;
#17891 = FACE_OUTER_BOUND ( 'NONE', #5490, .T. ) ;
#17892 = CARTESIAN_POINT ( 'NONE',  ( -8.927394655428429360, 11.06314620770957013, 11.00000000000000000 ) ) ;
#17893 = CARTESIAN_POINT ( 'NONE',  ( -12.92333245884202242, 21.66144175116086856, -17.43645980981951737 ) ) ;
#17894 = CARTESIAN_POINT ( 'NONE',  ( -13.73731780760944332, -15.49063096320742083, -27.84253586294682137 ) ) ;
#17895 = CARTESIAN_POINT ( 'NONE',  ( 9.195945848978588799, -18.32167064559432035, -29.35440300966851623 ) ) ;
#17896 = CYLINDRICAL_SURFACE ( 'NONE', #5582, 0.5000000000000004441 ) ;
#17897 = ORIENTED_EDGE ( 'NONE', *, *, #21444, .T. ) ;
#17898 = ORIENTED_EDGE ( 'NONE', *, *, #7631, .T. ) ;
#17899 = CARTESIAN_POINT ( 'NONE',  ( -11.70053153659217315, 32.50725898910726386, -8.095625848918006184 ) ) ;
#17900 = AXIS2_PLACEMENT_3D ( 'NONE', #11881, #36666, #8836 ) ;
#17901 = DIRECTION ( 'NONE',  ( 0.6691306063588670083, 0.7431448254773863615, 0.000000000000000000 ) ) ;
#17902 = CARTESIAN_POINT ( 'NONE',  ( 3.326583613081083968, 38.15036234293572193, 13.00000000000000178 ) ) ;
#17903 = AXIS2_PLACEMENT_3D ( 'NONE', #123, #6599, #13095 ) ;
#17904 = CARTESIAN_POINT ( 'NONE',  ( -8.981834765181659463, 10.98821582489678583, 10.99387789255783510 ) ) ;
#17905 = ORIENTED_EDGE ( 'NONE', *, *, #6024, .T. ) ;
#17906 = CARTESIAN_POINT ( 'NONE',  ( 30.82841397905490055, -0.0004293619779054370315, -5.946085982635294087 ) ) ;
#17907 = CARTESIAN_POINT ( 'NONE',  ( -6.348113209407908464, 9.835177808069893501, 13.00000000000000178 ) ) ;
#17908 = CARTESIAN_POINT ( 'NONE',  ( -7.611215932167762155, 18.68301270189229513, 7.000000000000000000 ) ) ;
#17909 = ORIENTED_EDGE ( 'NONE', *, *, #9645, .F. ) ;
#17910 = CARTESIAN_POINT ( 'NONE',  ( -20.60997075700326775, 0.8574756231443084742, -28.07786192183081653 ) ) ;
#17911 = PLANE ( 'NONE',  #38444 ) ;
#17912 = ORIENTED_EDGE ( 'NONE', *, *, #306, .F. ) ;
#17913 = CARTESIAN_POINT ( 'NONE',  ( 28.35998102576435542, -3.361797673834487021, -15.09859322067980436 ) ) ;
#17914 = CARTESIAN_POINT ( 'NONE',  ( 36.79828514077289725, -9.052677438810906807, 13.92931973827808534 ) ) ;
#17915 = VERTEX_POINT ( 'NONE', #16140 ) ;
#17916 = CARTESIAN_POINT ( 'NONE',  ( -11.85731412588568823, 35.03474529413922056, 14.53008259254079171 ) ) ;
#17917 = ADVANCED_FACE ( 'NONE', ( #16544 ), #28926, .F. ) ;
#17918 = CARTESIAN_POINT ( 'NONE',  ( 5.730292628140436939, -18.69445663741131014, 20.25080042701566541 ) ) ;
#17919 = CARTESIAN_POINT ( 'NONE',  ( 6.348106467989403257, 35.16482219193073178, 13.00000000000000178 ) ) ;
#17920 = CARTESIAN_POINT ( 'NONE',  ( -4.183427099969815544, 31.55590659971976919, 20.25080042701566185 ) ) ;
#17921 = CARTESIAN_POINT ( 'NONE',  ( -15.26585111513660209, 17.86474508437623143, 13.00000000000000178 ) ) ;
#17922 = ORIENTED_EDGE ( 'NONE', *, *, #10295, .F. ) ;
#17923 = CARTESIAN_POINT ( 'NONE',  ( 10.59792294478272723, 33.06643021166726015, 10.49999999999999467 ) ) ;
#17924 = CARTESIAN_POINT ( 'NONE',  ( 4.980911888400607168, 31.22871793335020030, 10.49999999999999822 ) ) ;
#17925 = CONICAL_SURFACE ( 'NONE', #24404, 1.000000000000002665, 0.7853981633974469467 ) ;
#17926 = AXIS2_PLACEMENT_3D ( 'NONE', #5829, #6020, #6221 ) ;
#17927 = CARTESIAN_POINT ( 'NONE',  ( 7.982650572986060844, 35.32968916061959419, -8.454540784394524167 ) ) ;
#17928 = VECTOR ( 'NONE', #17086, 1000.000000000000000 ) ;
#17929 = DIRECTION ( 'NONE',  ( -0.4731467892558353650, -0.5254827454987470725, 0.7071067811865425767 ) ) ;
#17930 = CARTESIAN_POINT ( 'NONE',  ( 24.20198940123849951, -6.620595927253059898, 20.94377226548378346 ) ) ;
#17931 = AXIS2_PLACEMENT_3D ( 'NONE', #36763, #8933, #21324 ) ;
#17932 = CARTESIAN_POINT ( 'NONE',  ( 16.28755400353538718, -21.47407573242956857, -17.03663477892219547 ) ) ;
#17933 = CARTESIAN_POINT ( 'NONE',  ( 17.34253826607184479, 27.32041144404033162, 11.00000000000000000 ) ) ;
#17934 = DIRECTION ( 'NONE',  ( -0.000000000000000000, -0.000000000000000000, -1.000000000000000000 ) ) ;
#17935 = DIRECTION ( 'NONE',  ( 0.000000000000000000, 0.000000000000000000, 1.000000000000000000 ) ) ;
#17936 = VERTEX_POINT ( 'NONE', #31778 ) ;
#17937 = CARTESIAN_POINT ( 'NONE',  ( 10.98606895505122338, 17.46037643935285999, -28.07419226985351557 ) ) ;
#17938 = VERTEX_POINT ( 'NONE', #32183 ) ;
#17939 = CARTESIAN_POINT ( 'NONE',  ( -15.20434278248479210, 25.80297669556701834, -8.770905639422021949 ) ) ;
#17940 = CARTESIAN_POINT ( 'NONE',  ( -32.94564365859725541, -13.95995841273573390, 18.42518152272108622 ) ) ;
#17941 = CARTESIAN_POINT ( 'NONE',  ( -3.585007771387415332, 8.038731668389095475, 10.82238861112328010 ) ) ;
#17942 = CARTESIAN_POINT ( 'NONE',  ( 15.21665582495734625, 26.14138673791106982, -8.298772713743886698 ) ) ;
#17943 = ORIENTED_EDGE ( 'NONE', *, *, #11789, .T. ) ;
#17944 = CARTESIAN_POINT ( 'NONE',  ( 20.07973543493038093, -12.71120667207603638, -21.84040384482505814 ) ) ;
#17945 = ORIENTED_EDGE ( 'NONE', *, *, #33758, .F. ) ;
#17947 = DIRECTION ( 'NONE',  ( 0.000000000000000000, 0.000000000000000000, 1.000000000000000000 ) ) ;
#17946 = CARTESIAN_POINT ( 'NONE',  ( -10.71119831444032222, 17.63713612967008260, -28.05781784345192165 ) ) ;
#17948 = CARTESIAN_POINT ( 'NONE',  ( -15.78324407152631181, -23.72706283566519048, -14.26634486285669290 ) ) ;
#17949 = CARTESIAN_POINT ( 'NONE',  ( 6.576253646258392926, 14.29921418520925869, 10.50000000000000000 ) ) ;
#17950 = ORIENTED_EDGE ( 'NONE', *, *, #20583, .F. ) ;
#17951 = CARTESIAN_POINT ( 'NONE',  ( -22.28223702159144537, -7.691998452970532085, -21.94978931996465477 ) ) ;
#17952 = CARTESIAN_POINT ( 'NONE',  ( -14.83319764216063774, -26.20259247624118970, -8.300228564017693600 ) ) ;
#17953 = CARTESIAN_POINT ( 'NONE',  ( 14.48927117870122494, -30.61587158504688233, 11.00000000000000000 ) ) ;
#17954 = ORIENTED_EDGE ( 'NONE', *, *, #33510, .F. ) ;
#17955 = CARTESIAN_POINT ( 'NONE',  ( 24.80179831294707782, 2.145886827218380422, -16.59895774698153303 ) ) ;
#17956 = DIRECTION ( 'NONE',  ( 1.000000000000000000, 0.000000000000000000, 0.000000000000000000 ) ) ;
#17957 = CARTESIAN_POINT ( 'NONE',  ( 8.118377661053324701, 10.47536095541698486, 7.000000000000000000 ) ) ;
#17958 = VERTEX_POINT ( 'NONE', #29131 ) ;
#17959 = CARTESIAN_POINT ( 'NONE',  ( -20.61531321053539756, 0.7630595300999895025, -28.07314328191137065 ) ) ;
#17960 = EDGE_LOOP ( 'NONE', ( #37926, #754, #22332 ) ) ;
#17961 = CARTESIAN_POINT ( 'NONE',  ( 29.62581357150819983, -0.8124887880752176272, -11.51961869691573703 ) ) ;
#17962 = CARTESIAN_POINT ( 'NONE',  ( 21.96131288150857586, -24.83662238097890906, 18.42518152272107912 ) ) ;
#17963 = AXIS2_PLACEMENT_3D ( 'NONE', #37468, #28515, #25663 ) ;
#17964 = ADVANCED_FACE ( 'NONE', ( #22419 ), #3940, .F. ) ;
#17965 = ORIENTED_EDGE ( 'NONE', *, *, #34596, .T. ) ;
#17966 = CARTESIAN_POINT ( 'NONE',  ( -27.71315567531769375, 2.639235371980216627, -9.283902402946985433 ) ) ;
#17967 = CARTESIAN_POINT ( 'NONE',  ( 12.05832241004688399, 18.99596958976722760, -30.00000000000000000 ) ) ;
#17968 = DIRECTION ( 'NONE',  ( 0.000000000000000000, 0.000000000000000000, 1.000000000000000000 ) ) ;
#17969 = DIRECTION ( 'NONE',  ( 1.000000000000000000, 0.000000000000000000, 0.000000000000000000 ) ) ;
#17970 = EDGE_CURVE ( 'NONE', #35955, #15787, #32332, .T. ) ;
#17971 = LINE ( 'NONE', #24848, #35717 ) ;
#17972 = EDGE_CURVE ( 'NONE', #14996, #15951, #7991, .T. ) ;
#17973 = CARTESIAN_POINT ( 'NONE',  ( -8.917741276437942233, 30.52956727630665057, 6.000000000000000000 ) ) ;
#17974 = CARTESIAN_POINT ( 'NONE',  ( -5.464848148916058967, 36.46930998210962116, 7.485699520496980064 ) ) ;
#17975 = ORIENTED_EDGE ( 'NONE', *, *, #40194, .T. ) ;
#17976 = CARTESIAN_POINT ( 'NONE',  ( -25.02193947835522536, 6.168178570904315983, -9.344460451553976199 ) ) ;
#17977 = FACE_OUTER_BOUND ( 'NONE', #36262, .T. ) ;
#17978 = DIRECTION ( 'NONE',  ( 0.5877852522924690293, -0.8090169943749503378, 0.000000000000000000 ) ) ;
#17979 = CARTESIAN_POINT ( 'NONE',  ( 24.74805592918939112, -25.69571450645518240, -8.048384647129612546 ) ) ;
#17980 = DIRECTION ( 'NONE',  ( 0.000000000000000000, 0.000000000000000000, 1.000000000000000000 ) ) ;
#17981 = CARTESIAN_POINT ( 'NONE',  ( 11.03704933452659098, 18.24793296388573083, -24.97710597946171518 ) ) ;
#17982 = CIRCLE ( 'NONE', #29630, 2.000000000000000000 ) ;
#17983 = CARTESIAN_POINT ( 'NONE',  ( 4.261257190324624642E-14, -26.71495157282352650, 12.14047268033097460 ) ) ;
#17984 = ORIENTED_EDGE ( 'NONE', *, *, #25674, .T. ) ;
#17986 = AXIS2_PLACEMENT_3D ( 'NONE', #38666, #23827, #23231 ) ;
#17985 = CARTESIAN_POINT ( 'NONE',  ( -15.42171207023761426, 20.87087894025797752, -13.66180630862146117 ) ) ;
#17987 = CARTESIAN_POINT ( 'NONE',  ( -25.20894334605400999, -14.55439022682983996, 20.94377226548377990 ) ) ;
#17988 = ADVANCED_FACE ( 'NONE', ( #17160 ), #27289, .F. ) ;
#17989 = ADVANCED_FACE ( 'NONE', ( #17361 ), #16181, .T. ) ;
#17990 = DIRECTION ( 'NONE',  ( 0.000000000000000000, 0.000000000000000000, 1.000000000000000000 ) ) ;
#17991 = CARTESIAN_POINT ( 'NONE',  ( 14.94931401584148034, 25.75487660405273616, -9.709665385797562109 ) ) ;
#17992 = ORIENTED_EDGE ( 'NONE', *, *, #37930, .T. ) ;
#17993 = CARTESIAN_POINT ( 'NONE',  ( -14.97009266215795087, 21.42933399866955213, 10.59344459855567422 ) ) ;
#17994 = ORIENTED_EDGE ( 'NONE', *, *, #38640, .T. ) ;
#17996 = CARTESIAN_POINT ( 'NONE',  ( 6.811226782241714517, 35.33967249274190436, 10.49999999999999822 ) ) ;
#17995 = CARTESIAN_POINT ( 'NONE',  ( -14.77757630377099929, 25.80207083792462441, -10.16863076474116312 ) ) ;
#17997 = CARTESIAN_POINT ( 'NONE',  ( -15.34706751505450661, -26.51099793413068184, -7.357307595070670558 ) ) ;
#17998 = CARTESIAN_POINT ( 'NONE',  ( -22.48079666807009147, 18.61591633964213344, 10.99999999999999645 ) ) ;
#17999 = VECTOR ( 'NONE', #7002, 1000.000000000000000 ) ;
#18000 = CARTESIAN_POINT ( 'NONE',  ( -17.91007841644879761, -10.80895702151930848, -26.96531573143874638 ) ) ;
#18001 = CARTESIAN_POINT ( 'NONE',  ( -13.94379063328525525, -26.36485034788368864, -5.474070472473820281 ) ) ;
#18002 = CARTESIAN_POINT ( 'NONE',  ( -21.91981567634955042, -15.65087685632102499, 20.99999999999999645 ) ) ;
#18003 = CARTESIAN_POINT ( 'NONE',  ( 16.07071250763885217, 24.35835661434920141, -6.420932443739101103 ) ) ;
#18004 = EDGE_LOOP ( 'NONE', ( #4079, #14218, #23638, #24276 ) ) ;
#18005 = CARTESIAN_POINT ( 'NONE',  ( 25.16591491352843235, 6.464046969047158697, -7.403904741422770996 ) ) ;
#18006 = DIRECTION ( 'NONE',  ( 1.000000000000000000, 0.000000000000000000, 0.000000000000000000 ) ) ;
#18007 = CARTESIAN_POINT ( 'NONE',  ( 8.118377661053324701, 10.47536095541698486, 7.500000000000000888 ) ) ;
#18008 = LINE ( 'NONE', #36486, #12180 ) ;
#18009 = ORIENTED_EDGE ( 'NONE', *, *, #28678, .F. ) ;
#18010 = CARTESIAN_POINT ( 'NONE',  ( -30.79868169068296879, -1.128537211814402585, -9.633236635348129795 ) ) ;
#18011 = CARTESIAN_POINT ( 'NONE',  ( 31.01989312948269628, -0.1972547478048194691, -5.943848862614698803 ) ) ;
#18012 = DIRECTION ( 'NONE',  ( -0.9135454576426005335, 0.4067366430758009299, -0.000000000000000000 ) ) ;
#18013 = CARTESIAN_POINT ( 'NONE',  ( 28.51362642450516915, -10.10416295265137165, 20.50957957746028981 ) ) ;
#18014 = EDGE_CURVE ( 'NONE', #20455, #1674, #1831, .T. ) ;
#18015 = CARTESIAN_POINT ( 'NONE',  ( 23.06249103411542478, 13.31513540672987972, -13.39439507595155199 ) ) ;
#18016 = CARTESIAN_POINT ( 'NONE',  ( 34.10020663062365287, -21.93670956716284337, 10.99999999999993960 ) ) ;
#18017 = VECTOR ( 'NONE', #38973, 1000.000000000000000 ) ;
#18018 = VERTEX_POINT ( 'NONE', #39275 ) ;
#18019 = DIRECTION ( 'NONE',  ( 0.6691306063588569053, -0.7431448254773954654, 0.000000000000000000 ) ) ;
#18020 = CIRCLE ( 'NONE', #32958, 0.9999999999999985567 ) ;
#18021 = AXIS2_PLACEMENT_3D ( 'NONE', #39329, #23889, #36293 ) ;
#18022 = CARTESIAN_POINT ( 'NONE',  ( -20.57678504286234755, 23.15270735508189759, 22.99999999999999645 ) ) ;
#18023 = FACE_OUTER_BOUND ( 'NONE', #28604, .T. ) ;
#18024 = CARTESIAN_POINT ( 'NONE',  ( 1.244695916669324998, 30.19017886107374693, -15.67990371887574952 ) ) ;
#18025 = FACE_OUTER_BOUND ( 'NONE', #26472, .T. ) ;
#18026 = CARTESIAN_POINT ( 'NONE',  ( -8.339609403135948895, 11.87216320208451314, 7.000000000000000000 ) ) ;
#18027 = LINE ( 'NONE', #30811, #2553 ) ;
#18028 = CARTESIAN_POINT ( 'NONE',  ( -21.39877161664097827, 15.54711762656374141, 11.00000000000000000 ) ) ;
#18029 = CARTESIAN_POINT ( 'NONE',  ( -11.89031881743725982, 33.20608791387860492, 12.00000000000000000 ) ) ;
#18030 = CARTESIAN_POINT ( 'NONE',  ( 14.44975846301061928, 26.39485539169812967, 10.49999999999999822 ) ) ;
#18031 = CARTESIAN_POINT ( 'NONE',  ( 12.96901561809162651, 24.98310741220821996, -14.31814338936165498 ) ) ;
#18032 = CARTESIAN_POINT ( 'NONE',  ( 13.48130249190479191, 27.93180293473185927, 7.500000000000000888 ) ) ;
#18033 = VERTEX_POINT ( 'NONE', #20604 ) ;
#18035 = DIRECTION ( 'NONE',  ( 0.000000000000000000, 0.000000000000000000, 1.000000000000000000 ) ) ;
#18034 = CARTESIAN_POINT ( 'NONE',  ( -15.92546573256853648, 12.96094696367512533, -28.84886678414710914 ) ) ;
#18036 = DIRECTION ( 'NONE',  ( 0.000000000000000000, 0.000000000000000000, 1.000000000000000000 ) ) ;
#18037 = CARTESIAN_POINT ( 'NONE',  ( 11.91801038985816596, -21.48403732790968235, -18.45078833793485273 ) ) ;
#18038 = ADVANCED_FACE ( 'NONE', ( #5545 ), #544, .T. ) ;
#18039 = CARTESIAN_POINT ( 'NONE',  ( 12.93090914344494813, 21.64873284080854887, -17.43820100889082170 ) ) ;
#18040 = CARTESIAN_POINT ( 'NONE',  ( 15.35905905661863180, 26.71843228421901628, -6.416469466895263096 ) ) ;
#18041 = EDGE_LOOP ( 'NONE', ( #13928, #31914, #27040, #13953 ) ) ;
#18042 = DIRECTION ( 'NONE',  ( 0.2079116908177532919, -0.9781476007338070211, -0.000000000000000000 ) ) ;
#18043 = LINE ( 'NONE', #29821, #8373 ) ;
#18044 = CIRCLE ( 'NONE', #8288, 0.5000000000000004441 ) ;
#18045 = AXIS2_PLACEMENT_3D ( 'NONE', #27535, #3346, #36879 ) ;
#18046 = CARTESIAN_POINT ( 'NONE',  ( -23.70091659983786414, -19.77374023286659721, -14.78722173017111174 ) ) ;
#18047 = CARTESIAN_POINT ( 'NONE',  ( 1.236634163872074366, -20.51914614933548719, -29.42994913469717488 ) ) ;
#18048 = CARTESIAN_POINT ( 'NONE',  ( 11.33092883969515441, 17.46816179166363980, -26.84939659920764043 ) ) ;
#18049 = CARTESIAN_POINT ( 'NONE',  ( 20.64747291529165807, 12.71173510070245882, -10.38670938929076115 ) ) ;
#18050 = DIRECTION ( 'NONE',  ( 0.000000000000000000, 0.000000000000000000, 1.000000000000000000 ) ) ;
#18051 = CARTESIAN_POINT ( 'NONE',  ( -5.326384147119485490, 37.63231972733477448, -4.999999999999993783 ) ) ;
#18052 = CIRCLE ( 'NONE', #10917, 1.000000000000000000 ) ;
#18053 = ORIENTED_EDGE ( 'NONE', *, *, #86, .T. ) ;
#18054 = CIRCLE ( 'NONE', #14824, 6.000000000000012434 ) ;
#18055 = CARTESIAN_POINT ( 'NONE',  ( -25.66376117784755095, 8.978964872303784261, 12.14047268033272786 ) ) ;
#18056 = ORIENTED_EDGE ( 'NONE', *, *, #21043, .F. ) ;
#18057 = DIRECTION ( 'NONE',  ( -0.000000000000000000, -0.000000000000000000, -1.000000000000000000 ) ) ;
#18058 = DIRECTION ( 'NONE',  ( 1.000000000000000000, 0.000000000000000000, 0.000000000000000000 ) ) ;
#18059 = CARTESIAN_POINT ( 'NONE',  ( -30.14481262437536913, 0.2169452752166688425, -8.299854351458789026 ) ) ;
#18060 = EDGE_CURVE ( 'NONE', #7748, #2515, #24527, .T. ) ;
#18061 = CARTESIAN_POINT ( 'NONE',  ( 29.16243740633159476, -8.764958120439876765, -14.83744052011651249 ) ) ;
#18062 = EDGE_CURVE ( 'NONE', #8408, #36861, #29717, .T. ) ;
#18063 = ORIENTED_EDGE ( 'NONE', *, *, #10113, .T. ) ;
#18064 = DIRECTION ( 'NONE',  ( 0.000000000000000000, 0.000000000000000000, 1.000000000000000000 ) ) ;
#18065 = ORIENTED_EDGE ( 'NONE', *, *, #34244, .T. ) ;
#18066 = LINE ( 'NONE', #20908, #37236 ) ;
#18067 = LINE ( 'NONE', #14811, #9759 ) ;
#18068 = CIRCLE ( 'NONE', #26499, 0.5000000000000004441 ) ;
#18069 = AXIS2_PLACEMENT_3D ( 'NONE', #28723, #10851, #7385 ) ;
#18070 = EDGE_CURVE ( 'NONE', #12849, #15047, #14493, .T. ) ;
#18071 = FACE_OUTER_BOUND ( 'NONE', #32977, .T. ) ;
#18072 = ORIENTED_EDGE ( 'NONE', *, *, #37560, .F. ) ;
#18073 = CARTESIAN_POINT ( 'NONE',  ( -6.980762143445980783, 14.59310681135558063, 10.50000000000000000 ) ) ;
#18074 = LINE ( 'NONE', #21114, #29938 ) ;
#18075 = VECTOR ( 'NONE', #32812, 1000.000000000000000 ) ;
#18076 = LINE ( 'NONE', #11771, #11112 ) ;
#18077 = CARTESIAN_POINT ( 'NONE',  ( 17.00786847495595566, -13.87811437483023980, -24.29345988331185424 ) ) ;
#18078 = CARTESIAN_POINT ( 'NONE',  ( 19.86842276243890382, 14.78994251298874296, -8.402377087950958057 ) ) ;
#18079 = CIRCLE ( 'NONE', #32927, 0.5000000000000004441 ) ;
#18080 = CARTESIAN_POINT ( 'NONE',  ( 9.808884097217401177, 27.70084310347472822, -14.97692238110015417 ) ) ;
#18081 = ORIENTED_EDGE ( 'NONE', *, *, #14101, .F. ) ;
#18082 = CARTESIAN_POINT ( 'NONE',  ( -18.65382632816861275, 9.289903503710515764, -25.50617801253576999 ) ) ;
#18083 = CARTESIAN_POINT ( 'NONE',  ( 0.000000000000000000, 22.50000000000000355, 6.000000000000000000 ) ) ;
#18084 = CARTESIAN_POINT ( 'NONE',  ( 2.853166178176219425, 23.42705098312512746, 12.00000000000000000 ) ) ;
#18085 = CARTESIAN_POINT ( 'NONE',  ( 15.10432571242179911, -26.01895073574682726, -9.232258709681612885 ) ) ;
#18086 = DIRECTION ( 'NONE',  ( 0.000000000000000000, 0.000000000000000000, 1.000000000000000000 ) ) ;
#18087 = EDGE_CURVE ( 'NONE', #15193, #27705, #27146, .T. ) ;
#18088 = ADVANCED_FACE ( 'NONE', ( #32594 ), #5351, .T. ) ;
#18089 = CARTESIAN_POINT ( 'NONE',  ( 27.08779848459123585, 7.221796966026769127, -13.42901749168596304 ) ) ;
#18090 = ADVANCED_FACE ( 'NONE', ( #39674 ), #11849, .F. ) ;
#18091 = CARTESIAN_POINT ( 'NONE',  ( -13.18985422166703181, 22.27197207924475109, -16.43952829204636146 ) ) ;
#18092 = CARTESIAN_POINT ( 'NONE',  ( -16.53877156149134819, -18.57266078395657161, -19.93956889360425322 ) ) ;
#18093 = CARTESIAN_POINT ( 'NONE',  ( 13.17310952450038464, -25.48991742312072262, -9.735372911299624121 ) ) ;
#18094 = LINE ( 'NONE', #23977, #12707 ) ;
#18095 = ORIENTED_EDGE ( 'NONE', *, *, #32309, .F. ) ;
#18096 = VERTEX_POINT ( 'NONE', #24832 ) ;
#18097 = CARTESIAN_POINT ( 'NONE',  ( -11.15150138062039709, 34.02824952835918992, -5.447195920641812350 ) ) ;
#18098 = CARTESIAN_POINT ( 'NONE',  ( 0.8726219063013830324, 37.33905845025570613, 10.49999999999999822 ) ) ;
#18099 = CARTESIAN_POINT ( 'NONE',  ( 10.06946225350410984, 32.23940090176269990, 7.000000000000000000 ) ) ;
#18100 = AXIS2_PLACEMENT_3D ( 'NONE', #23698, #36097, #8051 ) ;
#18101 = CIRCLE ( 'NONE', #7704, 1.000000000000000888 ) ;
#18102 = CARTESIAN_POINT ( 'NONE',  ( -9.221287281574706896, 10.65863771052213238, 10.59344459855561915 ) ) ;
#18103 = ORIENTED_EDGE ( 'NONE', *, *, #30515, .T. ) ;
#18104 = CARTESIAN_POINT ( 'NONE',  ( 20.48067366615298468, 0.8901913013804804153, -30.00000000000000000 ) ) ;
#18105 = CARTESIAN_POINT ( 'NONE',  ( -18.23649648353780961, -16.09146789626143814, 23.00000000000000000 ) ) ;
#18106 = DIRECTION ( 'NONE',  ( 0.000000000000000000, 0.000000000000000000, 1.000000000000000000 ) ) ;
#18107 = AXIS2_PLACEMENT_3D ( 'NONE', #31937, #13449, #38642 ) ;
#18108 = ORIENTED_EDGE ( 'NONE', *, *, #38179, .F. ) ;
#18109 = CARTESIAN_POINT ( 'NONE',  ( -30.87691200222618804, -0.01437998035276831163, -4.999999999999999112 ) ) ;
#18110 = CARTESIAN_POINT ( 'NONE',  ( -9.393455880287618243, 11.27231877233277224, 10.49999999999999822 ) ) ;
#18111 = EDGE_CURVE ( 'NONE', #15686, #37263, #30402, .T. ) ;
#18112 = ORIENTED_EDGE ( 'NONE', *, *, #15601, .F. ) ;
#18113 = CARTESIAN_POINT ( 'NONE',  ( 34.26529024853127936, -5.222454321802834087, -5.897803579761220938 ) ) ;
#18114 = CARTESIAN_POINT ( 'NONE',  ( 20.77381726376787086, -29.00435581194094325, 12.73282698324852724 ) ) ;
#18115 = EDGE_CURVE ( 'NONE', #25178, #17580, #23254, .T. ) ;
#18116 = ORIENTED_EDGE ( 'NONE', *, *, #7539, .T. ) ;
#18117 = CARTESIAN_POINT ( 'NONE',  ( -16.03057579645021491, 28.88256098452011145, 14.53008259253939194 ) ) ;
#18118 = DIRECTION ( 'NONE',  ( 1.000000000000000000, 0.000000000000000000, 0.000000000000000000 ) ) ;
#18119 = FACE_OUTER_BOUND ( 'NONE', #16461, .T. ) ;
#18120 = CARTESIAN_POINT ( 'NONE',  ( 1.161969254298447884, 33.23463598332013191, 19.99202127657103034 ) ) ;
#18121 = CARTESIAN_POINT ( 'NONE',  ( 2.211395437248501850, 12.61633075744433796, 13.00000000000000178 ) ) ;
#18122 = ORIENTED_EDGE ( 'NONE', *, *, #13451, .T. ) ;
#18123 = CARTESIAN_POINT ( 'NONE',  ( -10.14060191828654212, 25.26915018278947755, 10.50000000000000000 ) ) ;
#18124 = DIRECTION ( 'NONE',  ( 0.000000000000000000, 0.000000000000000000, 1.000000000000000000 ) ) ;
#18125 = AXIS2_PLACEMENT_3D ( 'NONE', #39364, #27373, #33493 ) ;
#18127 = AXIS2_PLACEMENT_3D ( 'NONE', #24514, #6023, #27763 ) ;
#18126 = CARTESIAN_POINT ( 'NONE',  ( 7.809096289090598830, 34.47606966685644636, -9.783655936083253124 ) ) ;
#18128 = CARTESIAN_POINT ( 'NONE',  ( -2.672146553953452575, 12.33340603770394139, 10.50000000000000000 ) ) ;
#18129 = CARTESIAN_POINT ( 'NONE',  ( 7.962467718759976165, 24.71319220552188156, 20.69868183039781329 ) ) ;
#18130 = CARTESIAN_POINT ( 'NONE',  ( 19.25558875303204687, -26.58026616919283924, -8.617268851883771674 ) ) ;
#18131 = VECTOR ( 'NONE', #33366, 999.9999999999998863 ) ;
#18132 = CARTESIAN_POINT ( 'NONE',  ( -14.01838097023000707, 23.73363068877903359, 6.000000000000000000 ) ) ;
#18133 = CARTESIAN_POINT ( 'NONE',  ( 10.32951289851633270, 32.69782367585502669, 10.83333333333333037 ) ) ;
#18134 = VERTEX_POINT ( 'NONE', #24633 ) ;
#18135 = CARTESIAN_POINT ( 'NONE',  ( 11.14038654638060244, 17.78806815055257573, -26.22011444304219907 ) ) ;
#18136 = VERTEX_POINT ( 'NONE', #24435 ) ;
#18137 = CARTESIAN_POINT ( 'NONE',  ( -11.06345206700481931, 17.40955828997764243, -28.07880555279562174 ) ) ;
#18138 = CARTESIAN_POINT ( 'NONE',  ( -26.60725962520553622, -21.34341596033566901, 19.27171037444156809 ) ) ;
#18139 = CARTESIAN_POINT ( 'NONE',  ( 12.56610953508889494, -22.55658933108479758, -16.45058249204709355 ) ) ;
#18140 = CARTESIAN_POINT ( 'NONE',  ( -13.39464589777671044, 26.66807349098043289, 12.00000000000000000 ) ) ;
#18141 = CARTESIAN_POINT ( 'NONE',  ( 15.46782449521607283, 26.59794325776330481, -5.474156741759839129 ) ) ;
#18142 = EDGE_LOOP ( 'NONE', ( #26872, #32755, #17898, #29919 ) ) ;
#18143 = CARTESIAN_POINT ( 'NONE',  ( 31.77261430474117532, -21.49768664888851788, -5.435972644969311318 ) ) ;
#18144 = ORIENTED_EDGE ( 'NONE', *, *, #38050, .F. ) ;
#18146 = CARTESIAN_POINT ( 'NONE',  ( 8.247851828378060191, 9.985713325475870761, 10.49999999999999822 ) ) ;
#18145 = CARTESIAN_POINT ( 'NONE',  ( -14.73108631288593529, 28.24757970853271516, -7.312183354124210055 ) ) ;
#18147 = CARTESIAN_POINT ( 'NONE',  ( -17.13315098722738483, -24.25158645364346910, -13.25521884679562490 ) ) ;
#18148 = CARTESIAN_POINT ( 'NONE',  ( 4.336808689942017736E-15, 40.84107189184581443, -5.000000000000008882 ) ) ;
#18149 = ORIENTED_EDGE ( 'NONE', *, *, #38612, .F. ) ;
#18150 = CARTESIAN_POINT ( 'NONE',  ( -32.58686633885861994, -12.27975601045717191, -11.10035766972282190 ) ) ;
#18151 = CARTESIAN_POINT ( 'NONE',  ( -14.90633381827083070, -26.31176259071834522, -7.829649256883607578 ) ) ;
#18152 = CARTESIAN_POINT ( 'NONE',  ( 36.53988293556055567, -0.5802930328960469453, 23.00000000000094147 ) ) ;
#18153 = ORIENTED_EDGE ( 'NONE', *, *, #34014, .F. ) ;
#18154 = CARTESIAN_POINT ( 'NONE',  ( 23.35664678750010381, 2.976149040520807532, -18.70198339929852338 ) ) ;
#18155 = DIRECTION ( 'NONE',  ( 1.000000000000000000, 0.000000000000000000, 0.000000000000000000 ) ) ;
#18156 = DIRECTION ( 'NONE',  ( 0.000000000000000000, 0.000000000000000000, 1.000000000000000000 ) ) ;
#18157 = ORIENTED_EDGE ( 'NONE', *, *, #4564, .F. ) ;
#18158 = CARTESIAN_POINT ( 'NONE',  ( -30.68763588371861672, -0.09248980374888614298, -7.355207434232696961 ) ) ;
#18159 = EDGE_LOOP ( 'NONE', ( #32774, #15157, #12073, #28724, #39476, #8310, #4958 ) ) ;
#18160 = CARTESIAN_POINT ( 'NONE',  ( 21.03689950211181880, -0.002815931881645192866, -26.15313960796883208 ) ) ;
#18161 = AXIS2_PLACEMENT_3D ( 'NONE', #27310, #17583, #36458 ) ;
#18162 = CARTESIAN_POINT ( 'NONE',  ( 33.72852460920453410, -9.442290196614045783, 17.92354375535250810 ) ) ;
#18163 = VERTEX_POINT ( 'NONE', #15291 ) ;
#18164 = CARTESIAN_POINT ( 'NONE',  ( -22.98279762503596757, 2.766379843953515216, -19.73711539544465410 ) ) ;
#18165 = AXIS2_PLACEMENT_3D ( 'NONE', #40187, #6061, #12358 ) ;
#18166 = DIRECTION ( 'NONE',  ( 0.000000000000000000, 0.000000000000000000, -1.000000000000000000 ) ) ;
#18167 = CARTESIAN_POINT ( 'NONE',  ( 4.984135866956514782, 36.15314577889351000, 10.49999999999999467 ) ) ;
#18168 = CARTESIAN_POINT ( 'NONE',  ( -36.92299321678470392, -6.638097534484090012, 10.99999999999989342 ) ) ;
#18169 = DIRECTION ( 'NONE',  ( 0.2079116908177663092, 0.9781476007338041345, -0.000000000000000000 ) ) ;
#18170 = DIRECTION ( 'NONE',  ( 1.000000000000000000, 0.000000000000000000, 0.000000000000000000 ) ) ;
#18171 = DIRECTION ( 'NONE',  ( 1.000000000000000000, 0.000000000000000000, 0.000000000000000000 ) ) ;
#18172 = ORIENTED_EDGE ( 'NONE', *, *, #29468, .T. ) ;
#18173 = CARTESIAN_POINT ( 'NONE',  ( -21.48723061098553444, 7.511881048007619022, -17.95007373264360595 ) ) ;
#18174 = DIRECTION ( 'NONE',  ( 0.000000000000000000, 0.000000000000000000, 1.000000000000000000 ) ) ;
#18175 = CARTESIAN_POINT ( 'NONE',  ( -11.11016527260153630, 31.83082137946488643, 7.000000000000000000 ) ) ;
#18176 = CARTESIAN_POINT ( 'NONE',  ( 24.96780582346026733, -24.47691348509939857, -9.803478453495912959 ) ) ;
#18177 = DIRECTION ( 'NONE',  ( 0.4156269377774490792, -0.5720614028176843613, -0.7071067811865500152 ) ) ;
#18178 = CARTESIAN_POINT ( 'NONE',  ( 13.06109374962291092, 22.50549497211172323, -16.41044510421365743 ) ) ;
#18179 = CARTESIAN_POINT ( 'NONE',  ( 15.20016916874808288, -27.86040092368543242, 14.53008259254010959 ) ) ;
#18180 = CIRCLE ( 'NONE', #25296, 1.000000000000000888 ) ;
#18181 = EDGE_LOOP ( 'NONE', ( #39029, #24549, #259, #15273 ) ) ;
#18182 = CARTESIAN_POINT ( 'NONE',  ( -13.76573679096662417, 19.44551850793918035, -18.63149991976310460 ) ) ;
#18183 = CARTESIAN_POINT ( 'NONE',  ( -26.76156665933352130, -9.514918190648881335, 20.82122704794052126 ) ) ;
#18184 = EDGE_CURVE ( 'NONE', #3501, #31354, #5944, .T. ) ;
#18185 = CARTESIAN_POINT ( 'NONE',  ( -3.057264508911468948, 12.92643568347973826, 10.50000000000000533 ) ) ;
#18186 = CARTESIAN_POINT ( 'NONE',  ( 14.95212139095325199, 25.74619849441134534, -9.709798330206572459 ) ) ;
#18187 = ORIENTED_EDGE ( 'NONE', *, *, #23839, .F. ) ;
#18188 = PLANE ( 'NONE',  #31337 ) ;
#18189 = AXIS2_PLACEMENT_3D ( 'NONE', #35043, #7198, #19597 ) ;
#18190 = ORIENTED_EDGE ( 'NONE', *, *, #26670, .F. ) ;
#18192 = DIRECTION ( 'NONE',  ( -0.6724985119639631526, -0.2185080122244104639, -0.7071067811865420216 ) ) ;
#18191 = CARTESIAN_POINT ( 'NONE',  ( -15.35513899590904430, 26.99708482749830907, -5.000000000000001776 ) ) ;
#18193 = CARTESIAN_POINT ( 'NONE',  ( -15.57263558642641854, -26.76429566359157164, -5.473788325833539581 ) ) ;
#18194 = LINE ( 'NONE', #30386, #4963 ) ;
#18195 = CARTESIAN_POINT ( 'NONE',  ( -33.36938334175751208, -17.47479766793881240, -7.973135956092645138 ) ) ;
#18196 = CARTESIAN_POINT ( 'NONE',  ( -13.40655439899805756, -25.53642076282103091, -9.731694637308171636 ) ) ;
#18197 = FACE_OUTER_BOUND ( 'NONE', #34237, .T. ) ;
#18198 = CARTESIAN_POINT ( 'NONE',  ( 16.28462322236242343, 23.84466805338936624, -5.948220019300794803 ) ) ;
#18199 = EDGE_CURVE ( 'NONE', #400, #36251, #3118, .T. ) ;
#18200 = ORIENTED_EDGE ( 'NONE', *, *, #27265, .T. ) ;
#18201 = CARTESIAN_POINT ( 'NONE',  ( 24.10931265530348000, 7.304982279079090368, -9.852240822340444737 ) ) ;
#18202 = CARTESIAN_POINT ( 'NONE',  ( 16.66551504892489888, -27.04635334451238649, -4.999999999999997335 ) ) ;
#18203 = CARTESIAN_POINT ( 'NONE',  ( -10.80698216227225394, 13.84996144622306247, 12.00000000000000000 ) ) ;
#18204 = ADVANCED_FACE ( 'NONE', ( #27679 ), #28076, .T. ) ;
#18205 = DIRECTION ( 'NONE',  ( -1.000000000000000000, 0.000000000000000000, 0.000000000000000000 ) ) ;
#18206 = ORIENTED_EDGE ( 'NONE', *, *, #32442, .F. ) ;
#18207 = CARTESIAN_POINT ( 'NONE',  ( -20.74142061204233656, -0.1647452484960928165, -27.38238928991409082 ) ) ;
#18208 = CARTESIAN_POINT ( 'NONE',  ( 29.41506271722083810, 0.006098485709055394971, -10.64827624646466653 ) ) ;
#18209 = CARTESIAN_POINT ( 'NONE',  ( 0.000000000000000000, 22.50000000000000355, 13.00000000000000178 ) ) ;
#18210 = CARTESIAN_POINT ( 'NONE',  ( 26.52908095339053673, -8.732144267389724490, 20.82122704794066692 ) ) ;
#18211 = CARTESIAN_POINT ( 'NONE',  ( 30.41237130417911771, 3.314011747244131723, -13.58461195433497437 ) ) ;
#18212 = DIRECTION ( 'NONE',  ( -0.4156269377774534091, 0.5720614028176876920, -0.7071067811865449082 ) ) ;
#18213 = ADVANCED_FACE ( 'NONE', ( #15092 ), #18745, .F. ) ;
#18214 = ORIENTED_EDGE ( 'NONE', *, *, #12997, .F. ) ;
#18215 = EDGE_CURVE ( 'NONE', #9209, #38623, #456, .T. ) ;
#18216 = AXIS2_PLACEMENT_3D ( 'NONE', #26401, #22952, #17075 ) ;
#18217 = CARTESIAN_POINT ( 'NONE',  ( -5.348113209407908464, 9.835177808069893501, 6.000000000000000000 ) ) ;
#18218 = CARTESIAN_POINT ( 'NONE',  ( -4.188939243032555382, 44.61227686191953268, 11.00000000000000000 ) ) ;
#18219 = CARTESIAN_POINT ( 'NONE',  ( 3.784955426773477072, 9.502919080911357952, 10.50000000000000000 ) ) ;
#18220 = CARTESIAN_POINT ( 'NONE',  ( 3.503895337239875118, 34.07186797344890294, -11.98835608762611216 ) ) ;
#18221 = DIRECTION ( 'NONE',  ( 1.000000000000000000, 0.000000000000000000, 0.000000000000000000 ) ) ;
#18222 = CYLINDRICAL_SURFACE ( 'NONE', #15612, 0.4999999999999997780 ) ;
#18223 = CARTESIAN_POINT ( 'NONE',  ( -13.46929972531958697, 26.35070966310183138, 7.000000000000000000 ) ) ;
#18224 = LINE ( 'NONE', #30812, #34857 ) ;
#18225 = DIRECTION ( 'NONE',  ( -0.3090169943749572767, -0.9510565162951503115, 0.000000000000000000 ) ) ;
#18226 = CARTESIAN_POINT ( 'NONE',  ( 4.940908595777813161, 35.94977745735560859, 7.000000000000000000 ) ) ;
#18227 = CARTESIAN_POINT ( 'NONE',  ( 14.84946995997173325, 27.27879204989079298, -8.260274125225500086 ) ) ;
#18228 = CARTESIAN_POINT ( 'NONE',  ( -4.458872323573595864, 26.51478363815348160, 12.00000000000000000 ) ) ;
#18229 = EDGE_LOOP ( 'NONE', ( #25785, #25379, #16855, #7454 ) ) ;
#18231 = DIRECTION ( 'NONE',  ( -0.5000000000000039968, -0.8660254037844363761, 0.000000000000000000 ) ) ;
#18230 = CARTESIAN_POINT ( 'NONE',  ( -19.46326072101385307, 15.42234476947875699, -8.889095617120403858 ) ) ;
#18232 = CARTESIAN_POINT ( 'NONE',  ( -4.881458130820804264, -28.77689918168226058, 10.99999999999999645 ) ) ;
#18233 = CIRCLE ( 'NONE', #38320, 0.5000000000000024425 ) ;
#18234 = CARTESIAN_POINT ( 'NONE',  ( 15.08555043039248389, -26.14723064015357679, -8.767643119045953171 ) ) ;
#18235 = CARTESIAN_POINT ( 'NONE',  ( -21.68568904104562023, -27.13690135270087822, -4.999999999999999112 ) ) ;
#18236 = CARTESIAN_POINT ( 'NONE',  ( 31.24272016125543772, 0.2902395683448326102, 15.72805884748939498 ) ) ;
#18237 = CARTESIAN_POINT ( 'NONE',  ( 14.72587059535505283, 25.43166455451370567, -10.65085080139201956 ) ) ;
#18238 = ORIENTED_EDGE ( 'NONE', *, *, #8552, .F. ) ;
#18239 = DIRECTION ( 'NONE',  ( 0.000000000000000000, 0.000000000000000000, -1.000000000000000000 ) ) ;
#18240 = ADVANCED_FACE ( 'NONE', ( #18346 ), #2901, .T. ) ;
#18241 = CARTESIAN_POINT ( 'NONE',  ( 11.80736835487432046, 13.95096189432328693, 7.000000000000000000 ) ) ;
#18242 = CARTESIAN_POINT ( 'NONE',  ( -33.41351084210700151, -21.43470647212746272, 14.53008259253988399 ) ) ;
#18243 = CARTESIAN_POINT ( 'NONE',  ( -29.90225311088989812, -23.39525860678804037, -5.437566589666127825 ) ) ;
#18244 = CARTESIAN_POINT ( 'NONE',  ( -0.3830839531904912665, -24.55156499636435186, -8.408222294404422925 ) ) ;
#18245 = CARTESIAN_POINT ( 'NONE',  ( 11.28710791291100435, 17.16441204958988109, -28.71847994827210471 ) ) ;
#18246 = CARTESIAN_POINT ( 'NONE',  ( 22.15128575431291935, 11.07349831676230778, -6.938905347179290750 ) ) ;
#18247 = CYLINDRICAL_SURFACE ( 'NONE', #10200, 1.000000000000000000 ) ;
#18248 = EDGE_CURVE ( 'NONE', #24077, #31037, #6354, .T. ) ;
#18249 = AXIS2_PLACEMENT_3D ( 'NONE', #37945, #29000, #22494 ) ;
#18250 = CARTESIAN_POINT ( 'NONE',  ( -4.192884458248775204, 37.73304570911393085, -6.703245015772555604 ) ) ;
#18251 = ORIENTED_EDGE ( 'NONE', *, *, #23023, .F. ) ;
#18252 = CARTESIAN_POINT ( 'NONE',  ( -20.50046019883160398, -3.737008032862233708, -27.16541881878944764 ) ) ;
#18253 = CARTESIAN_POINT ( 'NONE',  ( -25.01795332078377143, 8.530037020297342565, 14.53008259254123757 ) ) ;
#18254 = ORIENTED_EDGE ( 'NONE', *, *, #34125, .F. ) ;
#18255 = FACE_OUTER_BOUND ( 'NONE', #2069, .T. ) ;
#18256 = DIRECTION ( 'NONE',  ( 1.000000000000000000, 0.000000000000000000, 0.000000000000000000 ) ) ;
#18257 = CARTESIAN_POINT ( 'NONE',  ( -24.90203731630741757, 0.9589847940253315439, -17.49505980781958669 ) ) ;
#18258 = CARTESIAN_POINT ( 'NONE',  ( 32.62865313406591383, -11.96328060321731357, -11.10430041822750447 ) ) ;
#18259 = AXIS2_PLACEMENT_3D ( 'NONE', #20164, #26652, #29502 ) ;
#18260 = AXIS2_PLACEMENT_3D ( 'NONE', #33560, #23799, #30701 ) ;
#18261 = ORIENTED_EDGE ( 'NONE', *, *, #6760, .T. ) ;
#18262 = EDGE_CURVE ( 'NONE', #4778, #23735, #27482, .T. ) ;
#18263 = DIRECTION ( 'NONE',  ( -0.5254827454987577307, -0.4731467892558122723, 0.7071067811865503483 ) ) ;
#18264 = ORIENTED_EDGE ( 'NONE', *, *, #32604, .F. ) ;
#18265 = EDGE_CURVE ( 'NONE', #29319, #20641, #37424, .T. ) ;
#18266 = FACE_OUTER_BOUND ( 'NONE', #25951, .T. ) ;
#18267 = LINE ( 'NONE', #24353, #7893 ) ;
#18268 = FACE_OUTER_BOUND ( 'NONE', #8227, .T. ) ;
#18269 = ORIENTED_EDGE ( 'NONE', *, *, #38920, .F. ) ;
#18270 = CARTESIAN_POINT ( 'NONE',  ( -1.657330241813901317, 20.83889105489772220, -26.97771945235741242 ) ) ;
#18271 = CARTESIAN_POINT ( 'NONE',  ( -25.19768531712390569, 23.50223830518991619, 7.499999999999999112 ) ) ;
#18272 = DIRECTION ( 'NONE',  ( -1.000000000000000000, 0.000000000000000000, 0.000000000000000000 ) ) ;
#18273 = CARTESIAN_POINT ( 'NONE',  ( 2.525645716490518389, 8.212903943950921715, 7.000000000000000000 ) ) ;
#18274 = CARTESIAN_POINT ( 'NONE',  ( 29.07166297330496008, -23.76421018344883862, -6.712234129069530653 ) ) ;
#18275 = CARTESIAN_POINT ( 'NONE',  ( 16.61895836664333714, 12.92996417114949459, -24.37923977068471970 ) ) ;
#18276 = CARTESIAN_POINT ( 'NONE',  ( 13.12592325053682174, 31.71798720882053502, -5.454496241009516133 ) ) ;
#18277 = ORIENTED_EDGE ( 'NONE', *, *, #25063, .T. ) ;
#18278 = CARTESIAN_POINT ( 'NONE',  ( -21.81785358434161637, 11.77199115278586028, -5.482921482795456214 ) ) ;
#18279 = DIRECTION ( 'NONE',  ( -0.8660254037844363761, 0.5000000000000041078, -0.000000000000000000 ) ) ;
#18280 = CARTESIAN_POINT ( 'NONE',  ( 13.12731182914002659, -23.09957666458869951, -15.43892246686051095 ) ) ;
#18281 = CARTESIAN_POINT ( 'NONE',  ( -9.541476348891238857, 27.59512447410525127, 12.00000000000000000 ) ) ;
#18282 = CARTESIAN_POINT ( 'NONE',  ( 13.47223693944937750, 18.09844039693851769, -21.24786896499729139 ) ) ;
#18283 = ADVANCED_FACE ( 'NONE', ( #15495 ), #6533, .F. ) ;
#18284 = CARTESIAN_POINT ( 'NONE',  ( -13.47489597303660069, 22.84936685448861482, -15.44687488758540717 ) ) ;
#18285 = AXIS2_PLACEMENT_3D ( 'NONE', #11171, #22745, #1835 ) ;
#18286 = CARTESIAN_POINT ( 'NONE',  ( -24.97569650337160496, -26.32149808972361527, -5.444941899105278260 ) ) ;
#18287 = CARTESIAN_POINT ( 'NONE',  ( 10.76261159742561802, -25.66954346325781700, -5.000000000000002665 ) ) ;
#18288 = VECTOR ( 'NONE', #24949, 1000.000000000000000 ) ;
#18289 = CARTESIAN_POINT ( 'NONE',  ( -39.35969763408572675, -8.663070498340031733, 11.00000000000000355 ) ) ;
#18290 = ORIENTED_EDGE ( 'NONE', *, *, #6160, .F. ) ;
#18291 = ORIENTED_EDGE ( 'NONE', *, *, #11747, .T. ) ;
#18292 = CARTESIAN_POINT ( 'NONE',  ( -9.771457654459068110, 32.72495824132072784, -10.28232596613767669 ) ) ;
#18293 = EDGE_CURVE ( 'NONE', #26406, #5398, #31872, .T. ) ;
#18294 = CARTESIAN_POINT ( 'NONE',  ( -9.343266739736652227, 17.68301270189230578, 10.50000000000000000 ) ) ;
#18295 = CARTESIAN_POINT ( 'NONE',  ( -14.81329996725647469, 19.93755115561707569, 7.000000000000000000 ) ) ;
#18296 = CARTESIAN_POINT ( 'NONE',  ( -8.927394655428429360, 11.06314620770957013, 10.99999999999999289 ) ) ;
#18297 = VERTEX_POINT ( 'NONE', #21778 ) ;
#18298 = CARTESIAN_POINT ( 'NONE',  ( 30.15129433585467567, 0.04742302619024474364, -8.768128520917576552 ) ) ;
#18299 = CARTESIAN_POINT ( 'NONE',  ( 3.465511072935331782, 38.21601825462830249, -4.999999999999999112 ) ) ;
#18300 = CIRCLE ( 'NONE', #20248, 0.5000000000000002220 ) ;
#18301 = DIRECTION ( 'NONE',  ( -0.000000000000000000, -0.000000000000000000, -1.000000000000000000 ) ) ;
#18302 = VERTEX_POINT ( 'NONE', #6141 ) ;
#18303 = CARTESIAN_POINT ( 'NONE',  ( -29.79738327385628693, 0.04873725983771388937, -9.709267053127604186 ) ) ;
#18304 = CARTESIAN_POINT ( 'NONE',  ( 13.28503138821876917, 15.53523575316134142, 7.499999999999997335 ) ) ;
#18305 = ORIENTED_EDGE ( 'NONE', *, *, #36219, .F. ) ;
#18306 = CARTESIAN_POINT ( 'NONE',  ( 33.87848217329536027, -7.057063397675949368, -8.961058107038109455 ) ) ;
#18307 = ORIENTED_EDGE ( 'NONE', *, *, #28043, .T. ) ;
#18308 = CARTESIAN_POINT ( 'NONE',  ( 3.887054626305054938, 40.11907545043354872, 12.14047268033114690 ) ) ;
#18309 = CARTESIAN_POINT ( 'NONE',  ( -5.661571401657330860, -19.51153516500234630, 19.99202127657103389 ) ) ;
#18310 = DIRECTION ( 'NONE',  ( 1.000000000000000000, 0.000000000000000000, 0.000000000000000000 ) ) ;
#18311 = EDGE_CURVE ( 'NONE', #29828, #22802, #18938, .T. ) ;
#18312 = CARTESIAN_POINT ( 'NONE',  ( 4.528037020496070930, 32.30201321073025156, 19.99202127657103389 ) ) ;
#18313 = DIRECTION ( 'NONE',  ( 0.3090169943749573322, 0.9510565162951504226, 0.000000000000000000 ) ) ;
#18314 = ORIENTED_EDGE ( 'NONE', *, *, #33963, .F. ) ;
#18315 = CYLINDRICAL_SURFACE ( 'NONE', #6756, 0.5000000000000004441 ) ;
#18316 = LINE ( 'NONE', #2874, #10449 ) ;
#18317 = FACE_OUTER_BOUND ( 'NONE', #33782, .T. ) ;
#18318 = CARTESIAN_POINT ( 'NONE',  ( 7.070389571528393979, 36.44087030134537741, -7.144592491976538007 ) ) ;
#18319 = CARTESIAN_POINT ( 'NONE',  ( 3.888911272182352441, 9.013845280544455107, 9.500000000000000000 ) ) ;
#18320 = VECTOR ( 'NONE', #32695, 1000.000000000000000 ) ;
#18321 = CARTESIAN_POINT ( 'NONE',  ( 17.92107859924769286, -26.25758313345151507, -9.565594702903538860 ) ) ;
#18322 = FACE_OUTER_BOUND ( 'NONE', #15280, .T. ) ;
#18323 = FACE_OUTER_BOUND ( 'NONE', #7569, .T. ) ;
#18324 = EDGE_CURVE ( 'NONE', #19863, #26705, #14813, .T. ) ;
#18325 = ORIENTED_EDGE ( 'NONE', *, *, #4556, .F. ) ;
#18326 = CARTESIAN_POINT ( 'NONE',  ( -11.28570022020756092, 17.50099206051545053, -26.84538423779353167 ) ) ;
#18327 = VECTOR ( 'NONE', #5795, 1000.000000000000000 ) ;
#18328 = CARTESIAN_POINT ( 'NONE',  ( -31.84188463419280879, -5.263436490338604834, 18.42518152272108978 ) ) ;
#18329 = CARTESIAN_POINT ( 'NONE',  ( 10.99009283189107222, -20.50363791108294720, -20.56400601000566297 ) ) ;
#18330 = ADVANCED_FACE ( 'NONE', ( #39868 ), #28460, .T. ) ;
#18331 = CARTESIAN_POINT ( 'NONE',  ( -3.699151772512148995, 7.951170058885317360, 10.49999999999999822 ) ) ;
#18332 = ORIENTED_EDGE ( 'NONE', *, *, #6024, .F. ) ;
#18333 = ORIENTED_EDGE ( 'NONE', *, *, #39580, .T. ) ;
#18334 = CARTESIAN_POINT ( 'NONE',  ( -14.41188954600920624, 29.53590640632083719, -5.462209281689084150 ) ) ;
#18335 = CARTESIAN_POINT ( 'NONE',  ( -17.98125570054222067, -25.38052975340228556, -11.37714725492202028 ) ) ;
#18336 = CARTESIAN_POINT ( 'NONE',  ( 6.023418944065099367, 39.81932404830325112, -4.999999999999995559 ) ) ;
#18337 = ORIENTED_EDGE ( 'NONE', *, *, #22762, .F. ) ;
#18338 = EDGE_CURVE ( 'NONE', #7027, #23669, #34827, .T. ) ;
#18339 = CARTESIAN_POINT ( 'NONE',  ( -22.42412062115972660, -6.996450698531886836, -21.99081150208999702 ) ) ;
#18340 = PRODUCT_DEFINITION_CONTEXT ( 'detailed design', #4675, 'design' ) ;
#18341 = CARTESIAN_POINT ( 'NONE',  ( -10.95620176796833611, -20.50974478584956628, -20.56786716869152798 ) ) ;
#18342 = AXIS2_PLACEMENT_3D ( 'NONE', #26051, #6557, #9820 ) ;
#18343 = CARTESIAN_POINT ( 'NONE',  ( 37.88915195766846722, -19.37406375362047228, 11.00000000000000000 ) ) ;
#18344 = VERTEX_POINT ( 'NONE', #16902 ) ;
#18345 = CARTESIAN_POINT ( 'NONE',  ( 20.62687364291603487, 1.714078824949687441, -27.50299618919958178 ) ) ;
#18346 = FACE_OUTER_BOUND ( 'NONE', #29190, .T. ) ;
#18347 = DIRECTION ( 'NONE',  ( 0.1045284632676437703, -0.9945218953682745111, -0.000000000000000000 ) ) ;
#18348 = ORIENTED_EDGE ( 'NONE', *, *, #10776, .F. ) ;
#18349 = CARTESIAN_POINT ( 'NONE',  ( -30.86467312755451076, -0.1056312804566766766, -6.415435717435306273 ) ) ;
#18350 = ORIENTED_EDGE ( 'NONE', *, *, #14599, .F. ) ;
#18351 = CARTESIAN_POINT ( 'NONE',  ( 24.87279611354669484, -0.2351948277588876701, -18.36342014254012156 ) ) ;
#18352 = CARTESIAN_POINT ( 'NONE',  ( 3.503793317224329851, 8.420815634768676006, 7.000000000000000000 ) ) ;
#18353 = CARTESIAN_POINT ( 'NONE',  ( 24.79887074938343616, -23.91042127310592846, 18.42518152272109688 ) ) ;
#18354 = ORIENTED_EDGE ( 'NONE', *, *, #12543, .F. ) ;
#18355 = AXIS2_PLACEMENT_3D ( 'NONE', #2659, #15046, #27437 ) ;
#18356 = CARTESIAN_POINT ( 'NONE',  ( -27.15297274608521505, 3.518273904157881660, -8.818013410083365144 ) ) ;
#18357 = ADVANCED_FACE ( 'NONE', ( #28674 ), #7133, .F. ) ;
#18358 = CARTESIAN_POINT ( 'NONE',  ( -11.94134295108998245, 16.18301270189233065, 10.00000000000000000 ) ) ;
#18359 = EDGE_CURVE ( 'NONE', #25420, #32345, #37819, .T. ) ;
#18360 = FACE_OUTER_BOUND ( 'NONE', #16476, .T. ) ;
#18361 = CARTESIAN_POINT ( 'NONE',  ( -35.16163374036107570, -2.327860755070493060, 10.99999999999982414 ) ) ;
#18362 = DIRECTION ( 'NONE',  ( 1.000000000000000000, 0.000000000000000000, 0.000000000000000000 ) ) ;
#18363 = CIRCLE ( 'NONE', #32075, 0.9999999999999985567 ) ;
#18364 = FACE_BOUND ( 'NONE', #24470, .T. ) ;
#18365 = CONICAL_SURFACE ( 'NONE', #22233, 1.000000000000004441, 0.7853981633974524978 ) ;
#18366 = CARTESIAN_POINT ( 'NONE',  ( 23.13582672293635056, 13.35747578641157851, 12.14047268033097460 ) ) ;
#18367 = VERTEX_POINT ( 'NONE', #19531 ) ;
#18368 = CARTESIAN_POINT ( 'NONE',  ( -19.48816862725384169, 6.402609444000542993, -30.00000000000000355 ) ) ;
#18369 = DIRECTION ( 'NONE',  ( -0.6691306063588569053, 0.7431448254773954654, 0.000000000000000000 ) ) ;
#18370 = FACE_BOUND ( 'NONE', #35596, .T. ) ;
#18371 = CARTESIAN_POINT ( 'NONE',  ( 14.60836822939834434, -16.15617325942540106, -24.48969730763191066 ) ) ;
#18372 = CARTESIAN_POINT ( 'NONE',  ( 14.25384497784216009, 25.55416164399396806, 7.000000000000000000 ) ) ;
#18373 = EDGE_CURVE ( 'NONE', #24416, #16847, #2525, .T. ) ;
#18374 = CARTESIAN_POINT ( 'NONE',  ( 13.34594308816744324, 23.10805189355821554, -15.41729477589293928 ) ) ;
#18375 = AXIS2_PLACEMENT_3D ( 'NONE', #35359, #35964, #7721 ) ;
#18376 = VERTEX_POINT ( 'NONE', #25621 ) ;
#18377 = CARTESIAN_POINT ( 'NONE',  ( -16.15419993190558401, 23.97630781949517598, -6.895672015151252054 ) ) ;
#18378 = CARTESIAN_POINT ( 'NONE',  ( -26.92296394334159260, -7.646625634049264875, 20.69868183039781329 ) ) ;
#18379 = EDGE_CURVE ( 'NONE', #12836, #38979, #6926, .T. ) ;
#18380 = CIRCLE ( 'NONE', #23571, 17.00000000000000000 ) ;
#18381 = LINE ( 'NONE', #27911, #27597 ) ;
#18382 = CARTESIAN_POINT ( 'NONE',  ( 11.00415319253780488, 17.29620292487934563, -29.34878042274528198 ) ) ;
#18383 = VERTEX_POINT ( 'NONE', #38020 ) ;
#18384 = LINE ( 'NONE', #30967, #30707 ) ;
#18385 = EDGE_LOOP ( 'NONE', ( #18701, #39986, #30889, #15809 ) ) ;
#18387 = CARTESIAN_POINT ( 'NONE',  ( 15.82937963299585071, 7.760892663579005202, 10.00000000000000000 ) ) ;
#18386 = CARTESIAN_POINT ( 'NONE',  ( -15.33616239741719234, 27.06134930142311745, -5.472843250504300094 ) ) ;
#18388 = CARTESIAN_POINT ( 'NONE',  ( -9.670677759005913643, -18.31648422485758232, -27.44423000158573700 ) ) ;
#18389 = CARTESIAN_POINT ( 'NONE',  ( 9.189613563248487438, 10.70223284378001516, 10.76099332938164288 ) ) ;
#18390 = AXIS2_PLACEMENT_3D ( 'NONE', #2135, #26912, #26310 ) ;
#18391 = CARTESIAN_POINT ( 'NONE',  ( -19.55581111739057931, -11.80372462897835817, -22.98306217881111380 ) ) ;
#18392 = CARTESIAN_POINT ( 'NONE',  ( -13.18739005314428248, -25.19688251061680617, -10.68449307879287780 ) ) ;
#18393 = DIRECTION ( 'NONE',  ( -0.8090169943749430104, 0.5877852522924791323, 0.000000000000000000 ) ) ;
#18394 = CARTESIAN_POINT ( 'NONE',  ( 16.02269691061813006, 23.35602331712748025, -8.798133084021126038 ) ) ;
#18395 = ORIENTED_EDGE ( 'NONE', *, *, #16849, .F. ) ;
#18396 = CARTESIAN_POINT ( 'NONE',  ( 24.81717070478679688, 5.495116086519474585, -11.78307908032107854 ) ) ;
#18397 = FACE_OUTER_BOUND ( 'NONE', #36826, .T. ) ;
#18398 = LINE ( 'NONE', #27731, #4336 ) ;
#18399 = LINE ( 'NONE', #30597, #36206 ) ;
#18400 = VERTEX_POINT ( 'NONE', #16695 ) ;
#18401 = CARTESIAN_POINT ( 'NONE',  ( -31.94197113782983877, -1.240068278442397531, -5.930863948769548699 ) ) ;
#18402 = CIRCLE ( 'NONE', #33964, 1.000000000000006883 ) ;
#18403 = CARTESIAN_POINT ( 'NONE',  ( 30.24433606442397959, -0.05178948828996779441, -8.764081122583004202 ) ) ;
#18404 = DIRECTION ( 'NONE',  ( -0.9135454576425986462, 0.4067366430758054263, 0.000000000000000000 ) ) ;
#18405 = VECTOR ( 'NONE', #21847, 1000.000000000000000 ) ;
#18406 = CARTESIAN_POINT ( 'NONE',  ( 23.00727501322602819, -19.64144336131528590, 20.50957957746028626 ) ) ;
#18407 = EDGE_LOOP ( 'NONE', ( #38172, #33584, #18854, #19033, #8621, #14249 ) ) ;
#18408 = FACE_OUTER_BOUND ( 'NONE', #3251, .T. ) ;
#18409 = DIRECTION ( 'NONE',  ( 0.000000000000000000, 0.000000000000000000, 1.000000000000000000 ) ) ;
#18410 = COLOUR_RGB ( '', 0.40784314, 0.44705882, 0.49803922) ;
#18411 = EDGE_LOOP ( 'NONE', ( #4490, #34040, #1982, #7342 ) ) ;
#18412 = EDGE_CURVE ( 'NONE', #23249, #4180, #4090, .T. ) ;
#18413 = DIRECTION ( 'NONE',  ( -0.6691306063588570163, 0.7431448254773952433, 0.000000000000000000 ) ) ;
#18414 = CIRCLE ( 'NONE', #22955, 1.000000000000000888 ) ;
#18415 = DIRECTION ( 'NONE',  ( 0.000000000000000000, 0.000000000000000000, 1.000000000000000000 ) ) ;
#18416 = CARTESIAN_POINT ( 'NONE',  ( 13.94482798346721175, 26.50521816028912525, 11.00000000000000000 ) ) ;
#18417 = CARTESIAN_POINT ( 'NONE',  ( 1.910055380441378681, 26.73820970956909449, -18.62404870119007327 ) ) ;
#18418 = DIRECTION ( 'NONE',  ( 0.5821182788257885932, 0.000000000000000000, -0.8131041196900317125 ) ) ;
#18419 = CARTESIAN_POINT ( 'NONE',  ( 14.55573640795740076, 20.46737631633098431, 10.96580508970281542 ) ) ;
#18420 = PLANE ( 'NONE',  #24584 ) ;
#18421 = CARTESIAN_POINT ( 'NONE',  ( -12.19134295108997712, 16.61602540378455117, 10.00000000000000000 ) ) ;
#18422 = CARTESIAN_POINT ( 'NONE',  ( 11.59687233693865593, 32.01413362675371133, 7.485699520496978288 ) ) ;
#18423 = CARTESIAN_POINT ( 'NONE',  ( -12.28720923544494248, -14.55658080566520418, 23.00000000000000000 ) ) ;
#18424 = CARTESIAN_POINT ( 'NONE',  ( 14.30852138182742728, 26.56022758966166109, -10.58015527044261894 ) ) ;
#18425 = DIRECTION ( 'NONE',  ( 0.000000000000000000, 0.000000000000000000, 1.000000000000000000 ) ) ;
#18426 = VERTEX_POINT ( 'NONE', #28878 ) ;
#18428 = FACE_OUTER_BOUND ( 'NONE', #17306, .T. ) ;
#18427 = CARTESIAN_POINT ( 'NONE',  ( -17.91835549149922713, 18.20411370326764811, -9.837959905343433675 ) ) ;
#18429 = AXIS2_PLACEMENT_3D ( 'NONE', #26506, #4567, #26703 ) ;
#18430 = CARTESIAN_POINT ( 'NONE',  ( 13.24038105676659960, 15.43301270189224716, 10.59344459855565468 ) ) ;
#18431 = CARTESIAN_POINT ( 'NONE',  ( 11.90604067169677904, -21.48480776871750209, -18.45226974073501580 ) ) ;
#18432 = CARTESIAN_POINT ( 'NONE',  ( -16.57032929827895273, -22.18377021195244936, -16.08031649169519994 ) ) ;
#18433 = CARTESIAN_POINT ( 'NONE',  ( 15.01833821314311379, 25.96818848446423189, -9.238322678839528734 ) ) ;
#18434 = CARTESIAN_POINT ( 'NONE',  ( 14.83401637327768618, 25.62822920609098176, -10.17906930079575112 ) ) ;
#18435 = B_SPLINE_SURFACE_WITH_KNOTS ( 'NONE', 1, 3, ( 
 ( #39558, #18430, #30821, #25501, #27961, #31806, #37309, #25311, #28161, #3772 ),
 ( #24915, #13310, #34658, #37901, #733, #16371, #3377, #3971, #19019, #15574 ) ),
 .UNSPECIFIED., .F., .F., .F.,
 ( 2, 2 ),
 ( 4, 2, 2, 2, 4 ),
 ( 0.000000000000000000, 1.000000000000000000 ),
 ( 1.183199640139713571, 1.575898721838439265, 1.968597803537164737, 2.361296885235890208, 2.753995966934615680 ),
 .UNSPECIFIED. ) ;
#18436 = ORIENTED_EDGE ( 'NONE', *, *, #1768, .T. ) ;
#18437 = CYLINDRICAL_SURFACE ( 'NONE', #39318, 1.000000000000000000 ) ;
#18438 = CARTESIAN_POINT ( 'NONE',  ( -9.450798935534860945, -18.19154675410751310, -30.00000000000000000 ) ) ;
#18439 = CARTESIAN_POINT ( 'NONE',  ( -36.66879582113860181, -12.81605961718980602, 14.53008259253997636 ) ) ;
#18440 = PRESENTATION_LAYER_ASSIGNMENT (  '', '', ( #8047 ) ) ;
#18441 = CARTESIAN_POINT ( 'NONE',  ( -28.36389015409294601, -22.24485741755683677, -9.748513342677570748 ) ) ;
#18442 = CARTESIAN_POINT ( 'NONE',  ( 1.575182151896790339, -22.97049887755249031, -15.95023905627559024 ) ) ;
#18443 = CARTESIAN_POINT ( 'NONE',  ( 11.31999918839495933, 17.23783125480536782, -28.09381573830394174 ) ) ;
#18444 = CARTESIAN_POINT ( 'NONE',  ( 21.17511726572084285, 11.79403841473552461, -10.38720750812251481 ) ) ;
#18445 = CYLINDRICAL_SURFACE ( 'NONE', #32921, 16.99999999999999645 ) ;
#18446 = ADVANCED_FACE ( 'NONE', ( #29079 ), #29284, .F. ) ;
#18447 = CARTESIAN_POINT ( 'NONE',  ( -5.177819697455928072, 36.33475957580800042, -8.863124948621987187 ) ) ;
#18448 = ORIENTED_EDGE ( 'NONE', *, *, #16104, .T. ) ;
#18449 = CARTESIAN_POINT ( 'NONE',  ( -25.16898798258920777, -3.892907297832375324, -19.00733652691929265 ) ) ;
#18450 = CARTESIAN_POINT ( 'NONE',  ( -16.81416712651596868, 27.17354907308742185, 13.92931973827808712 ) ) ;
#18451 = VERTEX_POINT ( 'NONE', #37629 ) ;
#18452 = CARTESIAN_POINT ( 'NONE',  ( 4.727507481117214638, 31.88885898370941874, 11.00000000000000000 ) ) ;
#18453 = CARTESIAN_POINT ( 'NONE',  ( 19.30289106310104685, -16.27633469853321557, 23.00000000000000000 ) ) ;
#18454 = CARTESIAN_POINT ( 'NONE',  ( -24.28611727277358412, 1.006298860692754316, -18.51342557011203738 ) ) ;
#18455 = CARTESIAN_POINT ( 'NONE',  ( 34.22374188224875979, -12.56921889987730800, -8.873390837788807772 ) ) ;
#18456 = AXIS2_PLACEMENT_3D ( 'NONE', #3620, #21902, #16015 ) ;
#18457 = ADVANCED_FACE ( 'NONE', ( #28475 ), #1053, .F. ) ;
#18458 = ORIENTED_EDGE ( 'NONE', *, *, #10706, .T. ) ;
#18459 = DIRECTION ( 'NONE',  ( 0.2079116908177663647, 0.9781476007338042455, 0.000000000000000000 ) ) ;
#18460 = ORIENTED_EDGE ( 'NONE', *, *, #11360, .T. ) ;
#18461 = PLANE ( 'NONE',  #10613 ) ;
#18462 = CYLINDRICAL_SURFACE ( 'NONE', #12357, 17.99999999999992895 ) ;
#18463 = AXIS2_PLACEMENT_3D ( 'NONE', #9335, #6275, #14554 ) ;
#18464 = CARTESIAN_POINT ( 'NONE',  ( -7.611215932167763043, 18.68301270189229513, 7.000000000000000000 ) ) ;
#18465 = ORIENTED_EDGE ( 'NONE', *, *, #30713, .T. ) ;
#18466 = EDGE_CURVE ( 'NONE', #27796, #34177, #4295, .T. ) ;
#18467 = CARTESIAN_POINT ( 'NONE',  ( -1.624100677291492101, 20.43571491435562493, -29.21538960015010034 ) ) ;
#18468 = CARTESIAN_POINT ( 'NONE',  ( -5.494150297853999554, 36.06936027812446355, 11.00000000000000355 ) ) ;
#18469 = PLANE ( 'NONE',  #10471 ) ;
#18470 = EDGE_CURVE ( 'NONE', #10226, #11532, #25103, .T. ) ;
#18471 = LINE ( 'NONE', #12167, #38356 ) ;
#18472 = CARTESIAN_POINT ( 'NONE',  ( 28.65116837111353476, -23.44305233603574123, -7.996273562022556902 ) ) ;
#18473 = CARTESIAN_POINT ( 'NONE',  ( 16.00867692525036290, 13.39373376902821278, -25.45607993003914871 ) ) ;
#18474 = CARTESIAN_POINT ( 'NONE',  ( 8.790171551589970989, 18.84476076792456567, -27.27665836229843777 ) ) ;
#18475 = VECTOR ( 'NONE', #10457, 1000.000000000000000 ) ;
#18476 = EDGE_LOOP ( 'NONE', ( #23017, #39677, #11351, #12623 ) ) ;
#18477 = CARTESIAN_POINT ( 'NONE',  ( -21.15630055661832287, 12.66096790527163485, -7.428688768124617425 ) ) ;
#18478 = CARTESIAN_POINT ( 'NONE',  ( -0.5415361484146629101, 27.50000000000004974, 23.00000000000000000 ) ) ;
#18479 = CARTESIAN_POINT ( 'NONE',  ( 12.75462202092051101, -22.56042021202167547, -16.43275011361073368 ) ) ;
#18480 = CARTESIAN_POINT ( 'NONE',  ( 10.44103466624280507, 32.57396620494213124, 11.00000000000000000 ) ) ;
#18481 = CARTESIAN_POINT ( 'NONE',  ( 1.354211015180573125E-14, -26.63027081345975589, -13.39439507595156265 ) ) ;
#18482 = CARTESIAN_POINT ( 'NONE',  ( -14.92500765838162735, 25.83139737525633706, -9.707172920663500904 ) ) ;
#18483 = CARTESIAN_POINT ( 'NONE',  ( -16.46163937660932675, -19.62796718106372751, -18.96315420958638143 ) ) ;
#18484 = CARTESIAN_POINT ( 'NONE',  ( 13.11109743797562466, -26.17839091903269733, -5.474232844414386179 ) ) ;
#18485 = EDGE_CURVE ( 'NONE', #14611, #15571, #3890, .T. ) ;
#18486 = EDGE_CURVE ( 'NONE', #12690, #4300, #21340, .T. ) ;
#18487 = DIRECTION ( 'NONE',  ( 0.000000000000000000, 0.000000000000000000, 1.000000000000000000 ) ) ;
#18488 = ADVANCED_FACE ( 'NONE', ( #5300 ), #29881, .T. ) ;
#18489 = VERTEX_POINT ( 'NONE', #11201 ) ;
#18490 = CARTESIAN_POINT ( 'NONE',  ( -9.875490294415444126, 29.82293549085830264, -13.06707053424541520 ) ) ;
#18491 = CARTESIAN_POINT ( 'NONE',  ( 1.000000000000000444, 37.04625217320466390, 10.49999999999999822 ) ) ;
#18492 = CYLINDRICAL_SURFACE ( 'NONE', #2960, 1.000000000000000000 ) ;
#18493 = AXIS2_PLACEMENT_3D ( 'NONE', #16836, #23117, #35516 ) ;
#18494 = CARTESIAN_POINT ( 'NONE',  ( 9.303655249773111535, 10.73386218874820663, 7.500000000000000888 ) ) ;
#18495 = ORIENTED_EDGE ( 'NONE', *, *, #21059, .T. ) ;
#18496 = CARTESIAN_POINT ( 'NONE',  ( 29.35229056070877718, 0.07664280817823312941, -10.65354559736987383 ) ) ;
#18497 = CARTESIAN_POINT ( 'NONE',  ( -6.749995343096113487, 37.10960504752362255, -4.999999999999997335 ) ) ;
#18498 = DIRECTION ( 'NONE',  ( -0.1045284632676569819, -0.9945218953682730678, 0.000000000000000000 ) ) ;
#18499 = VERTEX_POINT ( 'NONE', #7743 ) ;
#18500 = AXIS2_PLACEMENT_3D ( 'NONE', #32624, #32419, #29356 ) ;
#18501 = CARTESIAN_POINT ( 'NONE',  ( -23.91902260382858714, 0.5374607429489602906, -19.50238920718228641 ) ) ;
#18502 = DIRECTION ( 'NONE',  ( -0.000000000000000000, -0.000000000000000000, -1.000000000000000000 ) ) ;
#18503 = ORIENTED_EDGE ( 'NONE', *, *, #13854, .T. ) ;
#18504 = CARTESIAN_POINT ( 'NONE',  ( 22.03414195915153684, -3.843093978875791628, -23.35154269917405756 ) ) ;
#18505 = CIRCLE ( 'NONE', #19802, 1.000000000000000000 ) ;
#18506 = ORIENTED_EDGE ( 'NONE', *, *, #32339, .T. ) ;
#18507 = CARTESIAN_POINT ( 'NONE',  ( 1.911335737650396993, 40.16401087634233846, 13.32518128616608877 ) ) ;
#18508 = CARTESIAN_POINT ( 'NONE',  ( -6.143904198944369455, -13.77689918168226235, 20.99999999999999645 ) ) ;
#18509 = CARTESIAN_POINT ( 'NONE',  ( -14.98890121934603314, -28.67928442654204346, 2.999999999999999112 ) ) ;
#18510 = EDGE_CURVE ( 'NONE', #2072, #8671, #2063, .T. ) ;
#18511 = CARTESIAN_POINT ( 'NONE',  ( 9.267781094589551572, 26.19038745656764533, 20.25080042701674543 ) ) ;
#18512 = LINE ( 'NONE', #22145, #21368 ) ;
#18513 = ORIENTED_EDGE ( 'NONE', *, *, #3692, .T. ) ;
#18514 = LINE ( 'NONE', #25203, #7311 ) ;
#18515 = DIRECTION ( 'NONE',  ( 1.000000000000000000, 0.000000000000000000, 0.000000000000000000 ) ) ;
#18516 = CARTESIAN_POINT ( 'NONE',  ( -6.854454053420242943, 35.54304081427989814, 7.500000000000000888 ) ) ;
#18517 = CARTESIAN_POINT ( 'NONE',  ( -12.30736835487442704, 14.81698729810789672, 7.000000000000000000 ) ) ;
#18518 = AXIS2_PLACEMENT_3D ( 'NONE', #2057, #14432, #2455 ) ;
#18519 = CARTESIAN_POINT ( 'NONE',  ( 7.047533809553444328, 27.34333616107158349, -16.78122118766336257 ) ) ;
#18520 = CARTESIAN_POINT ( 'NONE',  ( 13.39463915635820790, 18.33192650902018883, 12.00000000000000000 ) ) ;
#18521 = CARTESIAN_POINT ( 'NONE',  ( 18.05419321018431589, -26.43384140100978641, -9.107442122467894308 ) ) ;
#18522 = DIRECTION ( 'NONE',  ( 1.000000000000000000, 0.000000000000000000, 0.000000000000000000 ) ) ;
#18523 = VECTOR ( 'NONE', #28358, 1000.000000000000000 ) ;
#18524 = CARTESIAN_POINT ( 'NONE',  ( 3.813962023474613439, 32.29559562678520024, 10.50000000000000000 ) ) ;
#18525 = DIRECTION ( 'NONE',  ( -0.6691306063588670083, -0.7431448254773863615, 0.000000000000000000 ) ) ;
#18526 = ORIENTED_EDGE ( 'NONE', *, *, #12404, .T. ) ;
#18527 = CARTESIAN_POINT ( 'NONE',  ( -15.43019833371434579, 26.73233873233005653, -5.000000000000002665 ) ) ;
#18528 = AXIS2_PLACEMENT_3D ( 'NONE', #15839, #24979, #28224 ) ;
#18529 = CARTESIAN_POINT ( 'NONE',  ( -28.97703757779445866, -22.02226062111172311, 17.92354375535250810 ) ) ;
#18530 = CARTESIAN_POINT ( 'NONE',  ( 14.95787899955085543, -26.32395102021559197, -7.829361611777857277 ) ) ;
#18531 = CARTESIAN_POINT ( 'NONE',  ( -4.006135375494391582, 8.432903524120151317, 10.49999999999999822 ) ) ;
#18532 = EDGE_CURVE ( 'NONE', #28430, #6642, #11404, .T. ) ;
#18533 = ORIENTED_EDGE ( 'NONE', *, *, #5935, .F. ) ;
#18534 = VERTEX_POINT ( 'NONE', #35988 ) ;
#18535 = CARTESIAN_POINT ( 'NONE',  ( -12.50895407495804434, 23.45396610927918957, -16.29466274982731733 ) ) ;
#18536 = CARTESIAN_POINT ( 'NONE',  ( -20.24725042846177203, -26.82317351284016027, -7.696457707553546967 ) ) ;
#18537 = FACE_BOUND ( 'NONE', #23825, .T. ) ;
#18538 = ADVANCED_FACE ( 'NONE', ( #14040 ), #8353, .T. ) ;
#18539 = ORIENTED_EDGE ( 'NONE', *, *, #3467, .T. ) ;
#18540 = CARTESIAN_POINT ( 'NONE',  ( -19.78566680745120365, -6.173659883245491642, -27.77246204399593665 ) ) ;
#18541 = CARTESIAN_POINT ( 'NONE',  ( -10.62033910827488725, -20.04172040370476537, -21.64366540849149700 ) ) ;
#18542 = DIRECTION ( 'NONE',  ( 0.000000000000000000, 0.000000000000000000, 1.000000000000000000 ) ) ;
#18543 = ORIENTED_EDGE ( 'NONE', *, *, #37588, .F. ) ;
#18544 = CARTESIAN_POINT ( 'NONE',  ( 23.24001508372326441, 0.7665741418457661105, -20.56782922800247704 ) ) ;
#18545 = CARTESIAN_POINT ( 'NONE',  ( -14.26585111513660031, 17.86474508437623143, 13.00000000000000178 ) ) ;
#18546 = CARTESIAN_POINT ( 'NONE',  ( -13.37378135583788286, 20.59160479820267398, 9.500000000000000000 ) ) ;
#18547 = ORIENTED_EDGE ( 'NONE', *, *, #39557, .F. ) ;
#18548 = CARTESIAN_POINT ( 'NONE',  ( -28.37955323983597467, 0.09052745480185327154, -12.54540266281936844 ) ) ;
#18549 = ORIENTED_EDGE ( 'NONE', *, *, #27283, .T. ) ;
#18550 = CARTESIAN_POINT ( 'NONE',  ( 21.89958531435420497, -0.4341651203043321861, -23.71319811986195703 ) ) ;
#18551 = CARTESIAN_POINT ( 'NONE',  ( -0.2953921336507466799, -20.50164038595707439, -29.99999999999999645 ) ) ;
#18552 = CARTESIAN_POINT ( 'NONE',  ( 26.47427689499786041, -23.88731992525525172, 17.92354375535211730 ) ) ;
#18553 = ORIENTED_EDGE ( 'NONE', *, *, #37229, .F. ) ;
#18554 = CARTESIAN_POINT ( 'NONE',  ( -27.86048499494648567, 2.636343818125510108, -8.804713555145298187 ) ) ;
#18555 = VECTOR ( 'NONE', #7320, 1000.000000000000000 ) ;
#18556 = CARTESIAN_POINT ( 'NONE',  ( -10.24926262130046695, 33.45294210977303351, 7.102474990965862212 ) ) ;
#18557 = EDGE_CURVE ( 'NONE', #32632, #11714, #1659, .T. ) ;
#18558 = LINE ( 'NONE', #3309, #21289 ) ;
#18559 = VECTOR ( 'NONE', #10935, 1000.000000000000000 ) ;
#18560 = CIRCLE ( 'NONE', #38007, 6.000000000000003553 ) ;
#18561 = DIRECTION ( 'NONE',  ( -0.000000000000000000, -0.000000000000000000, -1.000000000000000000 ) ) ;
#18562 = EDGE_CURVE ( 'NONE', #37305, #35978, #31054, .T. ) ;
#18563 = AXIS2_PLACEMENT_3D ( 'NONE', #37756, #986, #34313 ) ;
#18564 = DIRECTION ( 'NONE',  ( 0.000000000000000000, 0.000000000000000000, 1.000000000000000000 ) ) ;
#18565 = EDGE_CURVE ( 'NONE', #13010, #18932, #19351, .T. ) ;
#18566 = DIRECTION ( 'NONE',  ( 1.000000000000000000, 0.000000000000000000, 0.000000000000000000 ) ) ;
#18567 = CARTESIAN_POINT ( 'NONE',  ( 31.94006737154954934, 0.9747213384812106751, 13.92931973827808712 ) ) ;
#18568 = CARTESIAN_POINT ( 'NONE',  ( -24.63660806518388924, 7.092056224046558555, -7.894412173378091424 ) ) ;
#18569 = DIRECTION ( 'NONE',  ( 0.000000000000000000, 0.000000000000000000, 1.000000000000000000 ) ) ;
#18570 = LINE ( 'NONE', #13413, #1295 ) ;
#18571 = CARTESIAN_POINT ( 'NONE',  ( 16.18034479685473670, -16.82698281147069252, -22.08061376403061971 ) ) ;
#18572 = LINE ( 'NONE', #280, #15088 ) ;
#18573 = CARTESIAN_POINT ( 'NONE',  ( 11.31663199219571148, 18.58087735513076666, -23.82738904643892397 ) ) ;
#18574 = ORIENTED_EDGE ( 'NONE', *, *, #17182, .F. ) ;
#18575 = CARTESIAN_POINT ( 'NONE',  ( -15.87128850075231590, 24.35504432729732471, -7.840557014529688118 ) ) ;
#18576 = CARTESIAN_POINT ( 'NONE',  ( -18.16616693041741470, -20.30807083247755784, 20.50957957746031823 ) ) ;
#18577 = LINE ( 'NONE', #3329, #36688 ) ;
#18578 = CARTESIAN_POINT ( 'NONE',  ( 11.02183263331336072, 17.28494426090127334, -29.34916159435818273 ) ) ;
#18579 = ORIENTED_EDGE ( 'NONE', *, *, #2912, .T. ) ;
#18580 = DIRECTION ( 'NONE',  ( -0.5877852522924691403, 0.8090169943749505599, -0.000000000000000000 ) ) ;
#18581 = ADVANCED_FACE ( 'NONE', ( #1865 ), #30086, .T. ) ;
#18582 = EDGE_LOOP ( 'NONE', ( #32675, #19171, #4907, #18144, #10860 ) ) ;
#18583 = AXIS2_PLACEMENT_3D ( 'NONE', #7731, #39213, #29671 ) ;
#18585 = CARTESIAN_POINT ( 'NONE',  ( 24.21836086243564523, 15.77821876070162332, 9.500000000000000000 ) ) ;
#18584 = CARTESIAN_POINT ( 'NONE',  ( -10.95724656110390960, 17.57990422145660503, -27.43878361132108878 ) ) ;
#18586 = ADVANCED_FACE ( 'NONE', ( #33147 ), #26633, .T. ) ;
#18587 = CARTESIAN_POINT ( 'NONE',  ( -14.18625507368043159, -24.63497049750179357, -12.53935437351460003 ) ) ;
#18588 = CARTESIAN_POINT ( 'NONE',  ( -1.981967702234832984, 30.37627742347970283, 13.00000000000000178 ) ) ;
#18589 = EDGE_CURVE ( 'NONE', #26936, #14625, #40123, .T. ) ;
#18590 = CIRCLE ( 'NONE', #23771, 1.000000000000000444 ) ;
#18591 = EDGE_LOOP ( 'NONE', ( #7465, #5549, #3354, #8386 ) ) ;
#18592 = CARTESIAN_POINT ( 'NONE',  ( -18.66148164344931004, -9.085586588243005579, -27.71109438505605738 ) ) ;
#18593 = CARTESIAN_POINT ( 'NONE',  ( -10.80975121954417695, -21.57342429178983068, -18.55613864020834214 ) ) ;
#18594 = DIRECTION ( 'NONE',  ( 0.8090169943749426773, -0.5877852522924796874, 0.000000000000000000 ) ) ;
#18595 = CARTESIAN_POINT ( 'NONE',  ( 15.94824334694384582, 24.12454408679510820, -7.842198151814580243 ) ) ;
#18596 = ORIENTED_EDGE ( 'NONE', *, *, #29980, .F. ) ;
#18597 = CARTESIAN_POINT ( 'NONE',  ( 26.43854853772318947, 4.666896068008411724, -7.871277590448321426 ) ) ;
#18598 = VECTOR ( 'NONE', #28117, 999.9999999999998863 ) ;
#18599 = CARTESIAN_POINT ( 'NONE',  ( -7.688306800005769048, 28.52217545723006609, 6.000000000000000000 ) ) ;
#18600 = CARTESIAN_POINT ( 'NONE',  ( 14.86556419889026515, 20.43481210330100595, 10.50000000000000000 ) ) ;
#18601 = CARTESIAN_POINT ( 'NONE',  ( -17.08966005440910507, -22.85233455234303079, -15.10154554898533874 ) ) ;
#18602 = ORIENTED_EDGE ( 'NONE', *, *, #26513, .T. ) ;
#18603 = CARTESIAN_POINT ( 'NONE',  ( -31.18229473435558319, -0.3319675162687183989, -4.999999999999999112 ) ) ;
#18604 = CARTESIAN_POINT ( 'NONE',  ( 30.03507885031549662, -0.2128173951707619527, -9.691532691046774062 ) ) ;
#18605 = DIRECTION ( 'NONE',  ( 0.000000000000000000, 0.000000000000000000, -1.000000000000000000 ) ) ;
#18606 = CARTESIAN_POINT ( 'NONE',  ( 28.63766977552451465, -11.08150102882311216, 20.50957957746029336 ) ) ;
#18607 = EDGE_LOOP ( 'NONE', ( #33178, #180, #39252, #16871 ) ) ;
#18608 = CARTESIAN_POINT ( 'NONE',  ( 22.52744239175980567, -0.1803094636422790109, -30.00000000000000000 ) ) ;
#18609 = ADVANCED_FACE ( 'NONE', ( #26431 ), #26230, .T. ) ;
#18610 = CARTESIAN_POINT ( 'NONE',  ( -7.468455364333135726, 29.89744377950679777, 11.00000000000000000 ) ) ;
#18611 = ADVANCED_FACE ( 'NONE', ( #5102 ), #4701, .F. ) ;
#18612 = ORIENTED_EDGE ( 'NONE', *, *, #2643, .F. ) ;
#18613 = DIRECTION ( 'NONE',  ( -0.000000000000000000, -0.000000000000000000, -1.000000000000000000 ) ) ;
#18614 = AXIS2_PLACEMENT_3D ( 'NONE', #30395, #14948, #33651 ) ;
#18615 = VECTOR ( 'NONE', #4843, 1000.000000000000000 ) ;
#18616 = DIRECTION ( 'NONE',  ( 0.9135454576426006446, -0.4067366430758009299, 0.000000000000000000 ) ) ;
#18617 = CARTESIAN_POINT ( 'NONE',  ( -1.590043107810771073, 12.61456814725308995, 10.50000000000000000 ) ) ;
#18618 = CARTESIAN_POINT ( 'NONE',  ( 2.734349871686851507, 38.15652731944587828, -6.277973080134718664 ) ) ;
#18619 = DIRECTION ( 'NONE',  ( -0.000000000000000000, -0.000000000000000000, 1.000000000000000000 ) ) ;
#18620 = DIRECTION ( 'NONE',  ( -0.9135454576426004225, 0.4067366430758009854, 0.000000000000000000 ) ) ;
#18621 = CARTESIAN_POINT ( 'NONE',  ( 13.30736835487433467, 16.54903810567660472, 7.000000000000000000 ) ) ;
#18622 = DIRECTION ( 'NONE',  ( -0.7071067811865504593, 0.000000000000000000, -0.7071067811865445751 ) ) ;
#18623 = CARTESIAN_POINT ( 'NONE',  ( 12.03571151536236528, 31.45218678977230908, 7.000000000000000000 ) ) ;
#18624 = DIRECTION ( 'NONE',  ( 1.000000000000000000, 0.000000000000000000, 0.000000000000000000 ) ) ;
#18625 = CARTESIAN_POINT ( 'NONE',  ( 13.28887463864177043, 24.39605242036939714, -14.37461945989296552 ) ) ;
#18626 = FACE_OUTER_BOUND ( 'NONE', #22167, .T. ) ;
#18627 = ORIENTED_EDGE ( 'NONE', *, *, #28252, .F. ) ;
#18629 = CARTESIAN_POINT ( 'NONE',  ( 12.22403502154099542, 14.67264973081032053, 10.83333333333333037 ) ) ;
#18628 = CARTESIAN_POINT ( 'NONE',  ( -16.90813000154546231, 15.39385669201410423, -17.92356762543468562 ) ) ;
#18630 = DIRECTION ( 'NONE',  ( 0.000000000000000000, 0.000000000000000000, 1.000000000000000000 ) ) ;
#18631 = CARTESIAN_POINT ( 'NONE',  ( 15.23417145244625281, -26.39024772874911307, -7.827869052557821838 ) ) ;
#18632 = CARTESIAN_POINT ( 'NONE',  ( -12.63282099796252034, -16.15870876741617579, -30.00000000000001066 ) ) ;
#18633 = DIRECTION ( 'NONE',  ( 0.000000000000000000, 0.000000000000000000, 1.000000000000000000 ) ) ;
#18634 = CARTESIAN_POINT ( 'NONE',  ( 11.05947062229327926, 17.51160466381875835, -27.44674441618432326 ) ) ;
#18635 = ORIENTED_EDGE ( 'NONE', *, *, #37534, .F. ) ;
#18636 = CARTESIAN_POINT ( 'NONE',  ( -9.559512017365660697, 19.71884705062586107, 12.00000000000000000 ) ) ;
#18637 = CARTESIAN_POINT ( 'NONE',  ( -14.75295324041043799, -25.80753188146049482, -9.710811175497244818 ) ) ;
#18638 = CARTESIAN_POINT ( 'NONE',  ( -36.20842572154693073, -9.127542156328868117, 15.13084544680213384 ) ) ;
#18639 = CARTESIAN_POINT ( 'NONE',  ( -18.13230426550196839, -12.48663698560311275, -24.23425696877543700 ) ) ;
#18640 = CARTESIAN_POINT ( 'NONE',  ( -0.2861739033633732832, -21.20374024808155156, -23.33089809976452500 ) ) ;
#18641 = CARTESIAN_POINT ( 'NONE',  ( 14.23250866199382436, 23.46649709690858643, -13.53614068862031061 ) ) ;
#18642 = CARTESIAN_POINT ( 'NONE',  ( 22.42968607831754113, 10.03218932006194386, -9.389054437147178689 ) ) ;
#18643 = DIRECTION ( 'NONE',  ( -0.000000000000000000, -0.000000000000000000, -1.000000000000000000 ) ) ;
#18644 = CARTESIAN_POINT ( 'NONE',  ( -3.836448945760380536, 22.38753517863213816, -23.07412469210595773 ) ) ;
#18645 = VERTEX_POINT ( 'NONE', #38828 ) ;
#18646 = CARTESIAN_POINT ( 'NONE',  ( -27.06678414647392117, -5.014901417910227366, -16.91862960005362382 ) ) ;
#18647 = AXIS2_PLACEMENT_3D ( 'NONE', #24882, #37277, #9451 ) ;
#18648 = CIRCLE ( 'NONE', #483, 6.000000000000008882 ) ;
#18649 = CARTESIAN_POINT ( 'NONE',  ( -16.37862447372143038, 21.59537890665771798, 16.87380292611990384 ) ) ;
#18650 = ORIENTED_EDGE ( 'NONE', *, *, #13036, .F. ) ;
#18651 = DIRECTION ( 'NONE',  ( 1.000000000000000000, 0.000000000000000000, 0.000000000000000000 ) ) ;
#18652 = CARTESIAN_POINT ( 'NONE',  ( 20.39194369155392295, -16.19744444934939764, 22.99999999999999289 ) ) ;
#18653 = AXIS2_PLACEMENT_3D ( 'NONE', #514, #15750, #3556 ) ;
#18654 = CARTESIAN_POINT ( 'NONE',  ( -25.51179355227999679, 0.9159808143456273921, -16.49580793394636302 ) ) ;
#18655 = CARTESIAN_POINT ( 'NONE',  ( 22.98695121338641201, -8.481255122890857479, -20.78017015740226725 ) ) ;
#18656 = VECTOR ( 'NONE', #27756, 1000.000000000000000 ) ;
#18657 = ORIENTED_EDGE ( 'NONE', *, *, #16466, .F. ) ;
#18658 = PLANE ( 'NONE',  #12205 ) ;
#18659 = ORIENTED_EDGE ( 'NONE', *, *, #8863, .T. ) ;
#18660 = PLANE ( 'NONE',  #12578 ) ;
#18661 = CARTESIAN_POINT ( 'NONE',  ( 27.36225479881668576, 10.16098284218095493, 22.99999999999999645 ) ) ;
#18662 = CARTESIAN_POINT ( 'NONE',  ( -16.99999999999999645, 22.50000000000000355, 13.00000000000000178 ) ) ;
#18663 = ORIENTED_EDGE ( 'NONE', *, *, #6931, .F. ) ;
#18664 = CARTESIAN_POINT ( 'NONE',  ( -4.032443027607593322, 36.05064863044662360, -9.738485491014769124 ) ) ;
#18665 = CARTESIAN_POINT ( 'NONE',  ( -9.284827327736387304, 10.70480225629000870, 10.49999999999999645 ) ) ;
#18666 = CARTESIAN_POINT ( 'NONE',  ( 7.064564986133971658, 13.54338174056915456, 13.00000000000000178 ) ) ;
#18667 = DIRECTION ( 'NONE',  ( 1.000000000000000000, 0.000000000000000000, 0.000000000000000000 ) ) ;
#18668 = CARTESIAN_POINT ( 'NONE',  ( 17.44545305909492683, -13.38241287727507256, -24.26558710457006285 ) ) ;
#18669 = CARTESIAN_POINT ( 'NONE',  ( 16.23943293897244544, 12.53170227796935343, -30.00000000000000355 ) ) ;
#18670 = CIRCLE ( 'NONE', #6986, 1.000000000000000000 ) ;
#18671 = CARTESIAN_POINT ( 'NONE',  ( 11.98794441292618984, 28.67068012064173388, -12.24360472531066968 ) ) ;
#18672 = CIRCLE ( 'NONE', #38122, 6.000000000000000888 ) ;
#18673 = ORIENTED_EDGE ( 'NONE', *, *, #34472, .F. ) ;
#18674 = CARTESIAN_POINT ( 'NONE',  ( -20.80119427603082016, 12.44190052851605444, -10.38726145399924050 ) ) ;
#18675 = CARTESIAN_POINT ( 'NONE',  ( 4.441848239913452900, 24.85865334748800848, 23.00000000000000355 ) ) ;
#18676 = CARTESIAN_POINT ( 'NONE',  ( 15.68314276670921359, -26.79173994879206688, -5.473249617827911528 ) ) ;
#18677 = LINE ( 'NONE', #12573, #6121 ) ;
#18678 = AXIS2_PLACEMENT_3D ( 'NONE', #14155, #17626, #20259 ) ;
#18679 = CARTESIAN_POINT ( 'NONE',  ( -5.636483973512888213, -22.01575377102104625, -29.99999999999999645 ) ) ;
#18680 = CARTESIAN_POINT ( 'NONE',  ( 5.198706521309295780, 29.65540566576566661, 9.000000000000001776 ) ) ;
#18681 = AXIS2_PLACEMENT_3D ( 'NONE', #20754, #2655, #27433 ) ;
#18682 = CARTESIAN_POINT ( 'NONE',  ( -15.15864152013962673, 26.33530742007706138, -8.295770841832171172 ) ) ;
#18683 = CARTESIAN_POINT ( 'NONE',  ( -13.12770624849639844, -15.75833046460326692, -30.00000000000001421 ) ) ;
#18684 = CARTESIAN_POINT ( 'NONE',  ( 10.69843551445597463, -25.55873913893780269, -6.902590252133971482 ) ) ;
#18685 = EDGE_CURVE ( 'NONE', #24743, #23135, #32476, .T. ) ;
#18686 = CARTESIAN_POINT ( 'NONE',  ( 5.644276917315719011, 36.40655018617690786, 10.49999999999999822 ) ) ;
#18687 = ORIENTED_EDGE ( 'NONE', *, *, #1118, .T. ) ;
#18688 = CARTESIAN_POINT ( 'NONE',  ( -6.721507432170120033, 20.19422004900923895, -25.81187786869902112 ) ) ;
#18689 = CARTESIAN_POINT ( 'NONE',  ( 4.835130509701799362, 15.55077355964573904, 12.00000000000000000 ) ) ;
#18690 = DIRECTION ( 'NONE',  ( 0.000000000000000000, 0.000000000000000000, 1.000000000000000000 ) ) ;
#18691 = DIRECTION ( 'NONE',  ( -0.4067366430758009299, -0.9135454576426005335, 0.000000000000000000 ) ) ;
#18692 = ORIENTED_EDGE ( 'NONE', *, *, #30211, .F. ) ;
#18693 = CARTESIAN_POINT ( 'NONE',  ( 30.89317523684279010, -0.03095884371312801128, -5.474201754116363006 ) ) ;
#18694 = EDGE_CURVE ( 'NONE', #19098, #15240, #37954, .T. ) ;
#18695 = DIRECTION ( 'NONE',  ( 1.000000000000000000, 0.000000000000000000, 0.000000000000000000 ) ) ;
#18696 = DIRECTION ( 'NONE',  ( -1.000000000000000000, 0.000000000000000000, 0.000000000000000000 ) ) ;
#18697 = EDGE_CURVE ( 'NONE', #32625, #29611, #35308, .T. ) ;
#18698 = EDGE_LOOP ( 'NONE', ( #36622, #9234, #10520, #29643 ) ) ;
#18699 = CARTESIAN_POINT ( 'NONE',  ( -23.30556412954694778, 0.5841231897993812705, -20.54594922719505234 ) ) ;
#18700 = CARTESIAN_POINT ( 'NONE',  ( 4.591666147298500533, 15.32946292166668556, 7.000000000000000000 ) ) ;
#18701 = ORIENTED_EDGE ( 'NONE', *, *, #33709, .T. ) ;
#18702 = CARTESIAN_POINT ( 'NONE',  ( 28.84037157294331521, -5.093697924006990618, -14.99084036193530345 ) ) ;
#18703 = CIRCLE ( 'NONE', #27774, 0.5000000000000004441 ) ;
#18704 = VECTOR ( 'NONE', #21982, 1000.000000000000000 ) ;
#18705 = EDGE_LOOP ( 'NONE', ( #8154, #18332, #36197, #4269 ) ) ;
#18706 = CARTESIAN_POINT ( 'NONE',  ( 10.85362879025560545, 36.78189293023390150, 12.14047268033097637 ) ) ;
#18707 = CIRCLE ( 'NONE', #1190, 16.00000000000000000 ) ;
#18708 = CARTESIAN_POINT ( 'NONE',  ( 5.688300058587269170, 16.47782454277055564, 6.000000000000000000 ) ) ;
#18709 = CARTESIAN_POINT ( 'NONE',  ( 8.559505275947156377, 25.28115294937476065, 6.000000000000000000 ) ) ;
#18710 = CARTESIAN_POINT ( 'NONE',  ( -6.290729337819993994, 29.14951258272757073, 20.50957957746074456 ) ) ;
#18711 = CIRCLE ( 'NONE', #1193, 1.000000000000013101 ) ;
#18712 = CARTESIAN_POINT ( 'NONE',  ( -3.370709253380788084E-06, 22.50000000000031264, 13.00000000000000178 ) ) ;
#18713 = ORIENTED_EDGE ( 'NONE', *, *, #22037, .F. ) ;
#18714 = DIRECTION ( 'NONE',  ( 0.000000000000000000, 0.000000000000000000, 1.000000000000000000 ) ) ;
#18715 = DIRECTION ( 'NONE',  ( -0.3090169943749589976, -0.9510565162951498674, 0.000000000000000000 ) ) ;
#18716 = EDGE_CURVE ( 'NONE', #10782, #22096, #29101, .T. ) ;
#18717 = CARTESIAN_POINT ( 'NONE',  ( -3.370709253380788084E-06, 22.50000000000031264, 12.00000000000000000 ) ) ;
#18718 = EDGE_CURVE ( 'NONE', #14858, #6691, #985, .T. ) ;
#18719 = LINE ( 'NONE', #28051, #25333 ) ;
#18720 = CARTESIAN_POINT ( 'NONE',  ( 6.275750612750602642, 24.42035190817285795, -19.81826795694746224 ) ) ;
#18721 = CARTESIAN_POINT ( 'NONE',  ( 11.21453531681511784, -17.17359087135386631, -29.31171484545407324 ) ) ;
#18722 = DIRECTION ( 'NONE',  ( -0.000000000000000000, -0.000000000000000000, 1.000000000000000000 ) ) ;
#18723 = DIRECTION ( 'NONE',  ( -0.6691306063588570163, 0.7431448254773953543, -0.000000000000000000 ) ) ;
#18724 = AXIS2_PLACEMENT_3D ( 'NONE', #18352, #9999, #31333 ) ;
#18725 = EDGE_LOOP ( 'NONE', ( #13684, #37777, #27967, #33051 ) ) ;
#18727 = VECTOR ( 'NONE', #16090, 1000.000000000000000 ) ;
#18726 = CARTESIAN_POINT ( 'NONE',  ( -12.67439586582248268, 21.02274553044240690, -18.45589385857095266 ) ) ;
#18728 = CARTESIAN_POINT ( 'NONE',  ( -20.52459090776379114, -25.56956579041120747, 17.92354375535250810 ) ) ;
#18729 = CARTESIAN_POINT ( 'NONE',  ( 15.08885268118981493, -26.51893482596228679, -6.888510563021540634 ) ) ;
#18730 = CARTESIAN_POINT ( 'NONE',  ( 3.820972158148982167, 8.017991022712324778, 10.49999999999999467 ) ) ;
#18731 = ORIENTED_EDGE ( 'NONE', *, *, #8423, .F. ) ;
#18732 = ORIENTED_EDGE ( 'NONE', *, *, #8830, .T. ) ;
#18733 = AXIS2_PLACEMENT_3D ( 'NONE', #8419, #11267, #29945 ) ;
#18734 = CARTESIAN_POINT ( 'NONE',  ( -10.57894702805681320, 19.19023191218746049, -23.71264430011183677 ) ) ;
#18735 = CARTESIAN_POINT ( 'NONE',  ( -11.63857182560571069, -18.06026089823302883, -24.81603628889719815 ) ) ;
#18736 = EDGE_CURVE ( 'NONE', #2141, #39108, #14460, .T. ) ;
#18737 = FACE_BOUND ( 'NONE', #29290, .T. ) ;
#18738 = EDGE_LOOP ( 'NONE', ( #36432, #8403, #35776, #14928, #25570 ) ) ;
#18739 = CARTESIAN_POINT ( 'NONE',  ( -20.89731588449937050, -6.521350128711503658, -24.35897028945197107 ) ) ;
#18740 = CARTESIAN_POINT ( 'NONE',  ( -11.05277117942599929, -20.49230150080012436, -20.55679038895522481 ) ) ;
#18741 = CARTESIAN_POINT ( 'NONE',  ( 4.458865582155095986, 18.48521636184714012, 12.00000000000000000 ) ) ;
#18742 = ORIENTED_EDGE ( 'NONE', *, *, #33004, .T. ) ;
#18743 = CARTESIAN_POINT ( 'NONE',  ( 26.35681613863516048, 0.5053618088134171904, -15.46827064861124512 ) ) ;
#18744 = B_SPLINE_CURVE_WITH_KNOTS ( 'NONE', 3,
 ( #29445, #26395, #7098, #16457, #29043, #13400, #10161, #13601 ),
 .UNSPECIFIED., .F., .F.,
 ( 4, 2, 2, 4 ),
 ( 0.000000000000000000, 0.0002364868538934293248, 0.0004729737077868575112, 0.0009459474155737107939 ),
 .UNSPECIFIED. ) ;
#18745 = CYLINDRICAL_SURFACE ( 'NONE', #9620, 6.000000000000008882 ) ;
#18746 = LINE ( 'NONE', #12439, #34840 ) ;
#18747 = ORIENTED_EDGE ( 'NONE', *, *, #27248, .F. ) ;
#18748 = CARTESIAN_POINT ( 'NONE',  ( -20.48364860518192998, 0.8189024673161406920, -30.00000000000000000 ) ) ;
#18749 = EDGE_LOOP ( 'NONE', ( #15581, #10608 ) ) ;
#18750 = CARTESIAN_POINT ( 'NONE',  ( 25.24172059964007175, -1.134046536396660310, -18.25343667544089499 ) ) ;
#18751 = CARTESIAN_POINT ( 'NONE',  ( 17.12152044068272971, -11.27946124554793883, -30.00000000000003553 ) ) ;
#18752 = CARTESIAN_POINT ( 'NONE',  ( 27.81120771500035005, -23.04947625254933286, 17.92354375535213862 ) ) ;
#18753 = ORIENTED_EDGE ( 'NONE', *, *, #35614, .F. ) ;
#18754 = CARTESIAN_POINT ( 'NONE',  ( -26.44546049722394798, 4.400203990190252767, -8.831313265021430325 ) ) ;
#18755 = CARTESIAN_POINT ( 'NONE',  ( -14.45538749008468038, 26.50521816028845734, 7.489440493383480835 ) ) ;
#18756 = DIRECTION ( 'NONE',  ( -0.4999999999999920064, 0.8660254037844432595, 0.000000000000000000 ) ) ;
#18757 = CIRCLE ( 'NONE', #31082, 1.000000000000000888 ) ;
#18758 = AXIS2_PLACEMENT_3D ( 'NONE', #17843, #36320, #35915 ) ;
#18759 = FACE_OUTER_BOUND ( 'NONE', #2351, .T. ) ;
#18760 = PLANE ( 'NONE',  #25982 ) ;
#18761 = EDGE_CURVE ( 'NONE', #29912, #1935, #3157, .T. ) ;
#18762 = B_SPLINE_SURFACE_WITH_KNOTS ( 'NONE', 1, 3, ( 
 ( #2848, #15236, #12188, #39813, #18098, #15035, #27427, #24581, #18491, #9142 ),
 ( #21527, #6086, #15436, #24775, #27827, #12385, #9345, #21725, #17206, #32441 ) ),
 .UNSPECIFIED., .F., .F., .F.,
 ( 2, 2 ),
 ( 4, 2, 2, 2, 4 ),
 ( 0.000000000000000000, 1.000000000000000000 ),
 ( 1.570796326794897002, 1.963495408493620920, 2.356194490192344837, 2.748893571891068976, 3.141592653589793116 ),
 .UNSPECIFIED. ) ;
#18763 = CARTESIAN_POINT ( 'NONE',  ( -30.90412082983564446, -0.04211290444597337590, -5.000000000000000888 ) ) ;
#18764 = CARTESIAN_POINT ( 'NONE',  ( 20.35904855840089311, 17.61891361913472309, 13.32518128616558784 ) ) ;
#18765 = CARTESIAN_POINT ( 'NONE',  ( -23.22194232212845577, 6.892050143596356371, -13.82897816699491678 ) ) ;
#18766 = CARTESIAN_POINT ( 'NONE',  ( 12.99377146717205633, 26.19620116591417869, 7.000000000000000000 ) ) ;
#18767 = DIRECTION ( 'NONE',  ( 1.000000000000000000, 0.000000000000000000, 0.000000000000000000 ) ) ;
#18768 = CARTESIAN_POINT ( 'NONE',  ( 21.28768541942379144, -24.85472925722318749, -11.24091203251788684 ) ) ;
#18769 = FACE_OUTER_BOUND ( 'NONE', #35511, .T. ) ;
#18770 = CARTESIAN_POINT ( 'NONE',  ( 14.18431540342452912, 24.75056589267492058, -12.52692153250820617 ) ) ;
#18771 = ORIENTED_EDGE ( 'NONE', *, *, #6638, .F. ) ;
#18772 = CARTESIAN_POINT ( 'NONE',  ( -15.01220060599063189, 22.71241345319973348, -12.61924114651307960 ) ) ;
#18773 = CARTESIAN_POINT ( 'NONE',  ( -24.76266088601904514, -18.72941319223700773, 20.50957957746028981 ) ) ;
#18774 = DIRECTION ( 'NONE',  ( 1.000000000000000000, 0.000000000000000000, 0.000000000000000000 ) ) ;
#18775 = CARTESIAN_POINT ( 'NONE',  ( 11.33221106479448714, 18.02071959632803910, -25.01755605303010555 ) ) ;
#18776 = VERTEX_POINT ( 'NONE', #10126 ) ;
#18777 = CARTESIAN_POINT ( 'NONE',  ( -20.33644687577595178, 12.50987689638972356, 7.000000000000000000 ) ) ;
#18778 = VERTEX_POINT ( 'NONE', #16629 ) ;
#18780 = DIRECTION ( 'NONE',  ( 0.5877852522924689183, -0.8090169943749505599, 0.000000000000000000 ) ) ;
#18779 = CARTESIAN_POINT ( 'NONE',  ( -10.83390719878747355, 17.40340976726015398, -29.99999999999999289 ) ) ;
#18781 = CARTESIAN_POINT ( 'NONE',  ( -15.70264670462719714, -26.79635097760029794, -5.000000000000000888 ) ) ;
#18782 = EDGE_CURVE ( 'NONE', #20347, #25619, #33015, .T. ) ;
#18783 = FACE_OUTER_BOUND ( 'NONE', #37376, .T. ) ;
#18784 = AXIS2_PLACEMENT_3D ( 'NONE', #6408, #12907, #923 ) ;
#18785 = VERTEX_POINT ( 'NONE', #4428 ) ;
#18786 = CARTESIAN_POINT ( 'NONE',  ( -25.09485740259016850, -12.19075756865849947, -17.60690265804054278 ) ) ;
#18787 = CARTESIAN_POINT ( 'NONE',  ( -11.29805317986360258, -25.35288615261349676, -8.807478906485194159 ) ) ;
#18788 = LINE ( 'NONE', #10439, #39087 ) ;
#18789 = CARTESIAN_POINT ( 'NONE',  ( 14.35723387269807461, 20.24307895078839792, -16.61037614182657052 ) ) ;
#18791 = EDGE_CURVE ( 'NONE', #12667, #8118, #20078, .T. ) ;
#18790 = VERTEX_POINT ( 'NONE', #31856 ) ;
#18792 = CARTESIAN_POINT ( 'NONE',  ( 25.84550903417051160, 5.566988420567247076, -7.396971983680807661 ) ) ;
#18793 = FACE_OUTER_BOUND ( 'NONE', #38373, .T. ) ;
#18794 = EDGE_CURVE ( 'NONE', #36223, #38699, #23918, .T. ) ;
#18795 = CARTESIAN_POINT ( 'NONE',  ( 6.654030453887980201, 35.94335816374507431, 7.500000000000000888 ) ) ;
#18796 = DIRECTION ( 'NONE',  ( 1.000000000000000000, -1.040834085586081417E-14, 0.000000000000000000 ) ) ;
#18797 = AXIS2_PLACEMENT_3D ( 'NONE', #23150, #815, #7102 ) ;
#18798 = ORIENTED_EDGE ( 'NONE', *, *, #38206, .T. ) ;
#18799 = CARTESIAN_POINT ( 'NONE',  ( -30.61729485247184002, -0.2875646607849730585, -8.283315588427790033 ) ) ;
#18800 = CARTESIAN_POINT ( 'NONE',  ( 20.83381800968227182, 0.6014786412957214834, -26.81279315949302955 ) ) ;
#18801 = ADVANCED_FACE ( 'NONE', ( #16833 ), #4227, .F. ) ;
#18802 = CARTESIAN_POINT ( 'NONE',  ( 25.50184330511968156, -18.07811769911567978, 20.50957957746029336 ) ) ;
#18803 = ORIENTED_EDGE ( 'NONE', *, *, #39347, .T. ) ;
#18804 = CARTESIAN_POINT ( 'NONE',  ( 8.937590682902566641, -20.71651963383554218, -21.24786896499729494 ) ) ;
#18805 = DIRECTION ( 'NONE',  ( -0.7431448254773953543, -0.6691306063588570163, 0.000000000000000000 ) ) ;
#18806 = ORIENTED_EDGE ( 'NONE', *, *, #9911, .F. ) ;
#18807 = CARTESIAN_POINT ( 'NONE',  ( -9.742785792574970571, -49.01344959084108410, 20.99999999999999645 ) ) ;
#18808 = ADVANCED_FACE ( 'NONE', ( #1588 ), #3824, .T. ) ;
#18809 = EDGE_CURVE ( 'NONE', #6441, #38979, #16792, .T. ) ;
#18810 = VECTOR ( 'NONE', #25808, 1000.000000000000114 ) ;
#18811 = CARTESIAN_POINT ( 'NONE',  ( 6.282361020112160688, 14.70372268239673197, 10.49999999999999822 ) ) ;
#18812 = CARTESIAN_POINT ( 'NONE',  ( 37.28744356507513658, -7.587582650827097375, -5.000000000000016875 ) ) ;
#18813 = CARTESIAN_POINT ( 'NONE',  ( 1.444440266932477623, 20.45847851156178265, -29.21425697047676451 ) ) ;
#18814 = CARTESIAN_POINT ( 'NONE',  ( 2.835130509701798918, 15.55077355964573904, 13.00000000000000178 ) ) ;
#18815 = FACE_OUTER_BOUND ( 'NONE', #19636, .T. ) ;
#18816 = DIRECTION ( 'NONE',  ( 1.000000000000000000, 0.000000000000000000, 0.000000000000000000 ) ) ;
#18817 = CONICAL_SURFACE ( 'NONE', #12950, 0.5000000000000013323, 0.7853981633974529419 ) ;
#18818 = CARTESIAN_POINT ( 'NONE',  ( 9.665073660139013256, 25.11464168560187460, 10.50000000000000711 ) ) ;
#18819 = CARTESIAN_POINT ( 'NONE',  ( -2.211402178667006169, 32.38366924255629442, 12.00000000000000000 ) ) ;
#18820 = DIRECTION ( 'NONE',  ( 0.000000000000000000, 0.000000000000000000, 1.000000000000000000 ) ) ;
#18821 = CARTESIAN_POINT ( 'NONE',  ( 10.13018406787138304, 17.82246755199521360, -29.33001752643188453 ) ) ;
#18822 = DIRECTION ( 'NONE',  ( 0.000000000000000000, 0.000000000000000000, 1.000000000000000000 ) ) ;
#18823 = ORIENTED_EDGE ( 'NONE', *, *, #4478, .T. ) ;
#18825 = LINE ( 'NONE', #335, #39518 ) ;
#18824 = CARTESIAN_POINT ( 'NONE',  ( -18.04083112182678406, 18.37157263296915133, -8.860390942907290679 ) ) ;
#18826 = DIRECTION ( 'NONE',  ( -0.3090169943749573878, -0.9510565162951503115, 0.000000000000000000 ) ) ;
#18827 = CARTESIAN_POINT ( 'NONE',  ( 10.84768000140452848, -19.98809413286245018, -21.61592137937718761 ) ) ;
#18828 = CARTESIAN_POINT ( 'NONE',  ( -21.44652559126361879, -26.87240656024164664, -7.228200811290371952 ) ) ;
#18829 = CARTESIAN_POINT ( 'NONE',  ( 14.29473281614541946, 24.46189118728469225, -12.55068749070381884 ) ) ;
#18830 = CARTESIAN_POINT ( 'NONE',  ( 14.52401956015651230, 24.99458846522630751, -11.59728651514169684 ) ) ;
#18831 = ORIENTED_EDGE ( 'NONE', *, *, #28583, .F. ) ;
#18832 = CARTESIAN_POINT ( 'NONE',  ( 12.80736835487433289, 15.68301270189216545, 7.000000000000000000 ) ) ;
#18833 = CARTESIAN_POINT ( 'NONE',  ( -14.78861890278166413, -25.81514123692260299, -9.710278502422099223 ) ) ;
#18834 = EDGE_CURVE ( 'NONE', #23552, #18136, #23284, .T. ) ;
#18835 = CARTESIAN_POINT ( 'NONE',  ( -20.76390118686629549, -28.86769433464280610, 13.32518128616608877 ) ) ;
#18836 = CARTESIAN_POINT ( 'NONE',  ( -20.30545432580447240, -13.99291260258515379, -20.70863365825785962 ) ) ;
#18837 = CARTESIAN_POINT ( 'NONE',  ( -2.563881278962895749, -24.61887866671625247, -7.916840171043283192 ) ) ;
#18838 = CARTESIAN_POINT ( 'NONE',  ( 15.21168623108442475, 24.52100632137278069, -10.20105120338589622 ) ) ;
#18839 = EDGE_CURVE ( 'NONE', #14121, #35424, #16224, .T. ) ;
#18840 = CARTESIAN_POINT ( 'NONE',  ( 18.89612423569448296, 9.643090400953798991, -23.32574488315787065 ) ) ;
#18841 = CARTESIAN_POINT ( 'NONE',  ( -12.25578195141909177, -14.54847271968242595, 23.00000000000000000 ) ) ;
#18842 = ORIENTED_EDGE ( 'NONE', *, *, #11014, .F. ) ;
#18843 = CARTESIAN_POINT ( 'NONE',  ( -33.03352659232529476, -3.420569429262189765, -7.712445482004824271 ) ) ;
#18844 = ADVANCED_FACE ( 'NONE', ( #25553 ), #7468, .T. ) ;
#18845 = CARTESIAN_POINT ( 'NONE',  ( -19.72827082055129111, 4.852702923346353892, 19.99202127657103389 ) ) ;
#18846 = ORIENTED_EDGE ( 'NONE', *, *, #13395, .T. ) ;
#18847 = CARTESIAN_POINT ( 'NONE',  ( -2.518583951651200081, 7.712953814960714638, 7.000000000000000000 ) ) ;
#18848 = CARTESIAN_POINT ( 'NONE',  ( 10.39021566973303656, 20.90519018800546291, 10.50000000000000000 ) ) ;
#18849 = CARTESIAN_POINT ( 'NONE',  ( -20.65398372803566573, 1.346249621251496054, -27.47960346742159743 ) ) ;
#18850 = CARTESIAN_POINT ( 'NONE',  ( 19.23659220497393108, -7.112289578705963677, -29.22637812988511641 ) ) ;
#18851 = CARTESIAN_POINT ( 'NONE',  ( 31.94006737154590070, 0.9747213384848182338, 13.92931973827809067 ) ) ;
#18852 = EDGE_LOOP ( 'NONE', ( #9795, #8971, #38786, #29077 ) ) ;
#18853 = DIRECTION ( 'NONE',  ( -1.000000000000000000, 0.000000000000000000, 0.000000000000000000 ) ) ;
#18854 = ORIENTED_EDGE ( 'NONE', *, *, #15113, .F. ) ;
#18855 = CARTESIAN_POINT ( 'NONE',  ( -0.9999999999999993339, 32.50000000000000000, 10.50000000000000178 ) ) ;
#18856 = CARTESIAN_POINT ( 'NONE',  ( 20.57678504272533004, 23.15270735503113286, 11.00000000000000000 ) ) ;
#18857 = ADVANCED_FACE ( 'NONE', ( #26158 ), #35107, .F. ) ;
#18858 = VECTOR ( 'NONE', #28092, 999.9999999999998863 ) ;
#18859 = CARTESIAN_POINT ( 'NONE',  ( -12.03641663870442713, 15.85735326529964873, 13.00000000000000178 ) ) ;
#18860 = ORIENTED_EDGE ( 'NONE', *, *, #39192, .T. ) ;
#18861 = CARTESIAN_POINT ( 'NONE',  ( -2.050360002403428972, 25.60080579252921495, -19.64802405917689754 ) ) ;
#18862 = AXIS2_PLACEMENT_3D ( 'NONE', #13557, #23315, #25944 ) ;
#18863 = DIRECTION ( 'NONE',  ( 1.000000000000000000, 0.000000000000000000, 0.000000000000000000 ) ) ;
#18864 = DIRECTION ( 'NONE',  ( 0.000000000000000000, 0.000000000000000000, 1.000000000000000000 ) ) ;
#18865 = CARTESIAN_POINT ( 'NONE',  ( -0.4999999999999998890, 37.50000000000000711, 7.000000000000000000 ) ) ;
#18866 = CARTESIAN_POINT ( 'NONE',  ( 3.476901250629512941, 26.36149378532653031, 13.00000000000000178 ) ) ;
#18867 = CARTESIAN_POINT ( 'NONE',  ( 9.840690490415067160, 20.46019347195515792, 10.50000000000000533 ) ) ;
#18868 = CARTESIAN_POINT ( 'NONE',  ( 14.23294558246579022, 29.80882899807581055, -4.999999999999997335 ) ) ;
#18869 = VERTEX_POINT ( 'NONE', #8075 ) ;
#18870 = CARTESIAN_POINT ( 'NONE',  ( -21.06328208572556093, 12.60356320803115970, -8.409244101891895085 ) ) ;
#18871 = CARTESIAN_POINT ( 'NONE',  ( 7.935770203493858865, 22.34671014717335780, 13.00000000000000178 ) ) ;
#18872 = CARTESIAN_POINT ( 'NONE',  ( 14.22674418391079243, -24.64141992797763336, -12.53611091602331662 ) ) ;
#18873 = DIRECTION ( 'NONE',  ( 0.000000000000000000, 0.000000000000000000, 1.000000000000000000 ) ) ;
#18874 = CIRCLE ( 'NONE', #1361, 1.000000000000000000 ) ;
#18875 = CARTESIAN_POINT ( 'NONE',  ( 14.90698185259310016, 25.88873565208333005, -9.704017660486000452 ) ) ;
#18876 = CARTESIAN_POINT ( 'NONE',  ( 8.937590682902566641, -20.71651963383554218, -30.00000000000000000 ) ) ;
#18877 = CARTESIAN_POINT ( 'NONE',  ( -10.59792294478258334, 33.06643021166741647, 10.49999999999999822 ) ) ;
#18878 = CARTESIAN_POINT ( 'NONE',  ( -15.45681155788697936, -16.36624024623564111, -23.23867721921044804 ) ) ;
#18879 = CARTESIAN_POINT ( 'NONE',  ( 10.50810896484892254, -25.22781171335135042, -8.817308065532962758 ) ) ;
#18880 = CARTESIAN_POINT ( 'NONE',  ( 12.19824770565493566, 19.84438704282505839, -20.55290514491795406 ) ) ;
#18881 = EDGE_CURVE ( 'NONE', #7713, #37486, #39556, .T. ) ;
#18882 = CARTESIAN_POINT ( 'NONE',  ( 17.05875634882093195, -11.52365334420840881, -28.44935981325557250 ) ) ;
#18883 = CARTESIAN_POINT ( 'NONE',  ( 8.412270287199628882, 10.07085245822955955, 10.59344459855562803 ) ) ;
#18884 = CARTESIAN_POINT ( 'NONE',  ( 5.459721035625122454, 35.99203088905944981, 11.00000000000000000 ) ) ;
#18885 = ORIENTED_EDGE ( 'NONE', *, *, #31009, .F. ) ;
#18886 = CARTESIAN_POINT ( 'NONE',  ( -10.90236520000052245, 33.11211960170862767, -8.515142989435695142 ) ) ;
#18887 = LINE ( 'NONE', #33930, #21217 ) ;
#18888 = DIRECTION ( 'NONE',  ( 1.000000000000000000, 0.000000000000000000, 0.000000000000000000 ) ) ;
#18889 = DIRECTION ( 'NONE',  ( -1.000000000000000000, 0.000000000000000000, 0.000000000000000000 ) ) ;
#18890 = ORIENTED_EDGE ( 'NONE', *, *, #29947, .T. ) ;
#18891 = CARTESIAN_POINT ( 'NONE',  ( 20.81362228500634970, 0.8536333317955857591, -26.83237868093558731 ) ) ;
#18892 = CARTESIAN_POINT ( 'NONE',  ( 75.15099915297797395, 43.38844959084117647, 3.000000000000000000 ) ) ;
#18893 = FACE_OUTER_BOUND ( 'NONE', #4739, .T. ) ;
#18894 = ORIENTED_EDGE ( 'NONE', *, *, #29593, .T. ) ;
#18895 = CARTESIAN_POINT ( 'NONE',  ( -27.71741899510553608, 0.2170695715558252636, -13.51503484893205531 ) ) ;
#18896 = CARTESIAN_POINT ( 'NONE',  ( -13.26585111513660031, 17.86474508437623143, 12.00000000000000000 ) ) ;
#18897 = ORIENTED_EDGE ( 'NONE', *, *, #36804, .T. ) ;
#18898 = CARTESIAN_POINT ( 'NONE',  ( 20.21125490546006276, -3.489748019849370220, -29.27149083989724687 ) ) ;
#18899 = EDGE_LOOP ( 'NONE', ( #17752, #35389 ) ) ;
#18900 = CARTESIAN_POINT ( 'NONE',  ( 5.682704777076756031, 39.36960561607962461, 12.73282698324853257 ) ) ;
#18901 = VECTOR ( 'NONE', #37749, 1000.000000000000114 ) ;
#18902 = DIRECTION ( 'NONE',  ( -0.000000000000000000, -0.000000000000000000, -1.000000000000000000 ) ) ;
#18903 = DIRECTION ( 'NONE',  ( -1.000000000000000000, 0.000000000000000000, 0.000000000000000000 ) ) ;
#18904 = CARTESIAN_POINT ( 'NONE',  ( -11.11100267139600639, 25.58833710557283325, 19.66345542862528362 ) ) ;
#18905 = CARTESIAN_POINT ( 'NONE',  ( 22.17929659509128371, 23.57150372095986057, 10.00000000000000000 ) ) ;
#18906 = ORIENTED_EDGE ( 'NONE', *, *, #40178, .F. ) ;
#18907 = CARTESIAN_POINT ( 'NONE',  ( -14.52509594610762456, 21.97885917798744870, 9.500000000000000000 ) ) ;
#18908 = EDGE_CURVE ( 'NONE', #28710, #39968, #18101, .T. ) ;
#18909 = CARTESIAN_POINT ( 'NONE',  ( -19.61636114005775511, 5.963768710578694510, -30.00000000000001776 ) ) ;
#18910 = DIRECTION ( 'NONE',  ( -0.8660254037844364872, 0.5000000000000038858, 0.000000000000000000 ) ) ;
#18911 = EDGE_CURVE ( 'NONE', #36946, #14129, #30427, .T. ) ;
#18912 = DIRECTION ( 'NONE',  ( 1.000000000000000000, 0.000000000000000000, 0.000000000000000000 ) ) ;
#18913 = CARTESIAN_POINT ( 'NONE',  ( 17.34393471781637075, 19.49149365859844352, -9.816462853724280180 ) ) ;
#18914 = CARTESIAN_POINT ( 'NONE',  ( 9.500382936455952887, 32.89299068974253260, -10.27676952640711505 ) ) ;
#18915 = AXIS2_PLACEMENT_3D ( 'NONE', #31059, #21900, #21705 ) ;
#18916 = CIRCLE ( 'NONE', #35129, 2.000000000000001776 ) ;
#18917 = EDGE_CURVE ( 'NONE', #8131, #38584, #29815, .T. ) ;
#18918 = CARTESIAN_POINT ( 'NONE',  ( 16.58821223849002635, -25.78030334186819772, -10.53774966371608279 ) ) ;
#18919 = CARTESIAN_POINT ( 'NONE',  ( 9.363324537585983265, 32.27640801132196913, 10.50000000000000000 ) ) ;
#18920 = DIRECTION ( 'NONE',  ( 0.000000000000000000, 0.000000000000000000, -1.000000000000000000 ) ) ;
#18921 = EDGE_LOOP ( 'NONE', ( #6294, #31803 ) ) ;
#18922 = CARTESIAN_POINT ( 'NONE',  ( -11.46775114909779880, 17.91482654455204937, -25.03573280478206797 ) ) ;
#18923 = CARTESIAN_POINT ( 'NONE',  ( -34.20210851612425529, -5.988401547694746974, 16.87380292611485899 ) ) ;
#18924 = CARTESIAN_POINT ( 'NONE',  ( 12.17258182436908065, -22.02639489287507502, -17.44778068929893067 ) ) ;
#18925 = CONICAL_SURFACE ( 'NONE', #770, 0.9999999999999991118, 0.7853981633974502774 ) ;
#18926 = LINE ( 'NONE', #25816, #30906 ) ;
#18927 = ORIENTED_EDGE ( 'NONE', *, *, #36802, .T. ) ;
#18928 = VERTEX_POINT ( 'NONE', #14377 ) ;
#18929 = CARTESIAN_POINT ( 'NONE',  ( -13.49361715555115282, 27.40176124217998321, -11.42939491410920994 ) ) ;
#18930 = CARTESIAN_POINT ( 'NONE',  ( -11.98442307596994816, -17.42517490280342329, -26.00811570201611289 ) ) ;
#18931 = FACE_BOUND ( 'NONE', #5134, .T. ) ;
#18932 = VERTEX_POINT ( 'NONE', #17646 ) ;
#18933 = CARTESIAN_POINT ( 'NONE',  ( -21.06133918572757224, -5.879866026727245121, -24.39648093831449671 ) ) ;
#18934 = CARTESIAN_POINT ( 'NONE',  ( -12.16148876965757530, -22.02675247291305283, -17.44874281179136943 ) ) ;
#18935 = DIRECTION ( 'NONE',  ( 0.000000000000000000, 0.000000000000000000, 1.000000000000000000 ) ) ;
#18936 = EDGE_LOOP ( 'NONE', ( #17545, #9952, #17293, #23560 ) ) ;
#18937 = CARTESIAN_POINT ( 'NONE',  ( 26.41552486178371950, 1.278391022459212545, -14.54603937267712332 ) ) ;
#18938 = LINE ( 'NONE', #3496, #5729 ) ;
#18939 = DIRECTION ( 'NONE',  ( -1.000000000000000000, 0.000000000000000000, 0.000000000000000000 ) ) ;
#18940 = ADVANCED_FACE ( 'NONE', ( #17239 ), #33285, .F. ) ;
#18941 = VERTEX_POINT ( 'NONE', #26764 ) ;
#18942 = CARTESIAN_POINT ( 'NONE',  ( -20.97406219683946915, 0.7643328109957392424, -26.22104410486783976 ) ) ;
#18943 = ORIENTED_EDGE ( 'NONE', *, *, #6890, .F. ) ;
#18944 = CARTESIAN_POINT ( 'NONE',  ( 23.71077850922558738, -0.6311408168542613772, -20.38398171457574293 ) ) ;
#18945 = CARTESIAN_POINT ( 'NONE',  ( 19.42600269443267891, -6.688926838600538716, -30.00000000000002842 ) ) ;
#18946 = CARTESIAN_POINT ( 'NONE',  ( 31.75251099004278288, -1.565804367081077064, 16.87380292611637245 ) ) ;
#18947 = ORIENTED_EDGE ( 'NONE', *, *, #34399, .T. ) ;
#18948 = CARTESIAN_POINT ( 'NONE',  ( -21.52205650746854815, 4.298041411267772283, -21.99797594555649383 ) ) ;
#18949 = DIRECTION ( 'NONE',  ( 1.000000000000000000, 0.000000000000000000, 0.000000000000000000 ) ) ;
#18950 = CARTESIAN_POINT ( 'NONE',  ( 5.383930013064285092, 36.46347792550310629, 10.49999999999999467 ) ) ;
#18951 = LINE ( 'NONE', #30949, #22633 ) ;
#18952 = EDGE_CURVE ( 'NONE', #37992, #2950, #5124, .T. ) ;
#18953 = AXIS2_PLACEMENT_3D ( 'NONE', #5209, #29992, #17621 ) ;
#18954 = CARTESIAN_POINT ( 'NONE',  ( -11.44473057578096764, 31.45924896672619298, 10.49999999999999822 ) ) ;
#18955 = PRODUCT_RELATED_PRODUCT_CATEGORY ( 'part', '', ( #37908 ) ) ;
#18956 = CIRCLE ( 'NONE', #34539, 1.000000000000000000 ) ;
#18957 = CARTESIAN_POINT ( 'NONE',  ( -4.096822963000304796, 8.035697679810704486, 10.49999999999999822 ) ) ;
#18958 = EDGE_CURVE ( 'NONE', #7705, #33301, #20713, .T. ) ;
#18959 = DIRECTION ( 'NONE',  ( -0.6691306063588569053, 0.7431448254773954654, 0.000000000000000000 ) ) ;
#18960 = CARTESIAN_POINT ( 'NONE',  ( -19.76188599801438173, 5.707498807444228106, -28.24951685685252656 ) ) ;
#18961 = DIRECTION ( 'NONE',  ( 0.000000000000000000, 0.000000000000000000, 1.000000000000000000 ) ) ;
#18962 = EDGE_CURVE ( 'NONE', #29758, #20580, #4831, .T. ) ;
#18963 = CARTESIAN_POINT ( 'NONE',  ( 19.41504592165321696, -20.20693249214978238, -16.82202162988696514 ) ) ;
#18964 = CARTESIAN_POINT ( 'NONE',  ( 19.26948696230199687, 27.85601271560034675, 23.00000000000000000 ) ) ;
#18965 = CARTESIAN_POINT ( 'NONE',  ( 10.94815433824005169, 17.73468434523852721, -26.81376961522255087 ) ) ;
#18966 = ORIENTED_EDGE ( 'NONE', *, *, #5317, .T. ) ;
#18967 = CARTESIAN_POINT ( 'NONE',  ( -15.96668161688104703, 24.53857560187668696, -6.893541485189635942 ) ) ;
#18968 = CIRCLE ( 'NONE', #23499, 0.5000000000000004441 ) ;
#18969 = CARTESIAN_POINT ( 'NONE',  ( -29.32420241873618494, -10.00128497722950804, 20.25080042701566541 ) ) ;
#18970 = CARTESIAN_POINT ( 'NONE',  ( -7.917741276437941345, 30.52956727630665057, 6.000000000000000000 ) ) ;
#18971 = CARTESIAN_POINT ( 'NONE',  ( 11.02183263331336072, 17.28494426090127334, -30.00000000000000000 ) ) ;
#18972 = ORIENTED_EDGE ( 'NONE', *, *, #34599, .F. ) ;
#18973 = LINE ( 'NONE', #9637, #3436 ) ;
#18974 = VERTEX_POINT ( 'NONE', #1790 ) ;
#18976 = PLANE ( 'NONE',  #34161 ) ;
#18975 = CARTESIAN_POINT ( 'NONE',  ( -15.09256969434682460, 26.55329248168451883, -8.287362166344871994 ) ) ;
#18977 = CARTESIAN_POINT ( 'NONE',  ( -9.607720528598306942, -18.16065568266596841, -28.70352573344614910 ) ) ;
#18978 = FACE_OUTER_BOUND ( 'NONE', #9982, .T. ) ;
#18979 = ORIENTED_EDGE ( 'NONE', *, *, #19410, .T. ) ;
#18980 = CARTESIAN_POINT ( 'NONE',  ( -19.27656959047015306, -9.383399175354611543, -25.58674328688679722 ) ) ;
#18981 = CARTESIAN_POINT ( 'NONE',  ( -11.92233111337420048, -22.55166628322649558, -16.49877645844951246 ) ) ;
#18982 = FACE_OUTER_BOUND ( 'NONE', #29336, .T. ) ;
#18983 = CARTESIAN_POINT ( 'NONE',  ( 12.56326696322676639, 16.68910371357088351, -26.36019947833989718 ) ) ;
#18984 = VERTEX_POINT ( 'NONE', #32677 ) ;
#18985 = CARTESIAN_POINT ( 'NONE',  ( 22.21757360568209094, 4.531282118560625349, -19.88525668396988877 ) ) ;
#18986 = CARTESIAN_POINT ( 'NONE',  ( 8.744117900323281845, 12.16605582823063614, 9.500000000000000000 ) ) ;
#18987 = EDGE_CURVE ( 'NONE', #9209, #10038, #21364, .T. ) ;
#18988 = LINE ( 'NONE', #34432, #16672 ) ;
#18989 = EDGE_CURVE ( 'NONE', #26812, #11440, #33484, .T. ) ;
#18990 = CARTESIAN_POINT ( 'NONE',  ( -12.11431921993760952, -16.53859995959433604, -28.58492679012440618 ) ) ;
#18991 = ORIENTED_EDGE ( 'NONE', *, *, #18262, .T. ) ;
#18992 = CARTESIAN_POINT ( 'NONE',  ( -20.64150323923506747, 0.1775972471279622378, -28.04374465433520314 ) ) ;
#18993 = CARTESIAN_POINT ( 'NONE',  ( 30.67384541073807114, -0.3508467513185977715, -8.280288242715185376 ) ) ;
#18994 = CIRCLE ( 'NONE', #34562, 1.000000000000000888 ) ;
#18995 = CARTESIAN_POINT ( 'NONE',  ( 19.07517029984344958, -22.84232114558952276, 19.66345542862526230 ) ) ;
#18996 = VERTEX_POINT ( 'NONE', #36119 ) ;
#18997 = CARTESIAN_POINT ( 'NONE',  ( 2.168404344971008868E-14, -26.63027081345975589, -4.999999999999999112 ) ) ;
#18998 = FACE_OUTER_BOUND ( 'NONE', #17143, .T. ) ;
#18999 = ORIENTED_EDGE ( 'NONE', *, *, #13876, .F. ) ;
#19000 = CARTESIAN_POINT ( 'NONE',  ( 10.03245514394483529, 31.53326318584457510, 7.000000000000000000 ) ) ;
#19001 = EDGE_CURVE ( 'NONE', #14160, #40031, #2592, .T. ) ;
#19002 = AXIS2_PLACEMENT_3D ( 'NONE', #27109, #36058, #8218 ) ;
#19003 = DIRECTION ( 'NONE',  ( 0.000000000000000000, 0.000000000000000000, 1.000000000000000000 ) ) ;
#19004 = CARTESIAN_POINT ( 'NONE',  ( 27.20167217099651680, 3.999461679709010564, -5.000000000000004441 ) ) ;
#19005 = CARTESIAN_POINT ( 'NONE',  ( 2.248380420413196301, 31.20224717405769965, -14.73880478081109224 ) ) ;
#19006 = DIRECTION ( 'NONE',  ( 1.000000000000000000, 0.000000000000000000, 0.000000000000000000 ) ) ;
#19007 = CARTESIAN_POINT ( 'NONE',  ( 14.31603901957230285, 19.98981538725070450, 10.49999999999999822 ) ) ;
#19008 = AXIS2_PLACEMENT_3D ( 'NONE', #31363, #9233, #15131 ) ;
#19009 = DIRECTION ( 'NONE',  ( 0.000000000000000000, 0.000000000000000000, 1.000000000000000000 ) ) ;
#19010 = CARTESIAN_POINT ( 'NONE',  ( -12.30736835487442882, 14.81698729810789672, 7.000000000000000000 ) ) ;
#19011 = DIRECTION ( 'NONE',  ( 0.000000000000000000, 0.000000000000000000, -1.000000000000000000 ) ) ;
#19012 = DIRECTION ( 'NONE',  ( 1.000000000000000000, 0.000000000000000000, 0.000000000000000000 ) ) ;
#19013 = CARTESIAN_POINT ( 'NONE',  ( 10.42368143308724093, 18.08059978384341449, -26.76484793057170819 ) ) ;
#19014 = CARTESIAN_POINT ( 'NONE',  ( -6.654030453887829211, 35.94335816374515247, 7.500000000000000888 ) ) ;
#19015 = ORIENTED_EDGE ( 'NONE', *, *, #7165, .T. ) ;
#19016 = CIRCLE ( 'NONE', #17732, 1.000000000000000000 ) ;
#19018 = CARTESIAN_POINT ( 'NONE',  ( 13.63581098909226874, 27.45627467658428955, 7.000000000000000000 ) ) ;
#19017 = CARTESIAN_POINT ( 'NONE',  ( -18.13727770824980823, 18.50383905080510161, -7.888881962196643727 ) ) ;
#19019 = CARTESIAN_POINT ( 'NONE',  ( 13.09742388243072320, 16.09289933416717489, 10.49999999999999822 ) ) ;
#19020 = CARTESIAN_POINT ( 'NONE',  ( 15.35224999201118301, -26.63338943820685145, -6.417067792862570563 ) ) ;
#19021 = CARTESIAN_POINT ( 'NONE',  ( -14.68365521139617513, -18.63605605981938496, -21.13871917996053540 ) ) ;
#19022 = CARTESIAN_POINT ( 'NONE',  ( 15.34221292749994703, 26.60361493431586410, -6.887934399220042359 ) ) ;
#19023 = CARTESIAN_POINT ( 'NONE',  ( 15.09678720978786792, 26.15351954639106680, -8.766955913214280471 ) ) ;
#19024 = ORIENTED_EDGE ( 'NONE', *, *, #2418, .T. ) ;
#19025 = DIRECTION ( 'NONE',  ( -1.000000000000000000, 0.000000000000000000, 0.000000000000000000 ) ) ;
#19026 = CARTESIAN_POINT ( 'NONE',  ( -12.18907228018264988, -22.02585773758839593, -17.44635340709443128 ) ) ;
#19027 = CONICAL_SURFACE ( 'NONE', #14565, 1.000000000000002665, 0.7853981633974530530 ) ;
#19028 = CARTESIAN_POINT ( 'NONE',  ( -36.90241796781145922, -7.097865958168809719, 12.73282698324792328 ) ) ;
#19029 = CARTESIAN_POINT ( 'NONE',  ( -17.27544398881353516, -12.67674546857244167, -25.60352082169515242 ) ) ;
#19030 = AXIS2_PLACEMENT_3D ( 'NONE', #39140, #23504, #36502 ) ;
#19031 = CARTESIAN_POINT ( 'NONE',  ( -4.648451212885357009, -24.43533398093167364, -9.867068457485020261 ) ) ;
#19032 = CARTESIAN_POINT ( 'NONE',  ( 11.33961468246317139, 17.07831742606941461, -29.35587556166173684 ) ) ;
#19033 = ORIENTED_EDGE ( 'NONE', *, *, #21986, .T. ) ;
#19034 = CARTESIAN_POINT ( 'NONE',  ( 18.89829205095695031, 8.796968066745694870, -25.49925083140837501 ) ) ;
#19035 = CARTESIAN_POINT ( 'NONE',  ( 6.176557290856084848, -13.77684855175925804, 22.99999999999999289 ) ) ;
#19036 = CARTESIAN_POINT ( 'NONE',  ( -1.350289120986974551E-13, 38.03812643383474779, 16.87380292611441490 ) ) ;
#19037 = ORIENTED_EDGE ( 'NONE', *, *, #20767, .T. ) ;
#19038 = CARTESIAN_POINT ( 'NONE',  ( -25.85780729842050008, -3.254098561623225194, -18.03984462349898266 ) ) ;
#19039 = EDGE_CURVE ( 'NONE', #17047, #28626, #36285, .T. ) ;
#19040 = AXIS2_PLACEMENT_3D ( 'NONE', #3420, #9528, #15816 ) ;
#19041 = CARTESIAN_POINT ( 'NONE',  ( -15.85745926894755620, 21.40218184478837316, 17.42190598798787349 ) ) ;
#19042 = EDGE_LOOP ( 'NONE', ( #23131, #16471, #10033, #16268 ) ) ;
#19043 = DIRECTION ( 'NONE',  ( 0.000000000000000000, -0.6729908358753945441, 0.7396508195275239839 ) ) ;
#19044 = CARTESIAN_POINT ( 'NONE',  ( -14.33346043011695414, 20.15556903647894416, 10.66666666666666252 ) ) ;
#19045 = CARTESIAN_POINT ( 'NONE',  ( -30.01474851606876726, 0.8478221152901143087, -5.946541633344167188 ) ) ;
#19046 = CARTESIAN_POINT ( 'NONE',  ( 34.71864531128215248, -13.96902139200064852, -7.560095839640886162 ) ) ;
#19047 = CARTESIAN_POINT ( 'NONE',  ( 32.09165771328279959, 1.123514972295850178, 13.32518128616608877 ) ) ;
#19048 = CONICAL_SURFACE ( 'NONE', #20368, 0.4999999999999980571, 0.7853981633974548293 ) ;
#19049 = VERTEX_POINT ( 'NONE', #5626 ) ;
#19050 = VERTEX_POINT ( 'NONE', #14976 ) ;
#19051 = DIRECTION ( 'NONE',  ( 0.000000000000000000, 0.000000000000000000, 1.000000000000000000 ) ) ;
#19052 = DIRECTION ( 'NONE',  ( 0.000000000000000000, 0.000000000000000000, 1.000000000000000000 ) ) ;
#19053 = EDGE_CURVE ( 'NONE', #24243, #16522, #25244, .T. ) ;
#19054 = DIRECTION ( 'NONE',  ( 1.000000000000000000, 0.000000000000000000, 0.000000000000000000 ) ) ;
#19055 = ORIENTED_EDGE ( 'NONE', *, *, #11014, .T. ) ;
#19056 = CIRCLE ( 'NONE', #6712, 0.5000000000000004441 ) ;
#19057 = ADVANCED_FACE ( 'NONE', ( #27365 ), #32877, .T. ) ;
#19058 = CARTESIAN_POINT ( 'NONE',  ( -1.963563434085775716, 24.56407772697490088, -20.71148629140979125 ) ) ;
#19059 = DIRECTION ( 'NONE',  ( 1.000000000000000000, 0.000000000000000000, 0.000000000000000000 ) ) ;
#19060 = LINE ( 'NONE', #769, #5283 ) ;
#19061 = DIRECTION ( 'NONE',  ( 0.000000000000000000, 0.000000000000000000, 1.000000000000000000 ) ) ;
#19062 = CARTESIAN_POINT ( 'NONE',  ( -7.301172712743408511, 30.08322998587614805, 10.74999999999999467 ) ) ;
#19063 = CARTESIAN_POINT ( 'NONE',  ( -33.75875814100324845, 2.759858869446484064, 11.00000000000000000 ) ) ;
#19064 = CIRCLE ( 'NONE', #1560, 15.00000000000000000 ) ;
#19065 = CARTESIAN_POINT ( 'NONE',  ( 8.342340113773577315, 19.48526559538274228, -25.93911266913574920 ) ) ;
#19066 = EDGE_LOOP ( 'NONE', ( #24597, #8249, #21923 ) ) ;
#19067 = EDGE_CURVE ( 'NONE', #22041, #23547, #10939, .T. ) ;
#19068 = CARTESIAN_POINT ( 'NONE',  ( -20.15622055155539272, 12.04428324321301425, -13.90711018673853872 ) ) ;
#19069 = CARTESIAN_POINT ( 'NONE',  ( 5.440908595777815826, 35.94977745735560859, 9.500000000000000000 ) ) ;
#19070 = CARTESIAN_POINT ( 'NONE',  ( 15.43512952755564349, -26.60538963749703356, -6.886851144620130150 ) ) ;
#19071 = CARTESIAN_POINT ( 'NONE',  ( -14.97009266215794021, 21.42933399866948463, 10.49999999999999822 ) ) ;
#19072 = CARTESIAN_POINT ( 'NONE',  ( 11.02889904915459063, 17.53211054968905813, -27.44436270301952163 ) ) ;
#19073 = CARTESIAN_POINT ( 'NONE',  ( -31.47283671532259675, -25.12609584734821411, -5.000000000000010658 ) ) ;
#19074 = AXIS2_PLACEMENT_3D ( 'NONE', #9856, #2969, #37690 ) ;
#19075 = CARTESIAN_POINT ( 'NONE',  ( -18.50717619730081864, -19.59423608300353692, -17.82256473852398670 ) ) ;
#19076 = CARTESIAN_POINT ( 'NONE',  ( 8.329568172293271289, -18.84798106794158201, -28.13937053122434051 ) ) ;
#19077 = CARTESIAN_POINT ( 'NONE',  ( 15.29674875102894482, 26.18853547279510607, -7.828964019014474474 ) ) ;
#19078 = CARTESIAN_POINT ( 'NONE',  ( 17.19085919694937203, -11.61334556840082399, -27.71234399686709438 ) ) ;
#19079 = CARTESIAN_POINT ( 'NONE',  ( 13.90768907780713270, 27.88359266870271824, 10.49999999999999822 ) ) ;
#19080 = CARTESIAN_POINT ( 'NONE',  ( 11.33320880805461606, 31.58310643763893211, 10.66666666666666607 ) ) ;
#19081 = ORIENTED_EDGE ( 'NONE', *, *, #10096, .F. ) ;
#19082 = CARTESIAN_POINT ( 'NONE',  ( -5.372192365448402285, 20.15702040454593913, -27.08516113732625641 ) ) ;
#19083 = EDGE_CURVE ( 'NONE', #23843, #32713, #32400, .T. ) ;
#19084 = CARTESIAN_POINT ( 'NONE',  ( 8.315274455032101386, 10.01576150750513250, 7.500000000000000888 ) ) ;
#19085 = EDGE_CURVE ( 'NONE', #12591, #31473, #7049, .T. ) ;
#19086 = AXIS2_PLACEMENT_3D ( 'NONE', #17330, #1275, #29305 ) ;
#19087 = DIRECTION ( 'NONE',  ( 1.000000000000000000, 0.000000000000000000, 0.000000000000000000 ) ) ;
#19088 = ORIENTED_EDGE ( 'NONE', *, *, #19083, .F. ) ;
#19089 = CARTESIAN_POINT ( 'NONE',  ( 30.65562841553949625, -0.05914043160616395262, -7.356430913030059138 ) ) ;
#19090 = CARTESIAN_POINT ( 'NONE',  ( -14.22382948751887177, 26.07014013211518133, 10.49999999999999645 ) ) ;
#19091 = LINE ( 'NONE', #3649, #3092 ) ;
#19092 = ORIENTED_EDGE ( 'NONE', *, *, #33302, .F. ) ;
#19093 = CARTESIAN_POINT ( 'NONE',  ( -29.31499521850481216, 0.1194913391831431554, -10.65473379611367655 ) ) ;
#19094 = CARTESIAN_POINT ( 'NONE',  ( -19.71199081357663729, -26.17691209550672937, -9.501020233452134534 ) ) ;
#19095 = VERTEX_POINT ( 'NONE', #3376 ) ;
#19096 = CARTESIAN_POINT ( 'NONE',  ( 21.98133561711489392, -4.524757649539990823, -23.29269831984457184 ) ) ;
#19097 = AXIS2_PLACEMENT_3D ( 'NONE', #36013, #8173, #17737 ) ;
#19098 = VERTEX_POINT ( 'NONE', #9686 ) ;
#19099 = CARTESIAN_POINT ( 'NONE',  ( -1.911335737650684097, 40.16401087634231004, 13.32518128616608521 ) ) ;
#19100 = FACE_OUTER_BOUND ( 'NONE', #34740, .T. ) ;
#19101 = CARTESIAN_POINT ( 'NONE',  ( -3.503793317224517700, 8.420815634768727520, 7.000000000000000000 ) ) ;
#19102 = EDGE_CURVE ( 'NONE', #38835, #29659, #12524, .T. ) ;
#19103 = CARTESIAN_POINT ( 'NONE',  ( 10.16357496796713100, 29.39421982382241438, 19.27171037444158230 ) ) ;
#19104 = AXIS2_PLACEMENT_3D ( 'NONE', #17728, #19595, #11421 ) ;
#19105 = FACE_OUTER_BOUND ( 'NONE', #33950, .T. ) ;
#19106 = ORIENTED_EDGE ( 'NONE', *, *, #35598, .T. ) ;
#19107 = EDGE_CURVE ( 'NONE', #31085, #34024, #7079, .T. ) ;
#19108 = DIRECTION ( 'NONE',  ( 1.000000000000000000, 0.000000000000000000, 0.000000000000000000 ) ) ;
#19109 = CARTESIAN_POINT ( 'NONE',  ( 1.087821238877949126, 20.47389780075598509, -30.00000000000000711 ) ) ;
#19110 = DIRECTION ( 'NONE',  ( 0.000000000000000000, 0.000000000000000000, 1.000000000000000000 ) ) ;
#19111 = DIRECTION ( 'NONE',  ( 0.5877852522924689183, -0.8090169943749503378, 0.000000000000000000 ) ) ;
#19112 = CARTESIAN_POINT ( 'NONE',  ( 17.57104634348523220, 19.83623530875129148, -7.877413894578867648 ) ) ;
#19113 = CARTESIAN_POINT ( 'NONE',  ( 4.967200795408929004, 22.09671430245085944, -23.13287681390427863 ) ) ;
#19114 = ORIENTED_EDGE ( 'NONE', *, *, #37687, .T. ) ;
#19115 = CARTESIAN_POINT ( 'NONE',  ( 10.16493647378288934, -17.96286526707443798, -28.04375298610375111 ) ) ;
#19116 = DIRECTION ( 'NONE',  ( 1.000000000000000000, 0.000000000000000000, 0.000000000000000000 ) ) ;
#19117 = CARTESIAN_POINT ( 'NONE',  ( 14.47283171447379146, 21.48159823030311344, 7.000000000000000000 ) ) ;
#19118 = VECTOR ( 'NONE', #28657, 1000.000000000000114 ) ;
#19119 = ORIENTED_EDGE ( 'NONE', *, *, #37352, .F. ) ;
#19120 = CARTESIAN_POINT ( 'NONE',  ( -14.74829102090526511, 25.36468816584346087, -10.65391712686787073 ) ) ;
#19121 = CARTESIAN_POINT ( 'NONE',  ( -32.40618899211658288, -4.990034233202359282, 17.92354375535250810 ) ) ;
#19122 = CARTESIAN_POINT ( 'NONE',  ( 14.94022447862385405, -26.11394648050683998, -8.769034538900596587 ) ) ;
#19123 = LINE ( 'NONE', #19521, #25041 ) ;
#19124 = EDGE_LOOP ( 'NONE', ( #418, #24937, #16675, #2863 ) ) ;
#19125 = EDGE_LOOP ( 'NONE', ( #5757, #36850, #38874, #2597 ) ) ;
#19126 = CARTESIAN_POINT ( 'NONE',  ( -12.20352377363692575, 22.79644703365081071, -17.28398000730053141 ) ) ;
#19127 = AXIS2_PLACEMENT_3D ( 'NONE', #39749, #23917, #2779 ) ;
#19128 = CARTESIAN_POINT ( 'NONE',  ( -12.15296444596746639, -16.58779297045509438, -28.59925402683893836 ) ) ;
#19129 = FACE_BOUND ( 'NONE', #5330, .T. ) ;
#19130 = VECTOR ( 'NONE', #27604, 1000.000000000000114 ) ;
#19131 = CARTESIAN_POINT ( 'NONE',  ( -20.30734916839453774, -5.667360972306529021, -26.38649982237350144 ) ) ;
#19132 = CARTESIAN_POINT ( 'NONE',  ( -9.488776258477622960, -18.31424688356152330, -28.08193020798964668 ) ) ;
#19133 = CARTESIAN_POINT ( 'NONE',  ( -3.607749162633401507, 7.931741834401821123, 7.000000000000000000 ) ) ;
#19134 = ORIENTED_EDGE ( 'NONE', *, *, #33510, .T. ) ;
#19135 = CARTESIAN_POINT ( 'NONE',  ( 29.99944291653464035, 0.2112700481506303019, -8.770229588436221135 ) ) ;
#19136 = CARTESIAN_POINT ( 'NONE',  ( 10.98647152987756748, 17.30743896080529609, -28.69679681820503347 ) ) ;
#19137 = DIRECTION ( 'NONE',  ( 0.9135454576425988682, -0.4067366430758048157, 3.469446951953606300E-15 ) ) ;
#19138 = EDGE_CURVE ( 'NONE', #34728, #18136, #2985, .T. ) ;
#19139 = EDGE_LOOP ( 'NONE', ( #282, #18214, #17286, #1397 ) ) ;
#19140 = CARTESIAN_POINT ( 'NONE',  ( -29.85246077738104731, -0.01121920330367918127, -9.705672615991840502 ) ) ;
#19141 = ORIENTED_EDGE ( 'NONE', *, *, #20727, .T. ) ;
#19142 = CARTESIAN_POINT ( 'NONE',  ( 30.98664919647288940, -1.692235243981042858, -10.06380571118922518 ) ) ;
#19143 = CARTESIAN_POINT ( 'NONE',  ( 20.92112759555548251, -16.07000418475261583, 20.99999999999999645 ) ) ;
#19144 = CARTESIAN_POINT ( 'NONE',  ( 32.94198380406537296, -19.01906321691718205, 16.87380292611441490 ) ) ;
#19145 = VERTEX_POINT ( 'NONE', #6609 ) ;
#19146 = CARTESIAN_POINT ( 'NONE',  ( -11.81630298851966288, 31.79381426990562787, 10.49999999999999822 ) ) ;
#19147 = VECTOR ( 'NONE', #7126, 999.9999999999998863 ) ;
#19148 = CARTESIAN_POINT ( 'NONE',  ( -3.003889247184246880, 27.48891118973640602, 20.99999999999988987 ) ) ;
#19149 = CARTESIAN_POINT ( 'NONE',  ( -11.44134295108998955, 15.31698729810788961, 9.500000000000000000 ) ) ;
#19150 = LINE ( 'NONE', #31544, #1344 ) ;
#19151 = CIRCLE ( 'NONE', #24354, 0.5000000000000000000 ) ;
#19152 = VECTOR ( 'NONE', #7534, 1000.000000000000000 ) ;
#19153 = CARTESIAN_POINT ( 'NONE',  ( -11.44169217588621201, 32.12932954397595608, 10.76099332938163933 ) ) ;
#19154 = CARTESIAN_POINT ( 'NONE',  ( 25.71480618106328109, 9.014447550977328305, 11.55979286844026532 ) ) ;
#19155 = CARTESIAN_POINT ( 'NONE',  ( -22.95459534405085122, 9.880914000425169874, -5.965707660850015692 ) ) ;
#19156 = CARTESIAN_POINT ( 'NONE',  ( 14.59364668521135755, -15.19212837545807382, -26.41884767242281384 ) ) ;
#19157 = DIRECTION ( 'NONE',  ( 0.000000000000000000, 0.000000000000000000, 1.000000000000000000 ) ) ;
#19158 = CARTESIAN_POINT ( 'NONE',  ( 14.87809943308360339, 25.97911021677501608, -9.699071928801664910 ) ) ;
#19159 = ORIENTED_EDGE ( 'NONE', *, *, #37728, .T. ) ;
#19160 = CARTESIAN_POINT ( 'NONE',  ( -15.56594212721577541, 25.60277546647914448, -7.361410068878811330 ) ) ;
#19161 = CARTESIAN_POINT ( 'NONE',  ( -22.33353841799275941, -20.81031336111065144, 20.25080042701592120 ) ) ;
#19162 = CARTESIAN_POINT ( 'NONE',  ( 4.524139159579314118, 31.43208625488810171, 10.49999999999999822 ) ) ;
#19163 = CARTESIAN_POINT ( 'NONE',  ( 15.12327263463977722, 26.06678387642238448, -8.768336635076099839 ) ) ;
#19164 = EDGE_LOOP ( 'NONE', ( #37854, #28284 ) ) ;
#19165 = FACE_OUTER_BOUND ( 'NONE', #10540, .T. ) ;
#19166 = EDGE_LOOP ( 'NONE', ( #7217, #26688, #20701, #776, #38916, #26219, #313 ) ) ;
#19168 = DIRECTION ( 'NONE',  ( 1.000000000000000000, 0.000000000000000000, 0.000000000000000000 ) ) ;
#19167 = CARTESIAN_POINT ( 'NONE',  ( -14.75774405092634645, 25.86145994709132978, -10.16509986974211976 ) ) ;
#19169 = CARTESIAN_POINT ( 'NONE',  ( -9.543759016413366325, -18.14299990126706419, -29.34740481499151343 ) ) ;
#19170 = PLANE ( 'NONE',  #39257 ) ;
#19171 = ORIENTED_EDGE ( 'NONE', *, *, #11126, .F. ) ;
#19172 = CARTESIAN_POINT ( 'NONE',  ( -25.74471773230272476, -13.48393985794896111, -16.62992022540315062 ) ) ;
#19173 = CARTESIAN_POINT ( 'NONE',  ( -13.68829447021390422, -25.58996436347754866, -9.727192414191598857 ) ) ;
#19174 = CYLINDRICAL_SURFACE ( 'NONE', #10521, 57.00000000000006395 ) ;
#19175 = CARTESIAN_POINT ( 'NONE',  ( 16.87377372029358469, 22.19217076240406428, -5.000000000000004441 ) ) ;
#19176 = EDGE_LOOP ( 'NONE', ( #5566, #7970, #8141, #4646 ) ) ;
#19177 = CARTESIAN_POINT ( 'NONE',  ( 23.39580328310244894, 5.396513899929180624, -15.78908983431174740 ) ) ;
#19178 = ADVANCED_FACE ( 'NONE', ( #22063 ), #36914, .F. ) ;
#19179 = DIRECTION ( 'NONE',  ( 1.000000000000000000, 0.000000000000000000, 0.000000000000000000 ) ) ;
#19180 = FACE_OUTER_BOUND ( 'NONE', #15080, .T. ) ;
#19181 = FACE_OUTER_BOUND ( 'NONE', #14448, .T. ) ;
#19182 = B_SPLINE_CURVE_WITH_KNOTS ( 'NONE', 3,
 ( #15169, #36907, #18030, #40145, #21071, #12123 ),
 .UNSPECIFIED., .F., .F.,
 ( 4, 2, 4 ),
 ( 0.000000000000000000, 0.5000000000000000000, 1.000000000000000000 ),
 .UNSPECIFIED. ) ;
#19183 = CIRCLE ( 'NONE', #11423, 1.000000000000000000 ) ;
#19184 = ORIENTED_EDGE ( 'NONE', *, *, #36222, .F. ) ;
#19185 = CARTESIAN_POINT ( 'NONE',  ( -26.97206810645275255, -0.4441396946580338789, -15.36407590373037912 ) ) ;
#19186 = CARTESIAN_POINT ( 'NONE',  ( 24.03547544862108154, 0.2628772248198613104, -19.46575558521258387 ) ) ;
#19187 = AXIS2_PLACEMENT_3D ( 'NONE', #23857, #24060, #33424 ) ;
#19188 = VECTOR ( 'NONE', #30675, 1000.000000000000000 ) ;
#19189 = EDGE_CURVE ( 'NONE', #29941, #35073, #3576, .T. ) ;
#19190 = CARTESIAN_POINT ( 'NONE',  ( 29.14609120334211667, -6.569533100115761748, 19.99202127657103389 ) ) ;
#19191 = ORIENTED_EDGE ( 'NONE', *, *, #11017, .F. ) ;
#19192 = EDGE_CURVE ( 'NONE', #15391, #16334, #3841, .T. ) ;
#19193 = CARTESIAN_POINT ( 'NONE',  ( 5.636483973512839363, -22.01575377102105691, -30.00000000000001421 ) ) ;
#19194 = LINE ( 'NONE', #7601, #24498 ) ;
#19195 = ORIENTED_EDGE ( 'NONE', *, *, #38386, .T. ) ;
#19196 = CARTESIAN_POINT ( 'NONE',  ( -6.348113209407908464, 9.835177808069893501, 6.000000000000000000 ) ) ;
#19197 = CYLINDRICAL_SURFACE ( 'NONE', #25303, 1.000000000000000888 ) ;
#19198 = CARTESIAN_POINT ( 'NONE',  ( 8.401171878996485987, 21.11424711454080594, 9.000000000000001776 ) ) ;
#19199 = CARTESIAN_POINT ( 'NONE',  ( 2.752814969234745668, 20.95510515482600056, -26.29072956667404171 ) ) ;
#19200 = CARTESIAN_POINT ( 'NONE',  ( -9.941034666242671847, 32.57396620494226624, 7.500000000000004441 ) ) ;
#19201 = EDGE_CURVE ( 'NONE', #37486, #33852, #13552, .T. ) ;
#19202 = CARTESIAN_POINT ( 'NONE',  ( 10.41267482483262619, 26.20820393249957192, 13.00000000000000178 ) ) ;
#19203 = EDGE_CURVE ( 'NONE', #2935, #13994, #1922, .T. ) ;
#19204 = DIRECTION ( 'NONE',  ( -0.8660254037844432595, -0.4999999999999921729, 0.000000000000000000 ) ) ;
#19205 = DIRECTION ( 'NONE',  ( 0.1045284632676570929, 0.9945218953682730678, 0.000000000000000000 ) ) ;
#19206 = CARTESIAN_POINT ( 'NONE',  ( -6.312041872459064784, 25.58773265502866678, 6.000000000000000000 ) ) ;
#19207 = DIRECTION ( 'NONE',  ( 1.000000000000000000, 0.000000000000000000, 0.000000000000000000 ) ) ;
#19208 = CARTESIAN_POINT ( 'NONE',  ( 15.09735744684384962, 27.15937815847784620, -7.340727882394975978 ) ) ;
#19209 = DIRECTION ( 'NONE',  ( 0.9781476007338067991, 0.2079116908177533474, 0.000000000000000000 ) ) ;
#19210 = ORIENTED_EDGE ( 'NONE', *, *, #29777, .T. ) ;
#19213 = DIRECTION ( 'NONE',  ( -0.000000000000000000, 0.000000000000000000, 1.000000000000000000 ) ) ;
#19212 = AXIS2_PLACEMENT_3D ( 'NONE', #12283, #22020, #6569 ) ;
#19211 = CARTESIAN_POINT ( 'NONE',  ( -17.44085994297563147, 17.55310934480021956, -12.80343249213678547 ) ) ;
#19214 = CARTESIAN_POINT ( 'NONE',  ( 37.51589702892714939, -12.89337557385784550, 11.00000000000017408 ) ) ;
#19215 = CARTESIAN_POINT ( 'NONE',  ( 15.42968591400663847, -26.70185147947299598, -5.946084178125359720 ) ) ;
#19216 = CARTESIAN_POINT ( 'NONE',  ( 17.00000000000000000, 22.50000000000000711, 10.00000000000000000 ) ) ;
#19217 = CARTESIAN_POINT ( 'NONE',  ( 15.10684921377551326, 26.12025004395372818, -8.767816402119800401 ) ) ;
#19218 = ORIENTED_EDGE ( 'NONE', *, *, #35969, .T. ) ;
#19219 = CARTESIAN_POINT ( 'NONE',  ( 15.01137483442351517, 25.99107282686816234, -9.237182367602107647 ) ) ;
#19220 = VERTEX_POINT ( 'NONE', #15573 ) ;
#19221 = CARTESIAN_POINT ( 'NONE',  ( 3.531008893910514868, 8.292776413244014933, 11.00000000000000000 ) ) ;
#19222 = CARTESIAN_POINT ( 'NONE',  ( -10.15894275696289917, -19.18740761933786843, -23.86200704285396768 ) ) ;
#19223 = CARTESIAN_POINT ( 'NONE',  ( -33.64699323788562424, -0.06984207429672421863, 12.14047268033065485 ) ) ;
#19224 = CARTESIAN_POINT ( 'NONE',  ( -28.27972534383151526, -19.54013907706369935, -11.98161375967031717 ) ) ;
#19225 = CARTESIAN_POINT ( 'NONE',  ( -4.747314164036073869, -24.73656458911068512, -7.904840398386835609 ) ) ;
#19226 = CARTESIAN_POINT ( 'NONE',  ( 11.88480245227968091, 18.08769387689092412, -23.91349747340691678 ) ) ;
#19227 = ORIENTED_EDGE ( 'NONE', *, *, #3800, .F. ) ;
#19228 = CARTESIAN_POINT ( 'NONE',  ( 20.78437466676830780, 10.47168160296281769, -14.91585341470220349 ) ) ;
#19229 = CARTESIAN_POINT ( 'NONE',  ( 1.278175571583998194, 14.08178954835375940, 9.000000000000001776 ) ) ;
#19230 = CARTESIAN_POINT ( 'NONE',  ( 12.40052356344507523, 30.91160080447357927, 17.42190598798393353 ) ) ;
#19231 = ORIENTED_EDGE ( 'NONE', *, *, #26619, .T. ) ;
#19232 = CARTESIAN_POINT ( 'NONE',  ( -29.68610188510462322, -2.963264296338544490, -13.23833758059748966 ) ) ;
#19233 = EDGE_CURVE ( 'NONE', #2021, #35146, #18825, .T. ) ;
#19234 = CARTESIAN_POINT ( 'NONE',  ( -15.87271492000489559, 26.91186955877756404, 15.72805884748939498 ) ) ;
#19235 = ORIENTED_EDGE ( 'NONE', *, *, #24665, .F. ) ;
#19236 = CARTESIAN_POINT ( 'NONE',  ( 12.30736835487433112, 14.81698729810772797, 11.00000000000000000 ) ) ;
#19237 = DIRECTION ( 'NONE',  ( -0.6691306063588670083, -0.7431448254773863615, 0.000000000000000000 ) ) ;
#19238 = CARTESIAN_POINT ( 'NONE',  ( -20.56034067317128944, 1.524475442768058020, -28.10962306186307913 ) ) ;
#19239 = CARTESIAN_POINT ( 'NONE',  ( 34.42547319207020706, -15.07984268493967051, -7.554536495709903932 ) ) ;
#19240 = CARTESIAN_POINT ( 'NONE',  ( 35.68447701591249910, -3.401722300707781255, 11.55979286843934872 ) ) ;
#19241 = AXIS2_PLACEMENT_3D ( 'NONE', #7783, #32582, #11047 ) ;
#19242 = ORIENTED_EDGE ( 'NONE', *, *, #1102, .T. ) ;
#19243 = VERTEX_POINT ( 'NONE', #39753 ) ;
#19244 = FACE_OUTER_BOUND ( 'NONE', #3506, .T. ) ;
#19245 = CARTESIAN_POINT ( 'NONE',  ( -1.000000000000000000, 37.00000000000000711, 10.50000000000000178 ) ) ;
#19246 = CARTESIAN_POINT ( 'NONE',  ( 5.622359283595903534, 36.35732237484523921, 10.76099332938163933 ) ) ;
#19247 = ORIENTED_EDGE ( 'NONE', *, *, #24047, .F. ) ;
#19248 = CARTESIAN_POINT ( 'NONE',  ( -0.6412407266015724971, 32.46939045798620072, -13.80435559440418203 ) ) ;
#19249 = LINE ( 'NONE', #6264, #15251 ) ;
#19250 = DIRECTION ( 'NONE',  ( 1.000000000000000000, 3.469446951953611033E-15, 0.000000000000000000 ) ) ;
#19251 = EDGE_CURVE ( 'NONE', #23547, #39980, #37307, .T. ) ;
#19252 = DIRECTION ( 'NONE',  ( 0.9135454576426059736, 0.4067366430757888285, 0.000000000000000000 ) ) ;
#19253 = CARTESIAN_POINT ( 'NONE',  ( 15.35385137484828633, 7.606384166391536361, 10.00000000000000000 ) ) ;
#19254 = CARTESIAN_POINT ( 'NONE',  ( -10.53831209642071975, 32.66155519649347383, 11.00000000000000000 ) ) ;
#19255 = CARTESIAN_POINT ( 'NONE',  ( 11.69931679021635418, 27.94617659413938782, -13.18484883679364472 ) ) ;
#19256 = DIRECTION ( 'NONE',  ( 0.000000000000000000, 0.000000000000000000, 1.000000000000000000 ) ) ;
#19257 = EDGE_LOOP ( 'NONE', ( #28206, #6173, #18122, #39736 ) ) ;
#19259 = CARTESIAN_POINT ( 'NONE',  ( -12.05736835487443237, 14.38397459621567442, 10.50000000000000000 ) ) ;
#19258 = CARTESIAN_POINT ( 'NONE',  ( -19.02464814996286080, 10.35021103555779476, -21.17776305350152555 ) ) ;
#19260 = CARTESIAN_POINT ( 'NONE',  ( -12.30736835487442882, 14.81698729810789672, 7.499999999999993783 ) ) ;
#19261 = CARTESIAN_POINT ( 'NONE',  ( 11.59088340238572989, -20.97132811465274926, -19.49109192369429167 ) ) ;
#19262 = CARTESIAN_POINT ( 'NONE',  ( -6.706342468480190000, 20.64589803375067945, 13.00000000000000178 ) ) ;
#19263 = CARTESIAN_POINT ( 'NONE',  ( 10.96081938953363277, 17.37715277537162351, -28.70507073696821720 ) ) ;
#19264 = CARTESIAN_POINT ( 'NONE',  ( 17.81784622497951176, -13.85677843414110555, -19.80438750953540961 ) ) ;
#19265 = DIRECTION ( 'NONE',  ( -1.000000000000000000, 0.000000000000000000, 0.000000000000000000 ) ) ;
#19266 = AXIS2_PLACEMENT_3D ( 'NONE', #10905, #35686, #7841 ) ;
#19267 = TOROIDAL_SURFACE ( 'NONE', #27707, 1.000000000000000000, 0.5000000000000000000 ) ;
#19268 = CARTESIAN_POINT ( 'NONE',  ( -23.68773345865362856, -25.06554053738202015, -9.830582403723438389 ) ) ;
#19269 = CARTESIAN_POINT ( 'NONE',  ( 7.051063895666721315, -19.39164703839861659, -28.19631161156121735 ) ) ;
#19270 = CARTESIAN_POINT ( 'NONE',  ( 14.93246635580137038, 25.33278714524708164, -10.18550836669002990 ) ) ;
#19271 = CARTESIAN_POINT ( 'NONE',  ( 30.91129473722968157, -20.93446817436120000, -8.409707594405761100 ) ) ;
#19272 = CARTESIAN_POINT ( 'NONE',  ( 8.087160441415365497, 9.969847506822922867, 10.49999999999999822 ) ) ;
#19273 = CARTESIAN_POINT ( 'NONE',  ( 5.578816091646283226, 36.25952276447326739, 10.87262190629270364 ) ) ;
#19274 = VERTEX_POINT ( 'NONE', #37509 ) ;
#19275 = CARTESIAN_POINT ( 'NONE',  ( -5.279954849186515808, 19.80786611602342973, -29.99999999999998224 ) ) ;
#19276 = AXIS2_PLACEMENT_3D ( 'NONE', #25527, #38529, #16396 ) ;
#19277 = ADVANCED_FACE ( 'NONE', ( #18428 ), #24321, .F. ) ;
#19278 = AXIS2_PLACEMENT_3D ( 'NONE', #327, #31400, #12708 ) ;
#19279 = LINE ( 'NONE', #31477, #33853 ) ;
#19280 = VERTEX_POINT ( 'NONE', #21271 ) ;
#19281 = CARTESIAN_POINT ( 'NONE',  ( 21.27883545512939634, 0.7584189411604885800, -25.01272306973745074 ) ) ;
#19282 = EDGE_CURVE ( 'NONE', #26489, #36944, #11626, .T. ) ;
#19283 = DIRECTION ( 'NONE',  ( -0.000000000000000000, 0.000000000000000000, 1.000000000000000000 ) ) ;
#19284 = CARTESIAN_POINT ( 'NONE',  ( -25.38348611796302734, -5.460896781494596119, 20.69868183039781329 ) ) ;
#19285 = ORIENTED_EDGE ( 'NONE', *, *, #10616, .T. ) ;
#19286 = CARTESIAN_POINT ( 'NONE',  ( -30.03482762601120015, 0.1729744975902109405, -8.769734599055784230 ) ) ;
#19287 = PLANE ( 'NONE',  #11220 ) ;
#19288 = EDGE_LOOP ( 'NONE', ( #18732, #39496, #32247, #2624 ) ) ;
#19289 = CARTESIAN_POINT ( 'NONE',  ( 35.19752256302763271, -8.465509976530269043, -5.879991153137873461 ) ) ;
#19290 = ADVANCED_FACE ( 'NONE', ( #132 ), #6225, .T. ) ;
#19291 = EDGE_LOOP ( 'NONE', ( #34806, #30319, #35572 ) ) ;
#19292 = CARTESIAN_POINT ( 'NONE',  ( 14.89626057892310307, 32.60452476689641088, 11.55979286843934872 ) ) ;
#19293 = FACE_OUTER_BOUND ( 'NONE', #13486, .T. ) ;
#19294 = CARTESIAN_POINT ( 'NONE',  ( -0.9008293819426604898, 37.47308728914261877, 7.382773698552460573 ) ) ;
#19295 = CARTESIAN_POINT ( 'NONE',  ( 9.991741549994847205, 30.98179641005372886, 18.87996532025785967 ) ) ;
#19296 = AXIS2_PLACEMENT_3D ( 'NONE', #5154, #18156, #17560 ) ;
#19297 = VECTOR ( 'NONE', #39327, 999.9999999999998863 ) ;
#19298 = CARTESIAN_POINT ( 'NONE',  ( -9.941034666242673623, 32.57396620494226624, 9.500000000000000000 ) ) ;
#19299 = ORIENTED_EDGE ( 'NONE', *, *, #3347, .F. ) ;
#19300 = CARTESIAN_POINT ( 'NONE',  ( 0.9999966292907466192, 22.50000000000031264, 6.000000000000000000 ) ) ;
#19301 = CARTESIAN_POINT ( 'NONE',  ( 6.811226782241714517, 35.33967249274190436, 7.500000000000000888 ) ) ;
#19302 = DIRECTION ( 'NONE',  ( 1.000000000000000000, 0.000000000000000000, 0.000000000000000000 ) ) ;
#19303 = ADVANCED_FACE ( 'NONE', ( #30623 ), #5832, .T. ) ;
#19304 = CIRCLE ( 'NONE', #1807, 62.00000000000002132 ) ;
#19305 = EDGE_CURVE ( 'NONE', #37355, #11442, #39571, .T. ) ;
#19306 = EDGE_CURVE ( 'NONE', #7015, #6898, #34331, .T. ) ;
#19307 = CARTESIAN_POINT ( 'NONE',  ( 17.10940565685277193, 17.54728818196264584, -13.79989119490213767 ) ) ;
#19308 = VECTOR ( 'NONE', #32850, 999.9999999999998863 ) ;
#19309 = CARTESIAN_POINT ( 'NONE',  ( 10.02000509642858361, 34.97447782610390732, -5.444435539378085664 ) ) ;
#19310 = ORIENTED_EDGE ( 'NONE', *, *, #39075, .F. ) ;
#19311 = CARTESIAN_POINT ( 'NONE',  ( 15.94139939152667829, -26.45195379938700242, -8.269321208413121127 ) ) ;
#19312 = CARTESIAN_POINT ( 'NONE',  ( -6.354454053420243831, 35.54304081427989814, 7.000000000000000000 ) ) ;
#19313 = DIRECTION ( 'NONE',  ( 0.7431448254773961315, 0.6691306063588561281, 0.000000000000000000 ) ) ;
#19314 = VERTEX_POINT ( 'NONE', #8675 ) ;
#19315 = CARTESIAN_POINT ( 'NONE',  ( -15.10507689876119564, 26.12566811475226558, -8.768196822005435820 ) ) ;
#19316 = CARTESIAN_POINT ( 'NONE',  ( -34.71804043165838038, -14.31680059899250068, 16.87380292611441135 ) ) ;
#19317 = CARTESIAN_POINT ( 'NONE',  ( 11.95185560643699318, -22.03370127656497246, -17.46682300787701791 ) ) ;
#19318 = CYLINDRICAL_SURFACE ( 'NONE', #8841, 18.00000000000001421 ) ;
#19319 = EDGE_LOOP ( 'NONE', ( #32613, #8823 ) ) ;
#19320 = ORIENTED_EDGE ( 'NONE', *, *, #2821, .F. ) ;
#19321 = AXIS2_PLACEMENT_3D ( 'NONE', #6316, #12818, #34759 ) ;
#19322 = CARTESIAN_POINT ( 'NONE',  ( -12.64160356943281727, 29.64681118489703948, -10.41304400021260612 ) ) ;
#19323 = CARTESIAN_POINT ( 'NONE',  ( -13.59760056006964035, -18.39269960460429232, -22.34963270891807952 ) ) ;
#19324 = ADVANCED_FACE ( 'NONE', ( #5427 ), #18420, .F. ) ;
#19325 = FACE_BOUND ( 'NONE', #23659, .T. ) ;
#19326 = CIRCLE ( 'NONE', #38121, 1.000000000000000000 ) ;
#19327 = CIRCLE ( 'NONE', #36888, 1.000000000000000888 ) ;
#19328 = CARTESIAN_POINT ( 'NONE',  ( -34.55393062045996544, -7.546469469217721660, -7.629845520436306927 ) ) ;
#19329 = CARTESIAN_POINT ( 'NONE',  ( 6.762317648415093529, 29.93445088906596752, 10.50000000000000178 ) ) ;
#19330 = EDGE_LOOP ( 'NONE', ( #25992, #22485, #36176, #39062 ) ) ;
#19331 = CARTESIAN_POINT ( 'NONE',  ( 20.47688798105681940, 0.9740165025114795316, -30.00000000000000000 ) ) ;
#19332 = EDGE_CURVE ( 'NONE', #36663, #20274, #12258, .T. ) ;
#19333 = CARTESIAN_POINT ( 'NONE',  ( 13.64210930126480115, 24.20081211342298744, 6.000000000000000000 ) ) ;
#19334 = FACE_OUTER_BOUND ( 'NONE', #34022, .T. ) ;
#19335 = AXIS2_PLACEMENT_3D ( 'NONE', #23551, #8102, #20513 ) ;
#19336 = EDGE_LOOP ( 'NONE', ( #36620, #14881, #2631, #26389, #35733 ) ) ;
#19337 = CARTESIAN_POINT ( 'NONE',  ( -20.48364860518192998, 0.8189024673161406920, -29.34763341778235812 ) ) ;
#19338 = PLANE ( 'NONE',  #11187 ) ;
#19339 = ORIENTED_EDGE ( 'NONE', *, *, #33203, .T. ) ;
#19340 = CARTESIAN_POINT ( 'NONE',  ( 25.62407562875491962, -2.247368772962396122, -18.13072093081501279 ) ) ;
#19341 = CIRCLE ( 'NONE', #16097, 0.5000000000000004441 ) ;
#19342 = CARTESIAN_POINT ( 'NONE',  ( 15.20858617250272005, 13.81569066517950795, -30.00000000000002842 ) ) ;
#19343 = CARTESIAN_POINT ( 'NONE',  ( 22.28716212642845917, -26.62569406410656825, 16.87380292611434385 ) ) ;
#19344 = ORIENTED_EDGE ( 'NONE', *, *, #23942, .F. ) ;
#19345 = CARTESIAN_POINT ( 'NONE',  ( 8.747212233148117022, 37.02488667719009641, 15.13084544680216759 ) ) ;
#19346 = DIRECTION ( 'NONE',  ( 0.8660254037844363761, -0.5000000000000039968, -0.000000000000000000 ) ) ;
#19347 = CARTESIAN_POINT ( 'NONE',  ( -3.998720052560664762, 27.76176938167515118, 20.94377226548378346 ) ) ;
#19348 = DIRECTION ( 'NONE',  ( -0.4999999999999921729, 0.8660254037844432595, 0.000000000000000000 ) ) ;
#19349 = DIRECTION ( 'NONE',  ( 1.000000000000000000, 0.000000000000000000, 0.000000000000000000 ) ) ;
#19350 = CIRCLE ( 'NONE', #1858, 0.4999999999999988898 ) ;
#19351 = CIRCLE ( 'NONE', #34300, 1.000000000000002665 ) ;
#19352 = FACE_BOUND ( 'NONE', #9663, .T. ) ;
#19353 = CARTESIAN_POINT ( 'NONE',  ( 18.23687175285641260, 10.52906281568832902, 19.27171037444156809 ) ) ;
#19354 = CARTESIAN_POINT ( 'NONE',  ( -20.48481815786151827, 8.169629148835463539, -20.07635314567754747 ) ) ;
#19355 = CARTESIAN_POINT ( 'NONE',  ( 20.89534821297474565, -25.82708108466523100, -9.908281912035883821 ) ) ;
#19356 = AXIS2_PLACEMENT_3D ( 'NONE', #1316, #35448, #7602 ) ;
#19357 = DIRECTION ( 'NONE',  ( -1.224646799147351235E-16, 1.000000000000000000, 0.000000000000000000 ) ) ;
#19358 = CARTESIAN_POINT ( 'NONE',  ( 14.22661425981019256, 24.64141455453919249, -12.53612259479494995 ) ) ;
#19359 = ORIENTED_EDGE ( 'NONE', *, *, #17315, .T. ) ;
#19360 = CARTESIAN_POINT ( 'NONE',  ( -12.01347213543522585, 16.66139596754671715, -28.74651697924976190 ) ) ;
#19361 = CARTESIAN_POINT ( 'NONE',  ( -28.10500220466552790, -8.168651434043027848, 20.50957957746051363 ) ) ;
#19362 = CARTESIAN_POINT ( 'NONE',  ( 10.66948297901455156, 33.02599466632828751, 10.49999999999999822 ) ) ;
#19363 = CARTESIAN_POINT ( 'NONE',  ( 11.20926058852595908, 17.73831205782239806, -26.22754255443350857 ) ) ;
#19364 = ORIENTED_EDGE ( 'NONE', *, *, #32198, .F. ) ;
#19365 = CARTESIAN_POINT ( 'NONE',  ( 32.29060608969265900, -17.80231044390160378, -9.282265745321158334 ) ) ;
#19366 = CARTESIAN_POINT ( 'NONE',  ( -13.63581098909220479, 27.45627467658446008, 7.000000000000000000 ) ) ;
#19367 = ORIENTED_EDGE ( 'NONE', *, *, #4167, .T. ) ;
#19369 = CARTESIAN_POINT ( 'NONE',  ( -8.294006203984645609, 33.46401007850805343, 12.00000000000000000 ) ) ;
#19368 = CARTESIAN_POINT ( 'NONE',  ( -10.72725030361012521, 17.46952664121795351, -29.99999999999999289 ) ) ;
#19370 = CARTESIAN_POINT ( 'NONE',  ( -9.745989649151084677, -18.27917357566746048, -27.43878329331307242 ) ) ;
#19371 = CARTESIAN_POINT ( 'NONE',  ( 12.47058434440061880, 14.72275450261863838, 10.96580508970282430 ) ) ;
#19372 = ORIENTED_EDGE ( 'NONE', *, *, #34556, .T. ) ;
#19373 = CARTESIAN_POINT ( 'NONE',  ( -18.23120227974498420, -9.562336488320314132, -28.44603666067110836 ) ) ;
#19374 = CARTESIAN_POINT ( 'NONE',  ( -8.933264501347940367, -18.58110093778079275, -28.11105939349013028 ) ) ;
#19375 = CARTESIAN_POINT ( 'NONE',  ( -5.136393443230096167, 36.08535633838094725, 10.66666666666666785 ) ) ;
#19376 = CARTESIAN_POINT ( 'NONE',  ( 13.40733656136086616, 18.39885974385108014, -20.74996682341825505 ) ) ;
#19377 = VERTEX_POINT ( 'NONE', #36709 ) ;
#19378 = CARTESIAN_POINT ( 'NONE',  ( 24.84641422454732407, 2.937850337337710727, -15.64433848410505945 ) ) ;
#19379 = DIRECTION ( 'NONE',  ( 1.000000000000000000, 0.000000000000000000, 0.000000000000000000 ) ) ;
#19380 = CARTESIAN_POINT ( 'NONE',  ( 4.984135866956514782, 36.15314577889351000, 7.500000000000000888 ) ) ;
#19381 = DIRECTION ( 'NONE',  ( -0.000000000000000000, -0.000000000000000000, -1.000000000000000000 ) ) ;
#19382 = ORIENTED_EDGE ( 'NONE', *, *, #21885, .T. ) ;
#19383 = CARTESIAN_POINT ( 'NONE',  ( -31.27312981421062688, -0.4309787749141147928, -5.471709692244465906 ) ) ;
#19385 = CARTESIAN_POINT ( 'NONE',  ( 20.70843681679315651, 0.6154661857135520497, -27.43333504746348694 ) ) ;
#19384 = AXIS2_PLACEMENT_3D ( 'NONE', #35492, #16808, #17009 ) ;
#19386 = VECTOR ( 'NONE', #32264, 1000.000000000000114 ) ;
#19387 = CARTESIAN_POINT ( 'NONE',  ( 29.98847540738146122, -8.745685015162887765, 19.99202127657102324 ) ) ;
#19388 = ORIENTED_EDGE ( 'NONE', *, *, #27501, .F. ) ;
#19389 = AXIS2_PLACEMENT_3D ( 'NONE', #19149, #19348, #3114 ) ;
#19390 = CARTESIAN_POINT ( 'NONE',  ( -12.33616729053607486, -27.99489201236593061, -13.58461195433496194 ) ) ;
#19391 = DIRECTION ( 'NONE',  ( 0.000000000000000000, -1.000000000000000000, 0.000000000000000000 ) ) ;
#19392 = VERTEX_POINT ( 'NONE', #30009 ) ;
#19393 = CARTESIAN_POINT ( 'NONE',  ( 0.7344908159097338629, 8.754836972118123839, 6.000000000000000000 ) ) ;
#19394 = LINE ( 'NONE', #9859, #12979 ) ;
#19395 = DIRECTION ( 'NONE',  ( 0.9510565162951541973, 0.3090169943749456194, 0.000000000000000000 ) ) ;
#19396 = CARTESIAN_POINT ( 'NONE',  ( 4.258837352292506928, 31.86736653883517079, -13.83424449677746360 ) ) ;
#19397 = DIRECTION ( 'NONE',  ( 0.9945218953682730678, -0.1045284632676569819, 0.000000000000000000 ) ) ;
#19398 = EDGE_CURVE ( 'NONE', #3976, #19822, #11724, .T. ) ;
#19399 = ORIENTED_EDGE ( 'NONE', *, *, #5365, .F. ) ;
#19400 = CARTESIAN_POINT ( 'NONE',  ( 0.5000000000000000000, 37.00000000000000711, 7.500000000000000888 ) ) ;
#19401 = CARTESIAN_POINT ( 'NONE',  ( -13.24038105676664401, 15.43301270189234486, 11.00000000000000000 ) ) ;
#19402 = CARTESIAN_POINT ( 'NONE',  ( 27.24828611745593321, -25.13066665804571542, -6.297441403926967496 ) ) ;
#19403 = LINE ( 'NONE', #28749, #17999 ) ;
#19404 = DIRECTION ( 'NONE',  ( -0.000000000000000000, -0.000000000000000000, -1.000000000000000000 ) ) ;
#19405 = CARTESIAN_POINT ( 'NONE',  ( 14.69283426033394768, 26.51965037005133752, -9.670188778881371405 ) ) ;
#19406 = DIRECTION ( 'NONE',  ( 0.000000000000000000, 0.000000000000000000, 1.000000000000000000 ) ) ;
#19407 = EDGE_LOOP ( 'NONE', ( #20137, #13920, #25669, #25187, #7233 ) ) ;
#19409 = CARTESIAN_POINT ( 'NONE',  ( 10.78893975237932956, 23.27376113029817617, 13.00000000000000178 ) ) ;
#19408 = CARTESIAN_POINT ( 'NONE',  ( -15.72881319288876156, 16.59632136301366856, -18.88276093887042606 ) ) ;
#19410 = EDGE_CURVE ( 'NONE', #22335, #14611, #21263, .T. ) ;
#19411 = CARTESIAN_POINT ( 'NONE',  ( 6.756943768455586863, 44.94911180988961519, 10.00000000000000000 ) ) ;
#19412 = CARTESIAN_POINT ( 'NONE',  ( 9.476873889470034840, -18.17797724348699973, -29.34878039533210625 ) ) ;
#19413 = EDGE_CURVE ( 'NONE', #12432, #6323, #17469, .T. ) ;
#19414 = DIRECTION ( 'NONE',  ( -0.000000000000000000, -0.000000000000000000, -1.000000000000000000 ) ) ;
#19415 = CARTESIAN_POINT ( 'NONE',  ( 15.29332824945628566, 26.51959359426387763, -7.358051658420890817 ) ) ;
#19416 = ORIENTED_EDGE ( 'NONE', *, *, #30110, .T. ) ;
#19417 = CARTESIAN_POINT ( 'NONE',  ( 15.23218277980890356, 26.40650644525691249, -7.827771362956440271 ) ) ;
#19418 = AXIS2_PLACEMENT_3D ( 'NONE', #34152, #25201, #31298 ) ;
#19419 = B_SPLINE_SURFACE_WITH_KNOTS ( 'NONE', 1, 3, ( 
 ( #16320, #16526, #28306, #26057, #34804, #6955, #29114, #678, #13058, #1285 ),
 ( #13667, #38051, #19362, #486, #6563, #28705, #25260, #12868, #37656, #9825 ) ),
 .UNSPECIFIED., .F., .F., .F.,
 ( 2, 2 ),
 ( 4, 2, 2, 2, 4 ),
 ( 0.000000000000000000, 1.000000000000000000 ),
 ( 2.137751973267104866, 2.530451054965827229, 2.923150136664549592, 3.315849218363272399, 3.708548300061994762 ),
 .UNSPECIFIED. ) ;
#19420 = VERTEX_POINT ( 'NONE', #5618 ) ;
#19422 = CYLINDRICAL_SURFACE ( 'NONE', #7556, 1.000000000000000000 ) ;
#19421 = CARTESIAN_POINT ( 'NONE',  ( -12.35792326267267072, 20.53483958506731710, -19.48932210671636867 ) ) ;
#19423 = CARTESIAN_POINT ( 'NONE',  ( -9.495857434766111993, -18.21849447287409518, -28.70794251271205866 ) ) ;
#19424 = CARTESIAN_POINT ( 'NONE',  ( -15.12590024503300512, -28.14827041158709520, 13.92931973827808889 ) ) ;
#19425 = CARTESIAN_POINT ( 'NONE',  ( -19.54867522336399688, -13.46797132751421167, -21.85517049677807933 ) ) ;
#19426 = CARTESIAN_POINT ( 'NONE',  ( -3.274116759621854111, -20.28896347757955354, -29.42369938977917343 ) ) ;
#19427 = CARTESIAN_POINT ( 'NONE',  ( 14.33614363210685205, 23.23110485604417619, -13.54771175783602466 ) ) ;
#19428 = EDGE_LOOP ( 'NONE', ( #23459, #5049, #25068, #10363, #9996 ) ) ;
#19429 = CARTESIAN_POINT ( 'NONE',  ( 19.78994368857117081, 10.03402965537161329, -19.05768763028667223 ) ) ;
#19430 = DIRECTION ( 'NONE',  ( -0.5877852522924796874, -0.8090169943749426773, 0.000000000000000000 ) ) ;
#19431 = CARTESIAN_POINT ( 'NONE',  ( -9.924110812759902700, 32.99075218357604200, 17.92354375535331101 ) ) ;
#19432 = ORIENTED_EDGE ( 'NONE', *, *, #9857, .F. ) ;
#19433 = CARTESIAN_POINT ( 'NONE',  ( -23.42691890934632326, -2.892262406529196195, -21.19212511098400142 ) ) ;
#19434 = CARTESIAN_POINT ( 'NONE',  ( -21.61978140912946955, 6.167694920803358016, 18.87996532025794849 ) ) ;
#19435 = ORIENTED_EDGE ( 'NONE', *, *, #9638, .T. ) ;
#19436 = CARTESIAN_POINT ( 'NONE',  ( -9.294006203984645609, 33.46401007850805343, 13.00000000000000178 ) ) ;
#19437 = CARTESIAN_POINT ( 'NONE',  ( 24.08873164041084536, -13.27722336041302320, 22.99999999999999645 ) ) ;
#19438 = EDGE_CURVE ( 'NONE', #9748, #21382, #4485, .T. ) ;
#19439 = CARTESIAN_POINT ( 'NONE',  ( 23.47267981164478101, -10.30042122731402543, -19.66540645570583123 ) ) ;
#19440 = CARTESIAN_POINT ( 'NONE',  ( 24.63751168576237305, -28.54157386115114292, 12.14047268033101545 ) ) ;
#19441 = CONICAL_SURFACE ( 'NONE', #25272, 1.000000000000009548, 0.7853981633974567167 ) ;
#19442 = VERTEX_POINT ( 'NONE', #11526 ) ;
#19443 = ORIENTED_EDGE ( 'NONE', *, *, #14464, .T. ) ;
#19444 = AXIS2_PLACEMENT_3D ( 'NONE', #5266, #29848, #36351 ) ;
#19445 = CYLINDRICAL_SURFACE ( 'NONE', #3474, 1.000000000000000000 ) ;
#19446 = CARTESIAN_POINT ( 'NONE',  ( 13.94482798346721530, 26.50521816028912525, 9.500000000000000000 ) ) ;
#19447 = DIRECTION ( 'NONE',  ( 1.000000000000000000, 0.000000000000000000, 0.000000000000000000 ) ) ;
#19448 = ORIENTED_EDGE ( 'NONE', *, *, #9518, .T. ) ;
#19449 = CARTESIAN_POINT ( 'NONE',  ( -1.909966974610407098, 38.03150725742897720, -7.118504882345924933 ) ) ;
#19450 = LINE ( 'NONE', #25150, #28239 ) ;
#19451 = DIRECTION ( 'NONE',  ( 1.000000000000000000, 0.000000000000000000, 0.000000000000000000 ) ) ;
#19452 = CYLINDRICAL_SURFACE ( 'NONE', #38998, 0.5000000000000004441 ) ;
#19454 = EDGE_CURVE ( 'NONE', #25405, #25736, #5823, .T. ) ;
#19453 = DIRECTION ( 'NONE',  ( 1.000000000000000000, -6.938893903907210234E-15, 0.000000000000000000 ) ) ;
#19455 = DIRECTION ( 'NONE',  ( 1.000000000000000000, 0.000000000000000000, 0.000000000000000000 ) ) ;
#19456 = CARTESIAN_POINT ( 'NONE',  ( 10.13776086571952995, 19.50640881937047055, -23.64984537069171111 ) ) ;
#19457 = CARTESIAN_POINT ( 'NONE',  ( 4.476901250629513385, 26.36149378532653031, 12.00000000000000000 ) ) ;
#19458 = EDGE_LOOP ( 'NONE', ( #20731, #9657, #22805, #10961 ) ) ;
#19460 = DIRECTION ( 'NONE',  ( -0.7431448254773871387, 0.6691306063588662312, -6.938893903907226800E-15 ) ) ;
#19459 = CARTESIAN_POINT ( 'NONE',  ( -19.63432798946420021, 15.59186056508892904, -6.934370416219701738 ) ) ;
#19461 = LINE ( 'NONE', #28407, #34793 ) ;
#19462 = CARTESIAN_POINT ( 'NONE',  ( 12.69066353061625740, -22.55866965907024735, -16.43980381259239110 ) ) ;
#19463 = EDGE_CURVE ( 'NONE', #20607, #39696, #40148, .T. ) ;
#19464 = DIRECTION ( 'NONE',  ( 0.000000000000000000, -0.000000000000000000, 1.000000000000000000 ) ) ;
#19465 = CARTESIAN_POINT ( 'NONE',  ( 14.71862476482751347, 25.45363487584512185, -10.64941651680690349 ) ) ;
#19466 = CARTESIAN_POINT ( 'NONE',  ( 2.927345865710861972E-15, 22.57051819516765789, -30.00000000000001421 ) ) ;
#19467 = B_SPLINE_CURVE_WITH_KNOTS ( 'NONE', 3,
 ( #15136, #33244, #2356, #33445 ),
 .UNSPECIFIED., .F., .F.,
 ( 4, 4 ),
 ( 0.000000000000000000, 1.000000000000000000 ),
 .UNSPECIFIED. ) ;
#19468 = DIRECTION ( 'NONE',  ( 1.000000000000000000, 0.000000000000000000, 0.000000000000000000 ) ) ;
#19469 = CARTESIAN_POINT ( 'NONE',  ( -15.47784844748352384, -15.42996703057364982, -24.40905844545180159 ) ) ;
#19470 = CARTESIAN_POINT ( 'NONE',  ( 6.083101977165589425, -24.65543650029558620, -9.357407788547908112 ) ) ;
#19471 = CARTESIAN_POINT ( 'NONE',  ( 15.02539757819879895, 25.52099869179298253, -9.713273572205364914 ) ) ;
#19472 = CARTESIAN_POINT ( 'NONE',  ( 24.95130836960470688, -16.89649762504703290, -15.68942752906997029 ) ) ;
#19473 = CYLINDRICAL_SURFACE ( 'NONE', #7605, 17.99999999999989697 ) ;
#19474 = CARTESIAN_POINT ( 'NONE',  ( 7.917734535019441466, 14.47043272369397116, 13.00000000000000178 ) ) ;
#19475 = EDGE_LOOP ( 'NONE', ( #28167, #17758, #17750 ) ) ;
#19476 = VECTOR ( 'NONE', #17379, 1000.000000000000114 ) ;
#19477 = CARTESIAN_POINT ( 'NONE',  ( -5.944679600751215709, 19.85052517187110510, -27.81791890879877371 ) ) ;
#19478 = CARTESIAN_POINT ( 'NONE',  ( 14.89501059309194808, 21.76138985984211160, 10.49999999999999822 ) ) ;
#19479 = ORIENTED_EDGE ( 'NONE', *, *, #38826, .T. ) ;
#19480 = CARTESIAN_POINT ( 'NONE',  ( 24.57639991767630505, 0.3971110913580137569, -18.44753617970850357 ) ) ;
#19481 = CARTESIAN_POINT ( 'NONE',  ( 0.000000000000000000, 22.50000000000000355, 7.000000000000000000 ) ) ;
#19482 = ADVANCED_FACE ( 'NONE', ( #17637 ), #33275, .F. ) ;
#19483 = CARTESIAN_POINT ( 'NONE',  ( -32.33143948541737700, 1.358872982502395965, 11.55979286843935050 ) ) ;
#19484 = EDGE_CURVE ( 'NONE', #19098, #14611, #33864, .T. ) ;
#19485 = VERTEX_POINT ( 'NONE', #15166 ) ;
#19486 = CARTESIAN_POINT ( 'NONE',  ( -30.68756512533535386, 0.07659338870116388920, -6.417149656870462238 ) ) ;
#19487 = DIRECTION ( 'NONE',  ( 0.000000000000000000, 0.000000000000000000, 1.000000000000000000 ) ) ;
#19488 = ORIENTED_EDGE ( 'NONE', *, *, #4052, .T. ) ;
#19489 = CARTESIAN_POINT ( 'NONE',  ( 27.17392716606788738, -6.462269799051562735, -16.83742809164828813 ) ) ;
#19490 = AXIS2_PLACEMENT_3D ( 'NONE', #6551, #16512, #9416 ) ;
#19491 = CONICAL_SURFACE ( 'NONE', #2654, 1.000000000000004441, 0.7853981633974524978 ) ;
#19492 = EDGE_LOOP ( 'NONE', ( #36640, #7088, #27067, #19998 ) ) ;
#19493 = DIRECTION ( 'NONE',  ( -0.4999999999999919509, -0.8660254037844432595, 0.000000000000000000 ) ) ;
#19494 = DIRECTION ( 'NONE',  ( 0.2079116908177532919, -0.9781476007338070211, -0.000000000000000000 ) ) ;
#19495 = DIRECTION ( 'NONE',  ( 0.000000000000000000, 0.000000000000000000, -1.000000000000000000 ) ) ;
#19496 = CARTESIAN_POINT ( 'NONE',  ( 10.49474413300069386, 21.89971208337373909, 10.00000000000000000 ) ) ;
#19497 = CARTESIAN_POINT ( 'NONE',  ( -3.681484855442400672, 33.42880943655691084, 19.66345542862530138 ) ) ;
#19498 = CARTESIAN_POINT ( 'NONE',  ( 2.568190708544436873, 12.82247983807080871, 10.50000000000000000 ) ) ;
#19499 = VERTEX_POINT ( 'NONE', #17833 ) ;
#19500 =( NAMED_UNIT ( * ) PLANE_ANGLE_UNIT ( ) SI_UNIT ( $, .RADIAN. ) );
#19501 = CARTESIAN_POINT ( 'NONE',  ( 0.09913434393121192678, 20.50242196421552165, -30.00000000000001066 ) ) ;
#19502 = DIRECTION ( 'NONE',  ( 0.000000000000000000, 0.000000000000000000, 1.000000000000000000 ) ) ;
#19503 = CIRCLE ( 'NONE', #2013, 1.000000000000000000 ) ;
#19504 = CARTESIAN_POINT ( 'NONE',  ( -25.71480618105494997, 9.014447550991285141, 11.00000000000190603 ) ) ;
#19505 = EDGE_CURVE ( 'NONE', #18941, #6805, #18027, .T. ) ;
#19506 = CARTESIAN_POINT ( 'NONE',  ( 14.31276673011558209, 14.78156386205161610, -28.23264745093075234 ) ) ;
#19507 = CARTESIAN_POINT ( 'NONE',  ( 6.253476071100840805, 21.63181789309742697, -23.22608574772441870 ) ) ;
#19508 = ORIENTED_EDGE ( 'NONE', *, *, #6413, .T. ) ;
#19509 = CARTESIAN_POINT ( 'NONE',  ( 10.14716901145161465, 12.46304090461738667, 12.00000000000000000 ) ) ;
#19510 = CARTESIAN_POINT ( 'NONE',  ( 11.35509078104043112, -19.86412214972710899, -21.54793691088456242 ) ) ;
#19511 = FACE_OUTER_BOUND ( 'NONE', #8360, .T. ) ;
#19512 = ADVANCED_FACE ( 'NONE', ( #20677 ), #30212, .F. ) ;
#19513 = CARTESIAN_POINT ( 'NONE',  ( 12.67417846324118358, 14.47720745114811436, 7.499999999999997335 ) ) ;
#19514 = B_SPLINE_CURVE_WITH_KNOTS ( 'NONE', 3,
 ( #16460, #28845, #32513, #7712, #17069, #10564 ),
 .UNSPECIFIED., .F., .F.,
 ( 4, 2, 4 ),
 ( 0.000000000000000000, 0.5000000000000000000, 1.000000000000000000 ),
 .UNSPECIFIED. ) ;
#19515 = ORIENTED_EDGE ( 'NONE', *, *, #12356, .T. ) ;
#19516 = CARTESIAN_POINT ( 'NONE',  ( -11.13735207663799542, 17.60437961019085762, -26.83156383840440640 ) ) ;
#19517 = VECTOR ( 'NONE', #7560, 1000.000000000000114 ) ;
#19518 = CARTESIAN_POINT ( 'NONE',  ( -35.36447994912705184, -9.234655410424128519, 16.30093088680190405 ) ) ;
#19519 = CARTESIAN_POINT ( 'NONE',  ( 14.20559445519923081, -25.38033748439481840, -10.66220569548931252 ) ) ;
#19520 = AXIS2_PLACEMENT_3D ( 'NONE', #14569, #39348, #11525 ) ;
#19521 = CARTESIAN_POINT ( 'NONE',  ( 3.610593701936705369, 31.83882289796390808, 10.50000000000000000 ) ) ;
#19522 = ORIENTED_EDGE ( 'NONE', *, *, #25437, .T. ) ;
#19523 = ORIENTED_EDGE ( 'NONE', *, *, #3467, .F. ) ;
#19524 = CARTESIAN_POINT ( 'NONE',  ( -12.65601555930210509, 32.35306062433939900, -5.000000000000000888 ) ) ;
#19525 = FACE_OUTER_BOUND ( 'NONE', #30491, .T. ) ;
#19526 = CARTESIAN_POINT ( 'NONE',  ( -12.74038105676667243, 14.56698729810793935, 10.59344459855562448 ) ) ;
#19527 = CARTESIAN_POINT ( 'NONE',  ( -22.71460563496382079, -4.894690698724015299, -22.13699196390837187 ) ) ;
#19528 = FACE_OUTER_BOUND ( 'NONE', #10837, .T. ) ;
#19529 = EDGE_LOOP ( 'NONE', ( #14763, #28511, #14802, #20994 ) ) ;
#19530 = CARTESIAN_POINT ( 'NONE',  ( 20.47484565207173546, 1.015995796922180006, -30.00000000000000355 ) ) ;
#19531 = CARTESIAN_POINT ( 'NONE',  ( 35.48538791413476190, -11.24999995268670006, -5.000000000000002665 ) ) ;
#19532 = CARTESIAN_POINT ( 'NONE',  ( 7.133890061153790541, 30.26901619224539175, 10.50000000000000000 ) ) ;
#19533 = VECTOR ( 'NONE', #25154, 1000.000000000000114 ) ;
#19534 = ORIENTED_EDGE ( 'NONE', *, *, #3268, .T. ) ;
#19535 = CARTESIAN_POINT ( 'NONE',  ( -20.97084573062722868, 0.7958700342359013025, -26.22383286897646926 ) ) ;
#19536 = DIRECTION ( 'NONE',  ( -0.000000000000000000, -0.000000000000000000, 1.000000000000000000 ) ) ;
#19538 = ADVANCED_FACE ( 'NONE', ( #27161 ), #26960, .T. ) ;
#19537 = ORIENTED_EDGE ( 'NONE', *, *, #31938, .F. ) ;
#19539 = CARTESIAN_POINT ( 'NONE',  ( 23.89622136170986266, -1.342169087894246715, -20.29735455761264262 ) ) ;
#19540 = CARTESIAN_POINT ( 'NONE',  ( -13.63581098909220479, 27.45627467658446008, 7.000000000000000000 ) ) ;
#19541 = CARTESIAN_POINT ( 'NONE',  ( 20.67781403882192848, -27.68125770801123409, 15.72805884748939853 ) ) ;
#19542 = VERTEX_POINT ( 'NONE', #27556 ) ;
#19543 = CARTESIAN_POINT ( 'NONE',  ( 11.06388406389920753, 34.19581601475721300, 16.30093088680188274 ) ) ;
#19544 = DIRECTION ( 'NONE',  ( 0.000000000000000000, 0.000000000000000000, 1.000000000000000000 ) ) ;
#19545 = CARTESIAN_POINT ( 'NONE',  ( -4.137850160812051037, 25.30681243524895052, 20.99999999999999645 ) ) ;
#19546 = CIRCLE ( 'NONE', #16980, 1.000000000000000888 ) ;
#19547 = FACE_OUTER_BOUND ( 'NONE', #4177, .T. ) ;
#19548 = AXIS2_PLACEMENT_3D ( 'NONE', #29095, #1268, #13652 ) ;
#19549 = DIRECTION ( 'NONE',  ( 0.4731467892558179900, 0.5254827454987496260, 0.7071067811865524577 ) ) ;
#19550 = EDGE_CURVE ( 'NONE', #33546, #35323, #601, .T. ) ;
#19551 = PLANE ( 'NONE',  #39155 ) ;
#19552 = EDGE_CURVE ( 'NONE', #28707, #10650, #33474, .T. ) ;
#19553 = CARTESIAN_POINT ( 'NONE',  ( 24.37528612859215471, 1.300641855011779979, 19.27171037445292257 ) ) ;
#19554 = CARTESIAN_POINT ( 'NONE',  ( -20.88678011286848601, 9.201183980115258620, -16.96328878660644790 ) ) ;
#19555 = AXIS2_PLACEMENT_3D ( 'NONE', #26427, #32740, #14036 ) ;
#19556 = CARTESIAN_POINT ( 'NONE',  ( 13.60358058528764325, -16.01930624727132368, -26.49426777756269402 ) ) ;
#19557 = LINE ( 'NONE', #25649, #31930 ) ;
#19558 = ORIENTED_EDGE ( 'NONE', *, *, #5610, .F. ) ;
#19559 = CARTESIAN_POINT ( 'NONE',  ( 15.24511751409066385, 26.68580942243475462, -7.353470569735968354 ) ) ;
#19560 = ORIENTED_EDGE ( 'NONE', *, *, #10108, .F. ) ;
#19561 = CARTESIAN_POINT ( 'NONE',  ( -12.56632571172008817, 18.66082033402736684, -21.73012474470345623 ) ) ;
#19562 = EDGE_CURVE ( 'NONE', #40105, #31103, #39744, .T. ) ;
#19563 = CARTESIAN_POINT ( 'NONE',  ( -31.11751153274386184, -7.091459469499522328, 19.27171037444191271 ) ) ;
#19564 = DIRECTION ( 'NONE',  ( 1.000000000000000000, 0.000000000000000000, 0.000000000000000000 ) ) ;
#19565 = CARTESIAN_POINT ( 'NONE',  ( 11.35793817090670643, 18.00059461891385837, -25.02099990739169755 ) ) ;
#19566 = ORIENTED_EDGE ( 'NONE', *, *, #3867, .T. ) ;
#19567 = CARTESIAN_POINT ( 'NONE',  ( 31.99386290378327402, -17.63808712151127622, -9.726114945743994156 ) ) ;
#19568 = CARTESIAN_POINT ( 'NONE',  ( 16.38619327006176363, 7.072988944186805682, 11.00000000000000000 ) ) ;
#19569 = EDGE_LOOP ( 'NONE', ( #25382, #37579 ) ) ;
#19571 = DIRECTION ( 'NONE',  ( -0.000000000000000000, -0.000000000000000000, -1.000000000000000000 ) ) ;
#19570 = CARTESIAN_POINT ( 'NONE',  ( -14.33922274708733369, 25.50030895700567157, -11.55966223143600047 ) ) ;
#19572 = CARTESIAN_POINT ( 'NONE',  ( -13.23125664540841839, -22.57002348086217580, -16.38072535630667304 ) ) ;
#19573 = CARTESIAN_POINT ( 'NONE',  ( 9.806975420853749625, 31.15003855377755571, 6.000000000000000000 ) ) ;
#19574 = AXIS2_PLACEMENT_3D ( 'NONE', #38344, #29604, #26149 ) ;
#19575 = VERTEX_POINT ( 'NONE', #21654 ) ;
#19576 = CARTESIAN_POINT ( 'NONE',  ( -20.06706900687590078, -9.031097061974783458, -24.24539032328864607 ) ) ;
#19577 = CARTESIAN_POINT ( 'NONE',  ( -14.31977663809412959, -26.17573132815211423, -7.833052140176563150 ) ) ;
#19578 = CARTESIAN_POINT ( 'NONE',  ( 10.06946225350410806, 32.23940090176269990, 9.500000000000000000 ) ) ;
#19579 = CARTESIAN_POINT ( 'NONE',  ( 12.40596010115784864, 16.36831411943918724, -28.76043401885274164 ) ) ;
#19580 = EDGE_LOOP ( 'NONE', ( #24377, #539, #10677, #6884 ) ) ;
#19581 = CARTESIAN_POINT ( 'NONE',  ( 24.35497143909449846, 3.753685042505659375, -15.69857805530405770 ) ) ;
#19582 = PLANE ( 'NONE',  #5067 ) ;
#19583 = CARTESIAN_POINT ( 'NONE',  ( 8.401171878996485987, 21.11424711454080594, 9.000000000000001776 ) ) ;
#19584 = EDGE_LOOP ( 'NONE', ( #17871, #16960 ) ) ;
#19585 = ADVANCED_FACE ( 'NONE', ( #12515 ), #15963, .F. ) ;
#19586 = CARTESIAN_POINT ( 'NONE',  ( -22.80720800583724994, 0.3548441269305998569, -21.58251948928919717 ) ) ;
#19587 = EDGE_CURVE ( 'NONE', #7787, #33406, #25490, .T. ) ;
#19588 = CARTESIAN_POINT ( 'NONE',  ( 29.81871666203916860, -0.4633601488208085595, -10.61095171305142237 ) ) ;
#19589 = CARTESIAN_POINT ( 'NONE',  ( 25.09931006221244942, -21.40067874915650137, 19.66345542862496387 ) ) ;
#19590 = ORIENTED_EDGE ( 'NONE', *, *, #6198, .F. ) ;
#19591 = AXIS2_PLACEMENT_3D ( 'NONE', #8303, #23134, #2016 ) ;
#19592 = CARTESIAN_POINT ( 'NONE',  ( -20.55563217186186620, -29.52600041847739831, -13.99876745781540777 ) ) ;
#19593 = CARTESIAN_POINT ( 'NONE',  ( -12.30736835487442704, 14.81698729810789672, 7.000000000000000000 ) ) ;
#19594 = LINE ( 'NONE', #32407, #33017 ) ;
#19595 = DIRECTION ( 'NONE',  ( 0.000000000000000000, 0.000000000000000000, 1.000000000000000000 ) ) ;
#19596 = EDGE_CURVE ( 'NONE', #36229, #10557, #9271, .T. ) ;
#19597 = DIRECTION ( 'NONE',  ( 1.000000000000000000, 0.000000000000000000, 0.000000000000000000 ) ) ;
#19598 = DIRECTION ( 'NONE',  ( 0.000000000000000000, 0.000000000000000000, 1.000000000000000000 ) ) ;
#19599 = AXIS2_PLACEMENT_3D ( 'NONE', #4114, #37841, #22396 ) ;
#19600 = EDGE_CURVE ( 'NONE', #12521, #6531, #34361, .T. ) ;
#19601 = CARTESIAN_POINT ( 'NONE',  ( 13.19371393710734708, 15.45995597598971116, 10.76099332938163933 ) ) ;
#19602 = ORIENTED_EDGE ( 'NONE', *, *, #33203, .F. ) ;
#19603 = DIRECTION ( 'NONE',  ( 0.000000000000000000, 0.000000000000000000, 1.000000000000000000 ) ) ;
#19604 = B_SPLINE_CURVE_WITH_KNOTS ( 'NONE', 3,
 ( #32425, #12920, #26109, #16374 ),
 .UNSPECIFIED., .F., .F.,
 ( 4, 4 ),
 ( 0.000000000000000000, 1.000000000000000000 ),
 .UNSPECIFIED. ) ;
#19605 = CARTESIAN_POINT ( 'NONE',  ( -3.476907992048017260, 18.63850621467409496, 12.00000000000000000 ) ) ;
#19606 = CARTESIAN_POINT ( 'NONE',  ( 15.49469401537697877, -13.43643885346290467, -29.23020519650644999 ) ) ;
#19607 = CYLINDRICAL_SURFACE ( 'NONE', #23846, 1.000000000000000000 ) ;
#19608 = DIRECTION ( 'NONE',  ( 0.9945218953682746221, 0.1045284632676415221, -0.000000000000000000 ) ) ;
#19609 = CARTESIAN_POINT ( 'NONE',  ( 10.57951390145473880, 17.61515124497404727, -28.68921471184503247 ) ) ;
#19610 = DIRECTION ( 'NONE',  ( 0.000000000000000000, 0.000000000000000000, 1.000000000000000000 ) ) ;
#19611 = VERTEX_POINT ( 'NONE', #21852 ) ;
#19612 = CARTESIAN_POINT ( 'NONE',  ( -15.94292200871946363, 16.92080024915129144, -17.84332993048722571 ) ) ;
#19613 = PLANE ( 'NONE',  #12095 ) ;
#19614 = CARTESIAN_POINT ( 'NONE',  ( 10.52269179291350376, -19.57971688490037110, -22.73667610652659477 ) ) ;
#19615 = DIRECTION ( 'NONE',  ( -0.000000000000000000, -0.000000000000000000, -1.000000000000000000 ) ) ;
#19616 = CARTESIAN_POINT ( 'NONE',  ( 15.02065328176380810, 25.96055969456606505, -9.238703151935258262 ) ) ;
#19617 = EDGE_LOOP ( 'NONE', ( #31995, #15692, #5433, #27563 ) ) ;
#19618 = CARTESIAN_POINT ( 'NONE',  ( 15.41558956916364664, 26.78481017491955285, -5.000000000000000000 ) ) ;
#19619 = VERTEX_POINT ( 'NONE', #16162 ) ;
#19621 = CARTESIAN_POINT ( 'NONE',  ( 3.607749162633204332, 7.931741834401770497, 10.49999999999999822 ) ) ;
#19620 = CARTESIAN_POINT ( 'NONE',  ( -11.02719225547328818, 17.53326252175294897, -27.44422965767462586 ) ) ;
#19622 = CARTESIAN_POINT ( 'NONE',  ( -15.23983141892431981, -26.39157610348082983, -7.828191424447879854 ) ) ;
#19623 = CARTESIAN_POINT ( 'NONE',  ( -36.93643098903786637, -14.76343610888389257, 12.73282698324853079 ) ) ;
#19624 = VECTOR ( 'NONE', #3936, 1000.000000000000227 ) ;
#19625 = CARTESIAN_POINT ( 'NONE',  ( -31.59563369834444302, -19.08695624603514673, -9.281276475905125167 ) ) ;
#19626 = CARTESIAN_POINT ( 'NONE',  ( -3.293094573708170714, -20.34456577815404188, -28.28364186545810455 ) ) ;
#19627 = CARTESIAN_POINT ( 'NONE',  ( 11.39019116559808076, 17.18986029501263602, -28.09783186015068779 ) ) ;
#19628 = ORIENTED_EDGE ( 'NONE', *, *, #27929, .T. ) ;
#19629 = CARTESIAN_POINT ( 'NONE',  ( 20.92795771179241626, 8.548002118599240973, -17.98415772267350832 ) ) ;
#19630 = CARTESIAN_POINT ( 'NONE',  ( 31.12126637737784307, -22.29934860316716438, -5.000000000000000000 ) ) ;
#19631 = CARTESIAN_POINT ( 'NONE',  ( 2.525645716490518389, 8.212903943950921715, 11.00000000000000000 ) ) ;
#19632 = CARTESIAN_POINT ( 'NONE',  ( -4.583318357746721361, 36.10598097934249040, 17.92354375535251521 ) ) ;
#19633 = ORIENTED_EDGE ( 'NONE', *, *, #23709, .F. ) ;
#19634 = CARTESIAN_POINT ( 'NONE',  ( -26.72032155736675207, -3.378370715629333887, -17.03970011708248222 ) ) ;
#19635 = CARTESIAN_POINT ( 'NONE',  ( -15.65370567419120640, 2.019989953599362842, 20.99999999999999645 ) ) ;
#19636 = EDGE_LOOP ( 'NONE', ( #24710, #18065, #31927 ) ) ;
#19637 = CARTESIAN_POINT ( 'NONE',  ( 24.22138565352628348, -9.557272464391640909, 20.99999999999999645 ) ) ;
#19638 = CARTESIAN_POINT ( 'NONE',  ( 14.57736017774144877, 22.47612012567140383, 7.000000000000000000 ) ) ;
#19639 = EDGE_CURVE ( 'NONE', #10420, #1897, #38241, .T. ) ;
#19640 = CARTESIAN_POINT ( 'NONE',  ( 34.13230107285825454, -16.19066397787869249, -7.548977151778921701 ) ) ;
#19641 = CARTESIAN_POINT ( 'NONE',  ( 16.88398162953626525, -29.10422986782303667, 12.14047268032943805 ) ) ;
#19642 = ORIENTED_EDGE ( 'NONE', *, *, #37398, .T. ) ;
#19643 = VECTOR ( 'NONE', #18714, 1000.000000000000000 ) ;
#19644 = ORIENTED_EDGE ( 'NONE', *, *, #867, .T. ) ;
#19645 = FACE_OUTER_BOUND ( 'NONE', #30125, .T. ) ;
#19646 = CARTESIAN_POINT ( 'NONE',  ( -7.766013557953293400, 28.81973365084998306, 10.50000000000000000 ) ) ;
#19647 = CIRCLE ( 'NONE', #16406, 0.5000000000000004441 ) ;
#19648 = CARTESIAN_POINT ( 'NONE',  ( -7.577547685840081648, 11.84256962714647798, 6.000000000000000000 ) ) ;
#19649 = ORIENTED_EDGE ( 'NONE', *, *, #38567, .T. ) ;
#19650 = CARTESIAN_POINT ( 'NONE',  ( -0.5026506373464326716, 25.74991689940979711, -19.62692947300378776 ) ) ;
#19651 = DIRECTION ( 'NONE',  ( -0.2079116908177663092, -0.9781476007338041345, 0.000000000000000000 ) ) ;
#19652 = CARTESIAN_POINT ( 'NONE',  ( 12.30736835487432579, 14.81698729810772619, 11.00000000000000000 ) ) ;
#19653 = CARTESIAN_POINT ( 'NONE',  ( 30.33933116650763040, 6.243556997736084746, 11.00000000000000000 ) ) ;
#19654 = DIRECTION ( 'NONE',  ( -0.000000000000000000, -0.000000000000000000, -1.000000000000000000 ) ) ;
#19655 = CIRCLE ( 'NONE', #35236, 0.4999999999999999445 ) ;
#19656 = DIRECTION ( 'NONE',  ( -0.7431448254773846962, 0.6691306063588690067, 0.000000000000000000 ) ) ;
#19657 = CARTESIAN_POINT ( 'NONE',  ( 14.21692097054198634, 29.76874005997475692, -5.917914220045247475 ) ) ;
#19658 = CARTESIAN_POINT ( 'NONE',  ( -13.22516817658055288, 40.70288237343638826, 11.00000000000000000 ) ) ;
#19659 = ORIENTED_EDGE ( 'NONE', *, *, #5773, .F. ) ;
#19661 = DIRECTION ( 'NONE',  ( -0.9135454576426004225, 0.4067366430758009854, -0.000000000000000000 ) ) ;
#19660 = CARTESIAN_POINT ( 'NONE',  ( -16.80464701721349385, 11.74058409121013469, -29.42729362730365494 ) ) ;
#19662 = CLOSED_SHELL ( 'NONE', ( #34324, #26074, #17585, #35242, #3646, #12487, #38404, #29093, #30501, #9135, #30156, #1374, #14698, #15598, #8791, #5293, #17721, #6340, #20987, #18609, #20668, #5894, #35743, #32393, #5448, #28887, #10653, #9179, #38543, #20466, #17964, #29973, #1976, #10262, #12615, #6390, #12497, #13012, #29243, #31357, #19277, #20106, #9366, #36626, #2446, #15099, #22761, #30891, #2920, #26304, #29883, #25510, #36528, #10513, #28229, #4638, #30002, #27379, #31040, #1993, #38439, #39694, #23699, #18240, #13852, #25983, #31110, #10043, #36650, #6112, #28024, #14077, #28342, #2735, #16823, #37101, #16697, #9243, #30026, #23662, #27727, #17746, #17700, #20942, #6298, #10124, #10909, #16766, #29751, #24944, #17462, #33733, #6959, #1169, #33634, #7116, #12370, #33922, #15064, #31098, #19482, #18204, #17889, #38846, #29672, #37403, #30140, #7660, #16203, #27401, #12142, #17050, #1474, #22688, #23171, #15942, #34150, #8015, #34694, #19921, #38741, #22893, #30514, #23780, #2765, #7100, #9394, #20721, #10663, #25724, #6148, #40076, #29250, #23829, #39123, #18581, #24544, #19538, #38547, #5714, #21312, #19814, #30404, #2817, #2074, #38967, #39501, #30191, #21583, #19324, #13856, #21307, #14494, #1820, #34941, #3312, #38100, #22996, #10404, #37051, #29496, #39781, #38719, #34627, #5342, #9912, #3298, #40096, #4145, #10749, #32668, #36582, #1539, #3410, #24044, #28255, #26920, #20545, #30742, #34691, #37731, #4421, #38830, #23693, #28027, #22379, #29878, #30142, #7581, #30207, #1819, #4782, #16753, #39137, #15853, #13643, #6363, #16301, #12890, #563, #17574, #30715, #7767, #3774, #21944, #15523, #21359, #38323, #5661, #24208, #12762, #39349, #32617, #24057, #29039, #23128, #11288, #17488, #12093, #32593, #7148, #7797, #39195, #6837, #19585, #25271, #5849, #37311, #3920, #39645, #39656, #32492, #13243, #36579, #3798, #28687, #8066, #34127, #36226, #27043, #6867, #5270, #29139, #10992, #38610, #33152, #8656, #25996, #25643, #4657, #13135, #1923, #22808, #23206, #37759, #13053, #13089, #36700, #6909, #26409, #27548, #5193, #12263, #5065, #8907, #11409, #32900, #14756, #25152, #28608, #18538, #16074, #26163, #30240, #31223, #25044, #35867, #9521, #38644, #27121, #36446, #6273, #29019, #24812, #596, #13324, #5164, #27635, #39970, #24664, #7527, #26815, #22283, #136, #19792, #18038, #38695, #30847, #11212, #29395, #23963, #32174, #31986, #24446, #10651, #36953, #23640, #35644, #8788, #4914, #9107, #11388, #10239, #16353, #9668, #30740, #3848, #16668, #11713, #27858, #11841, #7765, #36898, #16102, #33889, #27823, #3150, #33126, #11635, #34201, #35721, #39219, #28747, #23331, #31789, #13342, #26454, #35839, #33857, #26491, #36693, #39469, #25672, #517, #34219, #19303, #24209, #28696, #25792, #29381, #35846, #20841, #16445, #18940, #18808, #15568, #30710, #24786, #11371, #15901, #2470, #36398, #4581, #33711, #14711, #5420, #25198, #38441, #8327, #23897, #7011, #38208, #25927, #38409, #26645, #12842, #7394, #1845, #16211, #17917, #33329, #15096, #21240, #14029, #14342, #21754, #9895, #37929, #5146, #13750, #39141, #9337, #35110, #37172, #5167, #3049, #7242, #12722, #18611, #8307, #16432, #9546, #34706, #27272, #3194, #2967, #17097, #27772, #24422, #5563, #28986, #26808, #40130, #28078, #5597, #14298, #25264, #15199, #4430, #23944, #18088, #15208, #12013, #5408, #37678, #15268, #37608, #12245, #12845, #35059, #36125, #19742, #35698, #28890, #18844, #27225, #1322, #34019, #19930, #6621, #34835, #7376, #17989, #5302, #33207, #38102, #39872, #31143, #6442, #26382, #19290, #31665, #6518, #38317, #31437, #23808, #18330, #22254, #18857, #18586, #2937, #17126, #39203, #26098, #32856, #8255, #34591, #1974, #22539, #32967, #2558, #29780, #2373, #35447, #12602, #39676, #10667, #6809, #1473, #2296, #23989, #4201, #30367, #34338, #15850, #21781, #6744, #35864, #9586, #31213, #21036, #32134, #32356, #5967, #6661, #22790, #25753, #16101, #9666, #6759, #36495, #17024, #28231, #40050, #8189, #23177, #30452, #24767, #5287, #3685, #19057, #27390, #36998, #2941, #31557, #9157, #15828, #7346, #10248, #19969, #39077, #28450, #29467, #33411, #4285, #18488, #20563, #25623, #13573, #28904, #10461, #34831, #14566, #28748, #26184, #1400, #31070, #2187, #18213, #12617, #18801, #37131, #62, #30808, #15254, #12642, #13986, #15368, #13216, #36795, #392, #31410, #23502, #8052, #39414, #9378, #37098, #27006, #4375, #40079, #26949, #15696, #28047, #30851, #24315, #35443, #8614, #20005, #2444, #23561, #24841, #38971, #27154 ) ) ;
#19663 = DIRECTION ( 'NONE',  ( -0.000000000000000000, -0.000000000000000000, -1.000000000000000000 ) ) ;
#19664 = EDGE_CURVE ( 'NONE', #21646, #27087, #33737, .T. ) ;
#19665 = CARTESIAN_POINT ( 'NONE',  ( 15.55330811712816796, -26.75926366330655881, -5.473885071091127763 ) ) ;
#19666 = DIRECTION ( 'NONE',  ( 0.5000000000000041078, 0.8660254037844362651, 0.000000000000000000 ) ) ;
#19667 = CARTESIAN_POINT ( 'NONE',  ( 15.38114701770948223, 26.81500699202883808, -5.945400566827167665 ) ) ;
#19668 = CARTESIAN_POINT ( 'NONE',  ( -9.163310636333559245, 20.63632441393290762, -29.99999999999998579 ) ) ;
#19669 = DIRECTION ( 'NONE',  ( -0.6123724356957950254, 0.3535533905932778387, -0.7071067811865450192 ) ) ;
#19670 = VECTOR ( 'NONE', #5277, 1000.000000000000114 ) ;
#19671 = CARTESIAN_POINT ( 'NONE',  ( -14.92586248739858057, -14.88347242730710285, -26.39567461636375612 ) ) ;
#19672 = CARTESIAN_POINT ( 'NONE',  ( 6.239928823093291221, -25.04180554674758596, -6.442187431363892713 ) ) ;
#19673 = CARTESIAN_POINT ( 'NONE',  ( 15.26025490481548452, 25.99765090567122172, -8.299852100227690599 ) ) ;
#19674 = CARTESIAN_POINT ( 'NONE',  ( 20.51130358758450001, 13.93060706563202800, -6.938413485835397410 ) ) ;
#19675 = DIRECTION ( 'NONE',  ( -0.000000000000000000, -0.000000000000000000, 1.000000000000000000 ) ) ;
#19676 = CARTESIAN_POINT ( 'NONE',  ( 4.458865582155095986, 18.48521636184714012, 6.000000000000000000 ) ) ;
#19677 = EDGE_LOOP ( 'NONE', ( #7733, #29082, #37528, #10269 ) ) ;
#19678 = CARTESIAN_POINT ( 'NONE',  ( -9.303379230217553086, 35.08951236559498454, -7.168276996282715530 ) ) ;
#19679 = EDGE_LOOP ( 'NONE', ( #14984, #8244 ) ) ;
#19680 = CONICAL_SURFACE ( 'NONE', #23576, 1.000000000000004441, 0.7853981633974583820 ) ;
#19681 = FACE_OUTER_BOUND ( 'NONE', #32077, .T. ) ;
#19682 = ORIENTED_EDGE ( 'NONE', *, *, #2689, .F. ) ;
#19683 = CARTESIAN_POINT ( 'NONE',  ( 20.81893642488379115, 0.7903601759063493271, -26.82748604854442931 ) ) ;
#19684 = FACE_OUTER_BOUND ( 'NONE', #6857, .T. ) ;
#19685 = ADVANCED_FACE ( 'NONE', ( #16362 ), #9472, .F. ) ;
#19686 = DIRECTION ( 'NONE',  ( 1.000000000000000000, 0.000000000000000000, 0.000000000000000000 ) ) ;
#19687 = ORIENTED_EDGE ( 'NONE', *, *, #31611, .T. ) ;
#19688 = CARTESIAN_POINT ( 'NONE',  ( -27.04348299841949910, 0.3741087672331259162, -14.48585235329367826 ) ) ;
#19689 = EDGE_CURVE ( 'NONE', #4287, #6957, #5158, .T. ) ;
#19690 = CARTESIAN_POINT ( 'NONE',  ( -10.78894649379783388, 21.72623886970244911, 6.000000000000000000 ) ) ;
#19691 = ORIENTED_EDGE ( 'NONE', *, *, #23257, .T. ) ;
#19692 = CARTESIAN_POINT ( 'NONE',  ( 27.20974068289347159, -7.315317279060644218, -16.79268240890852937 ) ) ;
#19693 = VECTOR ( 'NONE', #16967, 999.9999999999998863 ) ;
#19694 = EDGE_CURVE ( 'NONE', #35769, #10247, #6216, .T. ) ;
#19695 = EDGE_CURVE ( 'NONE', #24976, #16279, #34453, .T. ) ;
#19696 = ORIENTED_EDGE ( 'NONE', *, *, #6052, .F. ) ;
#19697 = CARTESIAN_POINT ( 'NONE',  ( 0.000000000000000000, 0.000000000000000000, 0.000000000000000000 ) ) ;
#19698 = CARTESIAN_POINT ( 'NONE',  ( 7.591957726968924014, 38.93640765974104312, 10.99999999999980638 ) ) ;
#19699 = EDGE_CURVE ( 'NONE', #33109, #1261, #15760, .T. ) ;
#19700 = CARTESIAN_POINT ( 'NONE',  ( 8.859192577249615397, 12.20922670554002565, 20.99999999999999645 ) ) ;
#19701 = LINE ( 'NONE', #32094, #5286 ) ;
#19702 = ADVANCED_BREP_SHAPE_REPRESENTATION ( '', ( #8826, #24238 ), #31997 ) ;
#19703 = CARTESIAN_POINT ( 'NONE',  ( -1.248251703783856303, 34.03222469610383172, 19.66345542862528362 ) ) ;
#19704 = AXIS2_PLACEMENT_3D ( 'NONE', #11727, #8679, #30814 ) ;
#19705 = DIRECTION ( 'NONE',  ( 0.000000000000000000, 0.000000000000000000, 1.000000000000000000 ) ) ;
#19706 = EDGE_LOOP ( 'NONE', ( #3258, #1141, #33591 ) ) ;
#19707 = CARTESIAN_POINT ( 'NONE',  ( -1.541676259743169464, 20.48416492902245167, -30.00000000000001421 ) ) ;
#19708 = DIRECTION ( 'NONE',  ( 0.2185080122244179301, 0.6724985119639563802, 0.7071067811865462405 ) ) ;
#19709 = DIRECTION ( 'NONE',  ( 0.000000000000000000, 0.000000000000000000, 1.000000000000000000 ) ) ;
#19710 = CARTESIAN_POINT ( 'NONE',  ( 17.19287287506014295, 19.26288574755855620, -10.79497166203956660 ) ) ;
#19711 = CARTESIAN_POINT ( 'NONE',  ( 6.954109223000227047, 24.07807191830993077, -19.86921157130286275 ) ) ;
#19712 = VECTOR ( 'NONE', #10105, 1000.000000000000114 ) ;
#19713 = ORIENTED_EDGE ( 'NONE', *, *, #37200, .T. ) ;
#19714 = DIRECTION ( 'NONE',  ( 1.000000000000000000, 0.000000000000000000, 0.000000000000000000 ) ) ;
#19715 = EDGE_CURVE ( 'NONE', #7574, #36335, #14907, .T. ) ;
#19716 = DIRECTION ( 'NONE',  ( 1.000000000000000000, 0.000000000000000000, 0.000000000000000000 ) ) ;
#19717 = EDGE_CURVE ( 'NONE', #31091, #1084, #3961, .T. ) ;
#19718 = EDGE_CURVE ( 'NONE', #29442, #22687, #31008, .T. ) ;
#19719 = CARTESIAN_POINT ( 'NONE',  ( 10.01866435034643743, -18.04234178223556029, -28.05214097278188490 ) ) ;
#19720 = CARTESIAN_POINT ( 'NONE',  ( 13.05736835487433289, 16.11602540378438420, 7.499999999999997335 ) ) ;
#19721 = CARTESIAN_POINT ( 'NONE',  ( 2.036571916123615100, 8.108948098542045457, 11.00000000000000000 ) ) ;
#19722 = ORIENTED_EDGE ( 'NONE', *, *, #25769, .T. ) ;
#19723 = CARTESIAN_POINT ( 'NONE',  ( -14.53535404462992098, 24.96185776678678891, -11.59977167594924019 ) ) ;
#19724 = CIRCLE ( 'NONE', #35973, 1.000000000000000000 ) ;
#19725 = CARTESIAN_POINT ( 'NONE',  ( -15.60391421430763437, -26.29546805949255983, 16.87380292611441490 ) ) ;
#19726 = CARTESIAN_POINT ( 'NONE',  ( 10.46771542449441306, -20.07731438429163617, -21.66176537328637508 ) ) ;
#19727 = FACE_OUTER_BOUND ( 'NONE', #22138, .T. ) ;
#19728 = VERTEX_POINT ( 'NONE', #27951 ) ;
#19729 = VERTEX_POINT ( 'NONE', #18621 ) ;
#19730 = CARTESIAN_POINT ( 'NONE',  ( -9.705446205519352887, 20.57320699630038519, -22.42486721958433549 ) ) ;
#19731 = CARTESIAN_POINT ( 'NONE',  ( -8.935776944912362296, 22.65328985282726393, 6.000000000000000000 ) ) ;
#19732 = CARTESIAN_POINT ( 'NONE',  ( 0.000000000000000000, 22.50000000000000355, 13.00000000000000178 ) ) ;
#19733 = MECHANICAL_DESIGN_GEOMETRIC_PRESENTATION_REPRESENTATION (  '', ( #8047 ), #12601 ) ;
#19734 = CARTESIAN_POINT ( 'NONE',  ( -21.94754318934862169, -4.722844451827508117, -23.27871882223563205 ) ) ;
#19735 = DIRECTION ( 'NONE',  ( -0.000000000000000000, -0.000000000000000000, -1.000000000000000000 ) ) ;
#19736 = ORIENTED_EDGE ( 'NONE', *, *, #17283, .F. ) ;
#19737 = CARTESIAN_POINT ( 'NONE',  ( 30.70366785093425932, 0.06005377067882849973, -6.417126122636190644 ) ) ;
#19738 = CARTESIAN_POINT ( 'NONE',  ( 15.41558956916364842, 26.78481017491955285, -5.948412119462402003 ) ) ;
#19739 = CARTESIAN_POINT ( 'NONE',  ( 14.81329996725644271, 19.93755115561686964, 10.49999999999999822 ) ) ;
#19740 = ORIENTED_EDGE ( 'NONE', *, *, #4039, .F. ) ;
#19741 = CARTESIAN_POINT ( 'NONE',  ( -30.79516076619654896, -0.03407914214386141560, -6.416988314164135510 ) ) ;
#19742 = ADVANCED_FACE ( 'NONE', ( #125 ), #26585, .T. ) ;
#19743 = CARTESIAN_POINT ( 'NONE',  ( -5.132330917503045598, 36.34800796123247579, 10.49999999999999822 ) ) ;
#19744 = VERTEX_POINT ( 'NONE', #22052 ) ;
#19745 = CARTESIAN_POINT ( 'NONE',  ( 30.29736254084309621, -2.797781772719168725, -12.30903580646858941 ) ) ;
#19746 = VECTOR ( 'NONE', #33858, 1000.000000000000000 ) ;
#19747 = CARTESIAN_POINT ( 'NONE',  ( 20.21580222128064364, 3.470454069710441569, -30.00000000000000355 ) ) ;
#19748 = CARTESIAN_POINT ( 'NONE',  ( 31.31527935466855439, -1.911037205180780019, 17.42190598798589107 ) ) ;
#19749 = EDGE_LOOP ( 'NONE', ( #7182, #13144 ) ) ;
#19750 = CARTESIAN_POINT ( 'NONE',  ( 9.684793793941290474, 35.24386573278109580, 16.30093088680190405 ) ) ;
#19751 = DIRECTION ( 'NONE',  ( 1.000000000000000000, 0.000000000000000000, -0.000000000000000000 ) ) ;
#19752 = CARTESIAN_POINT ( 'NONE',  ( 5.469228652589973372, 26.20992143183299916, 20.94377226548378701 ) ) ;
#19753 = CYLINDRICAL_SURFACE ( 'NONE', #5129, 1.000000000000000000 ) ;
#19754 = FACE_OUTER_BOUND ( 'NONE', #29884, .T. ) ;
#19755 = B_SPLINE_SURFACE_WITH_KNOTS ( 'NONE', 1, 3, ( 
 ( #7137, #32344, #31926, #13642, #13436, #19743, #3159, #29288, #29084, #27937 ),
 ( #24689, #26030, #21639, #15550, #12496, #9459, #5305, #23596, #11408, #35992 ) ),
 .UNSPECIFIED., .F., .F., .F.,
 ( 2, 2 ),
 ( 4, 2, 2, 2, 4 ),
 ( 0.000000000000000000, 1.000000000000000000 ),
 ( 1.265795420569479912, 1.658494502268205162, 2.051193583966930412, 2.443892665665655439, 2.836591747364380467 ),
 .UNSPECIFIED. ) ;
#19756 = AXIS2_PLACEMENT_3D ( 'NONE', #26211, #23573, #27019 ) ;
#19757 = FACE_BOUND ( 'NONE', #23368, .T. ) ;
#19758 = CARTESIAN_POINT ( 'NONE',  ( 22.71318823113102070, 6.927825590551851320, 17.92354375535233046 ) ) ;
#19759 = CARTESIAN_POINT ( 'NONE',  ( -19.49657363026103951, 7.925481962114715451, -24.37616138078942640 ) ) ;
#19760 = ADVANCED_FACE ( 'NONE', ( #25302 ), #6600, .F. ) ;
#19761 = CARTESIAN_POINT ( 'NONE',  ( 14.87465728246612606, -18.53959208443260920, -21.11850284650765275 ) ) ;
#19762 = VECTOR ( 'NONE', #21858, 1000.000000000000000 ) ;
#19763 = CARTESIAN_POINT ( 'NONE',  ( -20.57924982997939622, -27.21273881503329051, -4.999999999999998224 ) ) ;
#19764 =( BOUNDED_CURVE ( )  B_SPLINE_CURVE ( 2, ( #39869, #12046, #36829 ),
 .UNSPECIFIED., .F., .F. ) 
 B_SPLINE_CURVE_WITH_KNOTS ( ( 3, 3 ),
 ( 0.000000000000000000, 1.000000000000000000 ),
 .UNSPECIFIED. ) 
 CURVE ( )  GEOMETRIC_REPRESENTATION_ITEM ( )  RATIONAL_B_SPLINE_CURVE ( ( 1.000000000000000000, 0.7071067811865475727, 1.000000000000000000 ) ) 
 REPRESENTATION_ITEM ( '' )  );
#19765 = VERTEX_POINT ( 'NONE', #34648 ) ;
#19766 = CARTESIAN_POINT ( 'NONE',  ( 13.96311103245068175, 24.09699048448357317, -13.49799974867627661 ) ) ;
#19767 = VERTEX_POINT ( 'NONE', #31592 ) ;
#19768 = VECTOR ( 'NONE', #23152, 1000.000000000000000 ) ;
#19769 = CARTESIAN_POINT ( 'NONE',  ( -12.28865036616621786, 17.24410649058709311, -25.13873084831685745 ) ) ;
#19770 = CARTESIAN_POINT ( 'NONE',  ( -28.04602290581260959, -19.07745245555469893, 19.66345542862529783 ) ) ;
#19771 = LINE ( 'NONE', #18970, #32185 ) ;
#19772 = CARTESIAN_POINT ( 'NONE',  ( 11.03067133885425655, 17.27930474757444657, -30.00000000000000000 ) ) ;
#19773 = ORIENTED_EDGE ( 'NONE', *, *, #15585, .F. ) ;
#19774 = CARTESIAN_POINT ( 'NONE',  ( 31.66152258591498736, -17.45444667796995120, -10.17335708870760946 ) ) ;
#19775 = FACE_OUTER_BOUND ( 'NONE', #26825, .T. ) ;
#19776 = ORIENTED_EDGE ( 'NONE', *, *, #34447, .F. ) ;
#19778 = CARTESIAN_POINT ( 'NONE',  ( -22.37674264578614469, 24.85189042352228839, 11.00000000000000000 ) ) ;
#19777 = CARTESIAN_POINT ( 'NONE',  ( -10.78183262531012154, 17.59235075900286915, -28.06201921541798328 ) ) ;
#19779 = CARTESIAN_POINT ( 'NONE',  ( -16.75447718561904864, -27.02424154557581915, -5.000000000000000000 ) ) ;
#19780 = CARTESIAN_POINT ( 'NONE',  ( 14.26584437371809777, 27.13525491562438319, 13.00000000000000178 ) ) ;
#19781 = ORIENTED_EDGE ( 'NONE', *, *, #22669, .T. ) ;
#19782 = CARTESIAN_POINT ( 'NONE',  ( -28.46622419312624430, -12.75272502055737434, -14.74906803505498765 ) ) ;
#19783 = CARTESIAN_POINT ( 'NONE',  ( -11.69238095878992745, -22.55098709441451632, -16.51565108365196721 ) ) ;
#19784 = DIRECTION ( 'NONE',  ( 1.000000000000000000, 0.000000000000000000, 0.000000000000000000 ) ) ;
#19785 = CARTESIAN_POINT ( 'NONE',  ( 13.21519265033025370, 15.68751749194264811, -30.00000000000001066 ) ) ;
#19786 = ORIENTED_EDGE ( 'NONE', *, *, #36332, .T. ) ;
#19787 = CARTESIAN_POINT ( 'NONE',  ( 27.78359518671923212, 2.894372651951440112, -8.330351127553241142 ) ) ;
#19788 = DIRECTION ( 'NONE',  ( 0.6123724356957886972, -0.3535533905932740639, -0.7071067811865525687 ) ) ;
#19789 = DIRECTION ( 'NONE',  ( 0.000000000000000000, 0.000000000000000000, 1.000000000000000000 ) ) ;
#19790 = VERTEX_POINT ( 'NONE', #3761 ) ;
#19791 = CARTESIAN_POINT ( 'NONE',  ( -26.62727581776185559, 0.09304277698053113610, -15.42802191721595406 ) ) ;
#19792 = ADVANCED_FACE ( 'NONE', ( #8016 ), #35454, .F. ) ;
#19793 = AXIS2_PLACEMENT_3D ( 'NONE', #20690, #23523, #35312 ) ;
#19794 = CARTESIAN_POINT ( 'NONE',  ( 31.41207073737789557, -0.7790156937066328169, -6.867375471341749638 ) ) ;
#19795 = EDGE_CURVE ( 'NONE', #29833, #29063, #2577, .T. ) ;
#19796 = CARTESIAN_POINT ( 'NONE',  ( 17.00801676779564886, -20.85310720624810088, 20.25080042701566541 ) ) ;
#19797 = ORIENTED_EDGE ( 'NONE', *, *, #25637, .T. ) ;
#19798 = EDGE_CURVE ( 'NONE', #3673, #21859, #16566, .T. ) ;
#19799 = CIRCLE ( 'NONE', #14639, 1.000000000000000000 ) ;
#19800 = CARTESIAN_POINT ( 'NONE',  ( -21.88444403592365362, 6.126538576424530369, -30.00000000000001066 ) ) ;
#19801 = CARTESIAN_POINT ( 'NONE',  ( 9.736411649803228485, 11.65093146000192625, 7.000000000000000000 ) ) ;
#19802 = AXIS2_PLACEMENT_3D ( 'NONE', #31450, #13354, #18863 ) ;
#19803 = EDGE_CURVE ( 'NONE', #35819, #4586, #20219, .T. ) ;
#19804 = AXIS2_PLACEMENT_3D ( 'NONE', #1908, #36031, #1294 ) ;
#19805 = DIRECTION ( 'NONE',  ( 1.000000000000000000, 0.000000000000000000, 0.000000000000000000 ) ) ;
#19806 = CARTESIAN_POINT ( 'NONE',  ( -5.348113209407908464, 9.835177808069893501, 12.00000000000000000 ) ) ;
#19807 = CARTESIAN_POINT ( 'NONE',  ( -11.25022250131745771, 31.95692947463384925, 10.96580508970282963 ) ) ;
#19808 = CARTESIAN_POINT ( 'NONE',  ( -8.238488885696254371, 24.65111619403957022, 9.000000000000001776 ) ) ;
#19809 = FACE_OUTER_BOUND ( 'NONE', #35638, .T. ) ;
#19810 = VERTEX_POINT ( 'NONE', #14113 ) ;
#19811 = FACE_OUTER_BOUND ( 'NONE', #14523, .T. ) ;
#19812 = CYLINDRICAL_SURFACE ( 'NONE', #27222, 1.000000000000000000 ) ;
#19813 = CARTESIAN_POINT ( 'NONE',  ( 27.32249163041963413, -25.19218879630926367, -5.869363991529141344 ) ) ;
#19814 = ADVANCED_FACE ( 'NONE', ( #7203 ), #29155, .T. ) ;
#19815 = EDGE_CURVE ( 'NONE', #18376, #30328, #37607, .T. ) ;
#19816 = DIRECTION ( 'NONE',  ( 1.000000000000000000, 0.000000000000000000, 0.000000000000000000 ) ) ;
#19817 = DIRECTION ( 'NONE',  ( 1.000000000000000000, 0.000000000000000000, 0.000000000000000000 ) ) ;
#19818 = EDGE_CURVE ( 'NONE', #13994, #31871, #1325, .T. ) ;
#19819 = CIRCLE ( 'NONE', #16571, 0.5000000000000004441 ) ;
#19820 = CARTESIAN_POINT ( 'NONE',  ( 10.51082547654175059, 17.86856945860100865, -27.40418496694546135 ) ) ;
#19821 =( NAMED_UNIT ( * ) PLANE_ANGLE_UNIT ( ) SI_UNIT ( $, .RADIAN. ) );
#19822 = VERTEX_POINT ( 'NONE', #29556 ) ;
#19823 = CARTESIAN_POINT ( 'NONE',  ( -16.96185042632790640, 20.08371563433640716, -10.29097588471536362 ) ) ;
#19824 = FACE_OUTER_BOUND ( 'NONE', #34891, .T. ) ;
#19825 = CARTESIAN_POINT ( 'NONE',  ( 9.484687302133613329, -18.22422652986723079, -28.70838076812352213 ) ) ;
#19826 = CARTESIAN_POINT ( 'NONE',  ( 30.90412082983250741, -0.04211290444289944590, -5.000000000000000000 ) ) ;
#19827 = CARTESIAN_POINT ( 'NONE',  ( 11.01823919507857141, 17.34030634537447213, -28.70746280985912691 ) ) ;
#19828 = ORIENTED_EDGE ( 'NONE', *, *, #34478, .T. ) ;
#19829 = CARTESIAN_POINT ( 'NONE',  ( 15.39658735393897437, 26.76009586085592673, -5.946078209756686661 ) ) ;
#19830 = EDGE_LOOP ( 'NONE', ( #4708, #1758, #20912, #33149 ) ) ;
#19832 = DIRECTION ( 'NONE',  ( -1.000000000000000000, 0.000000000000000000, 0.000000000000000000 ) ) ;
#19831 = CARTESIAN_POINT ( 'NONE',  ( -15.06796771947636771, 26.24911050298840820, -8.762714437537596268 ) ) ;
#19833 = CARTESIAN_POINT ( 'NONE',  ( -10.22236381303094532, -19.16528309895199556, -23.85432085113489364 ) ) ;
#19834 = CARTESIAN_POINT ( 'NONE',  ( -34.83527399001564362, -1.648960735037901637, 10.99999999999971045 ) ) ;
#19835 = VECTOR ( 'NONE', #13911, 1000.000000000000000 ) ;
#19836 = CIRCLE ( 'NONE', #23077, 1.000000000000000888 ) ;
#19837 = CARTESIAN_POINT ( 'NONE',  ( -32.98459937871956527, -19.91850110786283423, -5.435368959122942378 ) ) ;
#19838 = CARTESIAN_POINT ( 'NONE',  ( -4.803568943853530726, -24.90644357294165090, -5.962994550823584206 ) ) ;
#19839 = CARTESIAN_POINT ( 'NONE',  ( 12.41354392755694391, 18.82514156286238105, -21.70496632052628527 ) ) ;
#19840 = ORIENTED_EDGE ( 'NONE', *, *, #8773, .F. ) ;
#19841 = CARTESIAN_POINT ( 'NONE',  ( 19.02940903860087829, 8.038401761433641823, -27.15973525649786779 ) ) ;
#19842 = CARTESIAN_POINT ( 'NONE',  ( 0.000000000000000000, 22.50000000000000355, 7.000000000000000000 ) ) ;
#19843 = DIRECTION ( 'NONE',  ( 1.000000000000000000, 0.000000000000000000, 0.000000000000000000 ) ) ;
#19844 = CARTESIAN_POINT ( 'NONE',  ( -14.43694901005348719, 26.51279404187317112, 17.42190598798392642 ) ) ;
#19845 = EDGE_LOOP ( 'NONE', ( #36463, #26485 ) ) ;
#19846 = CARTESIAN_POINT ( 'NONE',  ( -31.09817132049496280, -1.548763601471955464, -9.610625396712832114 ) ) ;
#19847 = ADVANCED_FACE ( 'NONE', ( #38902 ), #11078, .F. ) ;
#19848 = PLANE ( 'NONE',  #6612 ) ;
#19849 = VERTEX_POINT ( 'NONE', #4571 ) ;
#19850 = EDGE_CURVE ( 'NONE', #7138, #7015, #35854, .T. ) ;
#19851 = CYLINDRICAL_SURFACE ( 'NONE', #40035, 0.5000000000000004441 ) ;
#19852 = CARTESIAN_POINT ( 'NONE',  ( -3.607749162633400619, 7.931741834401826452, 10.50000000000000000 ) ) ;
#19853 = B_SPLINE_CURVE_WITH_KNOTS ( 'NONE', 3,
 ( #15272, #18133, #36808, #27263 ),
 .UNSPECIFIED., .F., .F.,
 ( 4, 4 ),
 ( 0.000000000000000000, 1.000000000000000000 ),
 .UNSPECIFIED. ) ;
#19854 = CARTESIAN_POINT ( 'NONE',  ( 33.95719716996227078, -16.10408066851575626, -7.976629801705419354 ) ) ;
#19855 = CARTESIAN_POINT ( 'NONE',  ( 36.74707368630884474, -16.71203845619544026, 11.55979286843918885 ) ) ;
#19856 = ORIENTED_EDGE ( 'NONE', *, *, #28150, .F. ) ;
#19857 = CARTESIAN_POINT ( 'NONE',  ( 13.63581098909226519, 27.45627467658428600, 11.00000000000000000 ) ) ;
#19858 = VECTOR ( 'NONE', #32780, 1000.000000000000000 ) ;
#19859 = CARTESIAN_POINT ( 'NONE',  ( 0.000000000000000000, 22.50000000000000355, 7.000000000000000000 ) ) ;
#19860 = AXIS2_PLACEMENT_3D ( 'NONE', #22701, #775, #24408 ) ;
#19861 = VECTOR ( 'NONE', #8124, 999.9999999999998863 ) ;
#19862 = DIRECTION ( 'NONE',  ( 0.000000000000000000, -0.000000000000000000, -1.000000000000000000 ) ) ;
#19863 = VERTEX_POINT ( 'NONE', #23462 ) ;
#19864 = CARTESIAN_POINT ( 'NONE',  ( -1.787501278500105206, 35.33670910843994761, -11.06934470569155415 ) ) ;
#19865 = CARTESIAN_POINT ( 'NONE',  ( -13.81813021740780201, 28.33725983961547001, 7.102474990965858659 ) ) ;
#19866 = VECTOR ( 'NONE', #14978, 1000.000000000000000 ) ;
#19867 = CARTESIAN_POINT ( 'NONE',  ( -10.41268156625113228, 18.79179606750104981, 6.000000000000000000 ) ) ;
#19868 = FACE_OUTER_BOUND ( 'NONE', #20410, .T. ) ;
#19869 = CARTESIAN_POINT ( 'NONE',  ( 10.33795143809920170, 20.40792924032133016, 11.00000000000000000 ) ) ;
#19870 = CARTESIAN_POINT ( 'NONE',  ( 9.337241587065685522, 10.76617146908747991, 10.49999999999999467 ) ) ;
#19871 = CARTESIAN_POINT ( 'NONE',  ( 13.06030798789831948, 27.04582189987735319, -12.35125024899165780 ) ) ;
#19872 = CARTESIAN_POINT ( 'NONE',  ( 33.51290647813760870, -3.280245463519940063, -4.999999999999999112 ) ) ;
#19873 = ORIENTED_EDGE ( 'NONE', *, *, #33108, .T. ) ;
#19875 = DIRECTION ( 'NONE',  ( 0.1470157664652038954, 0.6916548014802263999, -0.7071067811865456854 ) ) ;
#19874 = CARTESIAN_POINT ( 'NONE',  ( -19.55823056015679384, 15.51636888105696066, -7.909696038444731236 ) ) ;
#19876 = CARTESIAN_POINT ( 'NONE',  ( -12.80736835487442349, 15.68301270189233954, 11.00000000000000000 ) ) ;
#19877 = CARTESIAN_POINT ( 'NONE',  ( 9.532625661562562414, -18.14880370279404076, -30.00000000000000000 ) ) ;
#19878 = CARTESIAN_POINT ( 'NONE',  ( -13.63581098909220302, 27.45627467658446719, 11.00000000000000000 ) ) ;
#19879 = CARTESIAN_POINT ( 'NONE',  ( 13.47022650129216537, 22.85893131970043868, -15.44577212985798198 ) ) ;
#19880 = CARTESIAN_POINT ( 'NONE',  ( -33.62187204924172335, 0.04418559750806146796, -5.000000000000000000 ) ) ;
#19881 = DIRECTION ( 'NONE',  ( 0.000000000000000000, 0.000000000000000000, 1.000000000000000000 ) ) ;
#19882 = CARTESIAN_POINT ( 'NONE',  ( -28.06200121101475986, -24.80525908879649322, -5.000000000000006217 ) ) ;
#19883 = CARTESIAN_POINT ( 'NONE',  ( 6.004260983034707344, -24.46000915886378735, -10.33918878589541102 ) ) ;
#19884 = CARTESIAN_POINT ( 'NONE',  ( 12.22994242602892712, 19.80693455908184930, -20.55844498058446135 ) ) ;
#19885 = CARTESIAN_POINT ( 'NONE',  ( 18.83106894595607983, 13.86228728257169962, -14.90432550276213242 ) ) ;
#19886 = DIRECTION ( 'NONE',  ( -0.2079116908177664480, -0.9781476007338042455, 0.000000000000000000 ) ) ;
#19887 = CARTESIAN_POINT ( 'NONE',  ( 1.000000000000000000, 37.00000000000000711, 7.500000000000000888 ) ) ;
#19888 = ORIENTED_EDGE ( 'NONE', *, *, #23709, .T. ) ;
#19889 = CARTESIAN_POINT ( 'NONE',  ( -9.351165396203874991, 35.32073807392316667, -6.306370732072846153 ) ) ;
#19890 = ORIENTED_EDGE ( 'NONE', *, *, #15000, .T. ) ;
#19891 = CARTESIAN_POINT ( 'NONE',  ( -15.33953269408914544, -26.67883706601617888, -5.946098135196418610 ) ) ;
#19892 = AXIS2_PLACEMENT_3D ( 'NONE', #5788, #2742, #15134 ) ;
#19893 = DIRECTION ( 'NONE',  ( 1.000000000000000000, 0.000000000000000000, 0.000000000000000000 ) ) ;
#19894 = VERTEX_POINT ( 'NONE', #4773 ) ;
#19895 = CARTESIAN_POINT ( 'NONE',  ( 30.03307712974922339, -0.01506494207477212556, -9.235894060447490617 ) ) ;
#19896 = DIRECTION ( 'NONE',  ( -1.000000000000000000, 0.000000000000000000, 0.000000000000000000 ) ) ;
#19897 = DIRECTION ( 'NONE',  ( 0.000000000000000000, 0.000000000000000000, 1.000000000000000000 ) ) ;
#19898 = ORIENTED_EDGE ( 'NONE', *, *, #12103, .F. ) ;
#19899 = CARTESIAN_POINT ( 'NONE',  ( -21.69376705123304561, 0.8088866752443155672, -23.86354191580900874 ) ) ;
#19900 = ORIENTED_EDGE ( 'NONE', *, *, #39075, .T. ) ;
#19901 = CARTESIAN_POINT ( 'NONE',  ( 31.75158787230413537, -7.547111399419645039, -12.10492256910596431 ) ) ;
#19902 = EDGE_LOOP ( 'NONE', ( #27584, #3047, #3871, #6186 ) ) ;
#19903 = DIRECTION ( 'NONE',  ( 1.000000000000000000, 0.000000000000000000, 0.000000000000000000 ) ) ;
#19904 = CARTESIAN_POINT ( 'NONE',  ( -10.89111091687339083, 36.83121428896948402, 10.99999999999999467 ) ) ;
#19905 = CARTESIAN_POINT ( 'NONE',  ( 6.354454053420414361, 35.54304081427980577, 7.500000000000000888 ) ) ;
#19906 = CARTESIAN_POINT ( 'NONE',  ( -9.892954722048926897, 20.95745441963942568, 10.50000000000000000 ) ) ;
#19907 = CARTESIAN_POINT ( 'NONE',  ( -2.974899668820556009, 35.98612526451936589, 18.42518152272109688 ) ) ;
#19908 = CARTESIAN_POINT ( 'NONE',  ( 9.126760388790467360, 17.80801270189218144, 10.74999999999999467 ) ) ;
#19909 = EDGE_LOOP ( 'NONE', ( #24046, #413, #38974, #38716 ) ) ;
#19910 = FILL_AREA_STYLE_COLOUR ( '', #31358 ) ;
#19911 = LINE ( 'NONE', #32307, #36628 ) ;
#19912 = DIRECTION ( 'NONE',  ( -0.4731467892558146038, -0.5254827454987658353, -0.7071067811865425767 ) ) ;
#19913 = DIRECTION ( 'NONE',  ( 0.000000000000000000, 0.000000000000000000, 1.000000000000000000 ) ) ;
#19914 = CARTESIAN_POINT ( 'NONE',  ( 17.94915298279187965, 17.13629230656877667, -11.82338326548747887 ) ) ;
#19915 = AXIS2_PLACEMENT_3D ( 'NONE', #29788, #39526, #2753 ) ;
#19916 = CARTESIAN_POINT ( 'NONE',  ( 9.390451618560783587, 29.18342345638610880, -13.98827517472965098 ) ) ;
#19917 = VECTOR ( 'NONE', #29024, 1000.000000000000227 ) ;
#19918 = ORIENTED_EDGE ( 'NONE', *, *, #15922, .F. ) ;
#19919 = FACE_OUTER_BOUND ( 'NONE', #9556, .T. ) ;
#19920 = LINE ( 'NONE', #12663, #28540 ) ;
#19921 = ADVANCED_FACE ( 'NONE', ( #7407 ), #20017, .T. ) ;
#19922 = CARTESIAN_POINT ( 'NONE',  ( 16.10068483903742376, -26.35529856002330718, -8.725391069711090353 ) ) ;
#19923 = DIRECTION ( 'NONE',  ( -0.000000000000000000, -0.000000000000000000, -1.000000000000000000 ) ) ;
#19924 = DIRECTION ( 'NONE',  ( 0.000000000000000000, 0.000000000000000000, 1.000000000000000000 ) ) ;
#19925 = ORIENTED_EDGE ( 'NONE', *, *, #35228, .F. ) ;
#19926 = CONICAL_SURFACE ( 'NONE', #9576, 1.000000000000000444, 0.7853981633974482790 ) ;
#19927 = CARTESIAN_POINT ( 'NONE',  ( -15.41919230091076187, 26.77186013819068577, -5.474270845225373883 ) ) ;
#19928 = CARTESIAN_POINT ( 'NONE',  ( -35.60445263620085399, -7.407141432649139823, 15.72805884748857963 ) ) ;
#19929 = CARTESIAN_POINT ( 'NONE',  ( 14.73589040286153562, -26.36289149956793310, -7.360008916301447712 ) ) ;
#19930 = ADVANCED_FACE ( 'NONE', ( #4975 ), #19441, .T. ) ;
#19931 = DIRECTION ( 'NONE',  ( -0.9510565162951503115, 0.3090169943749572767, 0.000000000000000000 ) ) ;
#19932 = EDGE_CURVE ( 'NONE', #34769, #11836, #1805, .T. ) ;
#19933 = ORIENTED_EDGE ( 'NONE', *, *, #12220, .F. ) ;
#19934 = VERTEX_POINT ( 'NONE', #38495 ) ;
#19935 = CARTESIAN_POINT ( 'NONE',  ( -9.018867048779389606, 18.89568106175847362, -26.64054324667225160 ) ) ;
#19936 = CARTESIAN_POINT ( 'NONE',  ( -12.22510875462229762, -16.67830573107660541, -27.92440096918162595 ) ) ;
#19937 = CARTESIAN_POINT ( 'NONE',  ( -12.47058434440077512, 14.72275450261881602, 10.96580508970281187 ) ) ;
#19938 = CARTESIAN_POINT ( 'NONE',  ( -35.08557715296313262, -7.694570891656546507, -5.446627638814927508 ) ) ;
#19939 = PLANE ( 'NONE',  #31254 ) ;
#19940 = ORIENTED_EDGE ( 'NONE', *, *, #40176, .F. ) ;
#19941 = CARTESIAN_POINT ( 'NONE',  ( 26.42155565230272529, 0.4047387329622965657, -15.46047363215482129 ) ) ;
#19942 = DIRECTION ( 'NONE',  ( -1.000000000000000000, 0.000000000000000000, 0.000000000000000000 ) ) ;
#19943 = CARTESIAN_POINT ( 'NONE',  ( -7.294006203984644721, 33.46401007850805343, 13.00000000000000178 ) ) ;
#19944 = ORIENTED_EDGE ( 'NONE', *, *, #23794, .F. ) ;
#19945 = CARTESIAN_POINT ( 'NONE',  ( -21.27851422119422153, 0.7607673571408221092, -25.01294376240213779 ) ) ;
#19946 = CARTESIAN_POINT ( 'NONE',  ( -5.198706521309195416, 29.65540566576573767, 9.000000000000001776 ) ) ;
#19947 = ORIENTED_EDGE ( 'NONE', *, *, #26148, .F. ) ;
#19948 = CARTESIAN_POINT ( 'NONE',  ( 33.15613636589012003, -3.183923766461477012, -6.816378949858656888 ) ) ;
#19949 = VECTOR ( 'NONE', #33986, 1000.000000000000000 ) ;
#19950 = VECTOR ( 'NONE', #21682, 1000.000000000000114 ) ;
#19951 = DIRECTION ( 'NONE',  ( -0.000000000000000000, -0.000000000000000000, -1.000000000000000000 ) ) ;
#19952 = CARTESIAN_POINT ( 'NONE',  ( 15.27443809245941786, -27.57253143578273935, 15.13084544680213561 ) ) ;
#19953 = EDGE_CURVE ( 'NONE', #12151, #7227, #39540, .T. ) ;
#19954 = VERTEX_POINT ( 'NONE', #10875 ) ;
#19955 = CARTESIAN_POINT ( 'NONE',  ( 12.27396990952286160, 32.91879577929221057, 16.30093088680193958 ) ) ;
#19956 = ADVANCED_FACE ( 'NONE', ( #38293 ), #19812, .F. ) ;
#19957 = CARTESIAN_POINT ( 'NONE',  ( 16.80389827882579112, -21.64427909826065743, 19.99202127657103389 ) ) ;
#19958 = DIRECTION ( 'NONE',  ( 0.000000000000000000, 0.000000000000000000, 1.000000000000000000 ) ) ;
#19959 = CARTESIAN_POINT ( 'NONE',  ( -7.164929079094340736, 24.49151390636721715, 20.82122704794079837 ) ) ;
#19960 = AXIS2_PLACEMENT_3D ( 'NONE', #3740, #28129, #7939 ) ;
#19961 = DIRECTION ( 'NONE',  ( 0.000000000000000000, 0.000000000000000000, 1.000000000000000000 ) ) ;
#19962 = CARTESIAN_POINT ( 'NONE',  ( -8.189058612310551766, 9.932416477787068487, 7.455686640544901600 ) ) ;
#19963 = DIRECTION ( 'NONE',  ( 1.000000000000000000, 0.000000000000000000, 0.000000000000000000 ) ) ;
#19964 = CARTESIAN_POINT ( 'NONE',  ( 12.55429062394625994, 25.98950339721545788, 18.87996532025784546 ) ) ;
#19965 = CARTESIAN_POINT ( 'NONE',  ( -22.18267962388761205, 8.601427261759537757, -13.87176402086122096 ) ) ;
#19966 = CARTESIAN_POINT ( 'NONE',  ( 20.32386968494314772, -26.55043266981761718, -8.585248161735293593 ) ) ;
#19967 = CIRCLE ( 'NONE', #30359, 1.000000000000000000 ) ;
#19968 = FACE_OUTER_BOUND ( 'NONE', #5472, .T. ) ;
#19969 = ADVANCED_FACE ( 'NONE', ( #13914 ), #26308, .T. ) ;
#19970 = ORIENTED_EDGE ( 'NONE', *, *, #39168, .T. ) ;
#19971 = CARTESIAN_POINT ( 'NONE',  ( 11.01761205127317211, 17.68717171916146214, -26.82030036599024569 ) ) ;
#19972 = AXIS2_PLACEMENT_3D ( 'NONE', #34731, #22934, #19686 ) ;
#19973 = VERTEX_POINT ( 'NONE', #9025 ) ;
#19975 = CIRCLE ( 'NONE', #21282, 0.4999999999999997224 ) ;
#19974 = CARTESIAN_POINT ( 'NONE',  ( -11.90029320544120139, 17.22241791299109792, -26.29854751065716201 ) ) ;
#19976 = CARTESIAN_POINT ( 'NONE',  ( -23.94831201522144326, -21.88372720616936817, 19.66345542862529072 ) ) ;
#19977 = CARTESIAN_POINT ( 'NONE',  ( -14.39395135575592377, 26.65114718998442811, 10.68306085400104699 ) ) ;
#19978 = CARTESIAN_POINT ( 'NONE',  ( 11.03067133885425655, 17.27930474757444657, -29.34935180445048886 ) ) ;
#19979 = ORIENTED_EDGE ( 'NONE', *, *, #14965, .T. ) ;
#19980 = CARTESIAN_POINT ( 'NONE',  ( 33.48737131668896438, -18.46746012246179802, -6.696811483700092715 ) ) ;
#19981 = DIRECTION ( 'NONE',  ( 0.9510565162951497564, -0.3090169943749591086, 0.000000000000000000 ) ) ;
#19982 = ORIENTED_EDGE ( 'NONE', *, *, #6115, .T. ) ;
#19983 = CIRCLE ( 'NONE', #1836, 0.5000000000000001110 ) ;
#19985 = DIRECTION ( 'NONE',  ( 0.000000000000000000, 0.000000000000000000, -1.000000000000000000 ) ) ;
#19984 = CARTESIAN_POINT ( 'NONE',  ( -15.15253849576580514, 26.98910714531248090, -7.345250183262973742 ) ) ;
#19986 = CARTESIAN_POINT ( 'NONE',  ( -9.644844900892618256, -18.14121070125914414, -28.70205165269834424 ) ) ;
#19987 = DIRECTION ( 'NONE',  ( 0.000000000000000000, 0.000000000000000000, 1.000000000000000000 ) ) ;
#19988 = CIRCLE ( 'NONE', #19960, 1.000000000000000888 ) ;
#19989 = ORIENTED_EDGE ( 'NONE', *, *, #30204, .F. ) ;
#19990 = CARTESIAN_POINT ( 'NONE',  ( -19.54202594190227416, -8.796642138048818893, -25.59909437478174610 ) ) ;
#19991 = CARTESIAN_POINT ( 'NONE',  ( -14.81594859391628027, -26.54803943294492896, -5.946254171449712800 ) ) ;
#19992 = DIRECTION ( 'NONE',  ( 1.000000000000000000, 0.000000000000000000, 0.000000000000000000 ) ) ;
#19993 = CARTESIAN_POINT ( 'NONE',  ( 16.48001596753842435, 21.51165321008922859, -9.781392695578974283 ) ) ;
#19994 = ORIENTED_EDGE ( 'NONE', *, *, #36102, .T. ) ;
#19995 = CARTESIAN_POINT ( 'NONE',  ( 26.24812223541028544, 2.914455890864420251, -12.67480056851672821 ) ) ;
#19996 = CARTESIAN_POINT ( 'NONE',  ( 9.788939752379329562, 23.27376113029817617, 13.00000000000000178 ) ) ;
#19997 = CARTESIAN_POINT ( 'NONE',  ( -20.38753357181594694, -16.19769905861803139, 23.00000000000000000 ) ) ;
#19998 = ORIENTED_EDGE ( 'NONE', *, *, #12462, .F. ) ;
#19999 = CARTESIAN_POINT ( 'NONE',  ( -20.70520357564727476, 0.6698834183737596426, -27.43687480068400575 ) ) ;
#20000 = CARTESIAN_POINT ( 'NONE',  ( 22.82302083792669478, 0.2992910856866396463, -21.57503696421676409 ) ) ;
#20001 = CARTESIAN_POINT ( 'NONE',  ( 31.83642866623112511, -11.02236948596282140, 19.27171037444156099 ) ) ;
#20002 = EDGE_CURVE ( 'NONE', #8296, #17265, #11676, .T. ) ;
#20003 = ORIENTED_EDGE ( 'NONE', *, *, #14773, .T. ) ;
#20004 = CARTESIAN_POINT ( 'NONE',  ( -21.42264437035803581, 2.133308088443877981, -24.00964802334802073 ) ) ;
#20005 = ADVANCED_FACE ( 'NONE', ( #20626 ), #30567, .F. ) ;
#20006 = CARTESIAN_POINT ( 'NONE',  ( -3.091399026088746727, 22.35909668862748134, -29.99999999999999289 ) ) ;
#20007 = CARTESIAN_POINT ( 'NONE',  ( -8.816778784387198087, 10.36474508437586195, 7.000000000000000000 ) ) ;
#20008 = AXIS2_PLACEMENT_3D ( 'NONE', #15144, #39916, #12096 ) ;
#20009 = CARTESIAN_POINT ( 'NONE',  ( -1.981967702234832984, 30.37627742347970283, 12.00000000000000000 ) ) ;
#20010 = AXIS2_PLACEMENT_3D ( 'NONE', #30654, #11959, #37541 ) ;
#20011 = AXIS2_PLACEMENT_3D ( 'NONE', #34933, #22522, #10957 ) ;
#20012 = CARTESIAN_POINT ( 'NONE',  ( -7.014595103779441843, 35.79644522156330311, 10.50000000000000000 ) ) ;
#20013 = CARTESIAN_POINT ( 'NONE',  ( -1.605702774688126722, 27.44183462127829642, 13.00000000000000178 ) ) ;
#20014 = CYLINDRICAL_SURFACE ( 'NONE', #2959, 1.000000000000000000 ) ;
#20015 = ORIENTED_EDGE ( 'NONE', *, *, #36732, .F. ) ;
#20016 = CYLINDRICAL_SURFACE ( 'NONE', #37683, 0.4999999999999997780 ) ;
#20017 = PLANE ( 'NONE',  #29161 ) ;
#20018 = CARTESIAN_POINT ( 'NONE',  ( 15.66978274593486198, -13.58963625838278055, -27.75455164708249356 ) ) ;
#20019 = CARTESIAN_POINT ( 'NONE',  ( 14.86556419889027048, 20.43481210330100240, 10.49999999999999822 ) ) ;
#20020 = CARTESIAN_POINT ( 'NONE',  ( 10.47804177580207607, 33.28010392086025604, 11.00000000000000000 ) ) ;
#20021 = EDGE_CURVE ( 'NONE', #648, #7392, #36969, .T. ) ;
#20022 = CARTESIAN_POINT ( 'NONE',  ( 11.30519648601890914, 19.26922631836183442, -22.66966561975009142 ) ) ;
#20023 = LINE ( 'NONE', #13511, #36014 ) ;
#20024 = ORIENTED_EDGE ( 'NONE', *, *, #10761, .T. ) ;
#20025 = CARTESIAN_POINT ( 'NONE',  ( -17.37423461678738690, 20.74184956833279969, -6.432056361720852600 ) ) ;
#20026 = CARTESIAN_POINT ( 'NONE',  ( 14.98890121934609532, -28.67928442654220333, 11.00000000000000000 ) ) ;
#20027 = EDGE_CURVE ( 'NONE', #7799, #32321, #14393, .T. ) ;
#20028 = CARTESIAN_POINT ( 'NONE',  ( 15.06737607521339939, -26.25728709294644503, -8.298505300031854048 ) ) ;
#20029 = DIRECTION ( 'NONE',  ( 0.6916548014802259559, -0.1470157664652035345, -0.7071067811865460184 ) ) ;
#20030 = CARTESIAN_POINT ( 'NONE',  ( 11.48833225930353130, 18.43385336031954225, -23.85456489029450111 ) ) ;
#20031 = ORIENTED_EDGE ( 'NONE', *, *, #10527, .T. ) ;
#20032 = CARTESIAN_POINT ( 'NONE',  ( 10.97760868008098889, 17.31306259807076131, -29.34820719497326280 ) ) ;
#20033 = ORIENTED_EDGE ( 'NONE', *, *, #7160, .T. ) ;
#20035 = CARTESIAN_POINT ( 'NONE',  ( 14.09933648065468503, 26.02968990214155198, 10.49999999999999822 ) ) ;
#20034 = CARTESIAN_POINT ( 'NONE',  ( -12.88510495915603293, 21.72514915063214502, -17.42774926625122589 ) ) ;
#20036 = CARTESIAN_POINT ( 'NONE',  ( -9.778777969284597305, -18.56702052074433951, -26.22551016879890184 ) ) ;
#20037 = CARTESIAN_POINT ( 'NONE',  ( -15.00437666251166746, -28.61930095463374712, 12.14047268033097460 ) ) ;
#20038 = AXIS2_PLACEMENT_3D ( 'NONE', #26134, #23495, #26948 ) ;
#20039 = AXIS2_PLACEMENT_3D ( 'NONE', #38555, #7261, #10729 ) ;
#20040 = CARTESIAN_POINT ( 'NONE',  ( -28.66680771549815887, -17.31871082804386219, -12.88878534390529040 ) ) ;
#20041 = CARTESIAN_POINT ( 'NONE',  ( -4.708882860453130981, -19.97645208405714712, -28.83077065012970408 ) ) ;
#20042 = CARTESIAN_POINT ( 'NONE',  ( 15.84467149865224833, 25.30824157118464868, -5.474055608616841262 ) ) ;
#20043 = ORIENTED_EDGE ( 'NONE', *, *, #23125, .F. ) ;
#20044 = CARTESIAN_POINT ( 'NONE',  ( 23.21632290521470665, 9.180027527831590817, -7.909577862357840772 ) ) ;
#20045 = CARTESIAN_POINT ( 'NONE',  ( 35.48538791413476190, -11.24999995268670006, -5.000000000000002665 ) ) ;
#20046 = FACE_OUTER_BOUND ( 'NONE', #18041, .T. ) ;
#20047 = DIRECTION ( 'NONE',  ( 0.000000000000000000, 0.000000000000000000, -1.000000000000000000 ) ) ;
#20048 = AXIS2_PLACEMENT_3D ( 'NONE', #34198, #270, #24847 ) ;
#20049 = ORIENTED_EDGE ( 'NONE', *, *, #2821, .T. ) ;
#20050 = CARTESIAN_POINT ( 'NONE',  ( -29.97494448726338234, -2.192815450784864062, -12.34847330071091598 ) ) ;
#20051 = CARTESIAN_POINT ( 'NONE',  ( -7.164929079095160525, 24.49151390636425418, 20.82122704794079837 ) ) ;
#20052 = VERTEX_POINT ( 'NONE', #8428 ) ;
#20053 = CARTESIAN_POINT ( 'NONE',  ( 18.23649648353767461, -16.09146789626181118, 20.99999999999999645 ) ) ;
#20054 = CARTESIAN_POINT ( 'NONE',  ( 18.76090689389210198, -16.22676322417229500, 20.99999999999999289 ) ) ;
#20055 = EDGE_CURVE ( 'NONE', #13272, #21146, #12946, .T. ) ;
#20056 = LINE ( 'NONE', #17423, #30703 ) ;
#20057 = CARTESIAN_POINT ( 'NONE',  ( 33.32532820267570628, -17.07072135929075429, -8.406244610255813043 ) ) ;
#20058 = EDGE_CURVE ( 'NONE', #20274, #36663, #29831, .T. ) ;
#20059 = CARTESIAN_POINT ( 'NONE',  ( 35.50541758542747317, -3.488475578028298774, 12.73282698324852724 ) ) ;
#20060 = ORIENTED_EDGE ( 'NONE', *, *, #24188, .T. ) ;
#20061 = FACE_OUTER_BOUND ( 'NONE', #21219, .T. ) ;
#20062 = DIRECTION ( 'NONE',  ( -1.000000000000000000, 0.000000000000000000, 0.000000000000000000 ) ) ;
#20063 = AXIS2_PLACEMENT_3D ( 'NONE', #28757, #13110, #16173 ) ;
#20064 = VECTOR ( 'NONE', #8270, 1000.000000000000114 ) ;
#20065 = CARTESIAN_POINT ( 'NONE',  ( -11.14717575287011542, 32.53695909538323860, 12.00000000000000000 ) ) ;
#20066 = ORIENTED_EDGE ( 'NONE', *, *, #24764, .F. ) ;
#20067 = CARTESIAN_POINT ( 'NONE',  ( -1.577295330230392700, 31.28878489215165715, -14.73372383095288285 ) ) ;
#20068 = CARTESIAN_POINT ( 'NONE',  ( -14.98531754163844276, 21.83276651127755486, 7.381627713044571770 ) ) ;
#20069 = CARTESIAN_POINT ( 'NONE',  ( 13.88403039571024244, 27.53692605078171241, 10.94611345180490503 ) ) ;
#20070 = PLANE ( 'NONE',  #7196 ) ;
#20071 = DIRECTION ( 'NONE',  ( -0.7071067811865479058, 0.000000000000000000, -0.7071067811865472397 ) ) ;
#20072 = EDGE_CURVE ( 'NONE', #15678, #21190, #27110, .T. ) ;
#20073 = CARTESIAN_POINT ( 'NONE',  ( 2.629601561899396422, 7.723830143584012653, 10.50000000000000000 ) ) ;
#20074 = CARTESIAN_POINT ( 'NONE',  ( 13.99360449555652686, 28.17614020743589265, -9.588039117105212839 ) ) ;
#20075 = CARTESIAN_POINT ( 'NONE',  ( -12.74038105676665289, 14.56698729810790027, 10.63089969389957368 ) ) ;
#20076 = ORIENTED_EDGE ( 'NONE', *, *, #18697, .F. ) ;
#20078 = LINE ( 'NONE', #25755, #8348 ) ;
#20077 = CARTESIAN_POINT ( 'NONE',  ( -20.11194080487678804, 14.58715024383956482, -7.424181446863920897 ) ) ;
#20079 = CARTESIAN_POINT ( 'NONE',  ( -0.8726219062944396976, 37.33905845026552583, 10.49999999999999822 ) ) ;
#20080 = EDGE_CURVE ( 'NONE', #34024, #13841, #24456, .T. ) ;
#20081 = CARTESIAN_POINT ( 'NONE',  ( 9.599968447380561543, -18.25860783104283769, -28.07576543594807461 ) ) ;
#20082 = DIRECTION ( 'NONE',  ( 0.6459741880212489518, 0.2876062384759403012, -0.7071067811865537900 ) ) ;
#20083 = CARTESIAN_POINT ( 'NONE',  ( 11.08697006596329793, 17.63936566195119227, -26.82682961117613729 ) ) ;
#20084 = CARTESIAN_POINT ( 'NONE',  ( -30.41237130417910706, 3.314011747244090422, -13.58461195433496371 ) ) ;
#20085 = CARTESIAN_POINT ( 'NONE',  ( -24.37697481792950782, -10.07885229508464953, 23.00000000000000355 ) ) ;
#20086 = EDGE_CURVE ( 'NONE', #22029, #12954, #29801, .T. ) ;
#20087 = CARTESIAN_POINT ( 'NONE',  ( -22.94869330768877802, -20.35003466596009858, -14.81020240946884492 ) ) ;
#20088 = CARTESIAN_POINT ( 'NONE',  ( 7.129976846286900205, -22.60938466117447732, -16.81300626758635630 ) ) ;
#20089 = CARTESIAN_POINT ( 'NONE',  ( 15.54167675008477723, 26.33752833710220997, -5.000000000000000888 ) ) ;
#20090 = CARTESIAN_POINT ( 'NONE',  ( 18.44994286627233038, 12.34598615494684637, -19.05470978867802145 ) ) ;
#20091 = DIRECTION ( 'NONE',  ( 0.000000000000000000, 0.000000000000000000, 1.000000000000000000 ) ) ;
#20092 = ORIENTED_EDGE ( 'NONE', *, *, #18115, .T. ) ;
#20093 = CARTESIAN_POINT ( 'NONE',  ( -4.084317376857201864, 20.18095795116958158, -28.48257084316769294 ) ) ;
#20094 = ORIENTED_EDGE ( 'NONE', *, *, #37842, .F. ) ;
#20095 = AXIS2_PLACEMENT_3D ( 'NONE', #19605, #1735, #38701 ) ;
#20096 = CARTESIAN_POINT ( 'NONE',  ( -2.476907992048017260, 18.63850621467409496, 13.00000000000000178 ) ) ;
#20097 = ORIENTED_EDGE ( 'NONE', *, *, #21664, .T. ) ;
#20098 = DIRECTION ( 'NONE',  ( -0.000000000000000000, 0.000000000000000000, 1.000000000000000000 ) ) ;
#20099 = CARTESIAN_POINT ( 'NONE',  ( 9.296885549838558305, 10.71356306745936138, 10.49999999999999822 ) ) ;
#20100 = AXIS2_PLACEMENT_3D ( 'NONE', #11167, #35754, #20722 ) ;
#20101 = ORIENTED_EDGE ( 'NONE', *, *, #32069, .F. ) ;
#20102 = CARTESIAN_POINT ( 'NONE',  ( -30.63398949461165088, 0.1319342208294977115, -6.417236068070889310 ) ) ;
#20103 = EDGE_CURVE ( 'NONE', #31697, #10973, #14316, .T. ) ;
#20104 = VERTEX_POINT ( 'NONE', #2133 ) ;
#20105 = CARTESIAN_POINT ( 'NONE',  ( 23.45217438398567111, -5.581096782014018487, -20.95586870486150843 ) ) ;
#20106 = ADVANCED_FACE ( 'NONE', ( #5569 ), #14517, .T. ) ;
#20107 = ORIENTED_EDGE ( 'NONE', *, *, #32878, .T. ) ;
#20108 = DIRECTION ( 'NONE',  ( 1.000000000000000000, 0.000000000000000000, 0.000000000000000000 ) ) ;
#20109 = CARTESIAN_POINT ( 'NONE',  ( -17.34253826607185900, 27.32041144404031030, 11.00000000000000000 ) ) ;
#20110 = ORIENTED_EDGE ( 'NONE', *, *, #31497, .T. ) ;
#20111 = DIRECTION ( 'NONE',  ( 1.000000000000000000, 0.000000000000000000, 0.000000000000000000 ) ) ;
#20112 = FACE_OUTER_BOUND ( 'NONE', #34146, .T. ) ;
#20113 = CARTESIAN_POINT ( 'NONE',  ( -5.791386747369965171, 35.03736185296623518, 18.42518152272108978 ) ) ;
#20114 = DIRECTION ( 'NONE',  ( -0.6691306063588671194, -0.7431448254773863615, 0.000000000000000000 ) ) ;
#20115 = EDGE_LOOP ( 'NONE', ( #16786, #8632, #35831, #22218 ) ) ;
#20116 = SURFACE_STYLE_FILL_AREA ( #29048 ) ;
#20117 = PLANE ( 'NONE',  #5500 ) ;
#20118 = CARTESIAN_POINT ( 'NONE',  ( -6.064571727552472424, 31.45661825943146894, 13.00000000000000178 ) ) ;
#20119 = LINE ( 'NONE', #32520, #22115 ) ;
#20120 = CARTESIAN_POINT ( 'NONE',  ( 15.98323640732827400, 14.59684562732355673, -22.14531699329461034 ) ) ;
#20122 = AXIS2_PLACEMENT_3D ( 'NONE', #27507, #39096, #33623 ) ;
#20121 = CARTESIAN_POINT ( 'NONE',  ( 6.309536247299391221, 19.51471286317475773, -29.25949660933323671 ) ) ;
#20123 = EDGE_LOOP ( 'NONE', ( #39563, #13679, #8465 ) ) ;
#20124 = CARTESIAN_POINT ( 'NONE',  ( 12.28720923547795429, -14.55658080553756584, 20.99999999999999645 ) ) ;
#20125 = CARTESIAN_POINT ( 'NONE',  ( -3.813962023474482876, 32.29559562678526419, 10.50000000000000000 ) ) ;
#20126 = EDGE_CURVE ( 'NONE', #30574, #23393, #10341, .T. ) ;
#20127 = CARTESIAN_POINT ( 'NONE',  ( 11.72988935907280350, -20.95426047538857972, -19.47340356160194474 ) ) ;
#20128 = DIRECTION ( 'NONE',  ( 0.2185080122244175416, 0.6724985119639551590, -0.7071067811865474617 ) ) ;
#20129 = CIRCLE ( 'NONE', #9105, 0.5000000000000004441 ) ;
#20130 = DIRECTION ( 'NONE',  ( -1.224646799147351235E-16, 1.000000000000000000, 0.000000000000000000 ) ) ;
#20131 = VERTEX_POINT ( 'NONE', #2534 ) ;
#20132 = CARTESIAN_POINT ( 'NONE',  ( -10.99444046889570537, 17.35561201924551256, -28.70647127135751475 ) ) ;
#20133 = CARTESIAN_POINT ( 'NONE',  ( -32.79363849989120894, -0.7437118703953984333, 15.13084544680199883 ) ) ;
#20134 = CARTESIAN_POINT ( 'NONE',  ( 12.30749475060790843, -22.55415536556771272, -16.47007971746634780 ) ) ;
#20135 = DIRECTION ( 'NONE',  ( 0.9510565162951544194, 0.3090169943749449533, -0.000000000000000000 ) ) ;
#20136 = ORIENTED_EDGE ( 'NONE', *, *, #5319, .T. ) ;
#20137 = ORIENTED_EDGE ( 'NONE', *, *, #3640, .F. ) ;
#20138 = CARTESIAN_POINT ( 'NONE',  ( -9.699844911044960938, 24.40834062817878447, -17.99019714132644765 ) ) ;
#20139 = CARTESIAN_POINT ( 'NONE',  ( 8.410254037844358876, 17.06698729810774395, 10.50000000000000000 ) ) ;
#20140 = FACE_BOUND ( 'NONE', #21788, .T. ) ;
#20141 = VECTOR ( 'NONE', #11567, 1000.000000000000000 ) ;
#20142 = CARTESIAN_POINT ( 'NONE',  ( -25.28614151405769306, -6.243831222781579982, -18.83763890451589518 ) ) ;
#20143 = DIRECTION ( 'NONE',  ( 1.000000000000000000, 0.000000000000000000, -0.000000000000000000 ) ) ;
#20144 = VERTEX_POINT ( 'NONE', #5965 ) ;
#20145 = CARTESIAN_POINT ( 'NONE',  ( 29.46685023586550400, 0.1954524857158681794, -10.18384896449856036 ) ) ;
#20146 = CARTESIAN_POINT ( 'NONE',  ( -13.63581098909220479, 27.45627467658446008, 7.000000000000000000 ) ) ;
#20147 = DIRECTION ( 'NONE',  ( 0.000000000000000000, 0.000000000000000000, -1.000000000000000000 ) ) ;
#20148 = CARTESIAN_POINT ( 'NONE',  ( -2.525645716490712012, 8.212903943950955465, 7.000000000000000000 ) ) ;
#20149 = ORIENTED_EDGE ( 'NONE', *, *, #4610, .F. ) ;
#20150 = CARTESIAN_POINT ( 'NONE',  ( -28.89319593916525264, 0.09792079263888439633, -11.59890374343908803 ) ) ;
#20151 = PLANE ( 'NONE',  #6014 ) ;
#20152 = ORIENTED_EDGE ( 'NONE', *, *, #31119, .F. ) ;
#20153 = CARTESIAN_POINT ( 'NONE',  ( 29.11583290636277255, -1.894276822915576863, -13.31891975639820025 ) ) ;
#20154 = CARTESIAN_POINT ( 'NONE',  ( 31.71434132860828470, -22.43226626708964133, 15.72805884748975203 ) ) ;
#20155 = VERTEX_POINT ( 'NONE', #33224 ) ;
#20156 = CARTESIAN_POINT ( 'NONE',  ( 12.63299342935012959, 33.22349594678088636, 15.72805884748943939 ) ) ;
#20157 = ADVANCED_FACE ( 'NONE', ( #18370, #26708 ), #5372, .F. ) ;
#20158 = CIRCLE ( 'NONE', #29255, 0.5000000000000004441 ) ;
#20159 = CARTESIAN_POINT ( 'NONE',  ( 16.41753675003788615, -23.14183271658374608, 19.27171037444156454 ) ) ;
#20160 = FACE_OUTER_BOUND ( 'NONE', #603, .T. ) ;
#20161 = CARTESIAN_POINT ( 'NONE',  ( -3.137032374298060589, 29.29040802067846982, 20.82122704794080192 ) ) ;
#20162 = DIRECTION ( 'NONE',  ( -0.07391278520356001080, 0.7032331762534130837, -0.7071067811865392461 ) ) ;
#20163 = ORIENTED_EDGE ( 'NONE', *, *, #18809, .F. ) ;
#20164 = CARTESIAN_POINT ( 'NONE',  ( 0.5000000000000001110, 37.00000000000000711, 7.000000000000000000 ) ) ;
#20165 = ADVANCED_FACE ( 'NONE', ( #8827 ), #21213, .F. ) ;
#20166 = CARTESIAN_POINT ( 'NONE',  ( 3.215895501801615985, 24.37283748036874442, -20.74290920587755593 ) ) ;
#20167 = VECTOR ( 'NONE', #33811, 1000.000000000000000 ) ;
#20168 = CARTESIAN_POINT ( 'NONE',  ( 0.4999999999999995559, 37.00000000000000711, 11.00000000000000000 ) ) ;
#20169 = CARTESIAN_POINT ( 'NONE',  ( 15.87271491999413264, 26.91186955881611809, 15.72805884748939853 ) ) ;
#20170 = CARTESIAN_POINT ( 'NONE',  ( 16.66225199357186426, -19.51117972168512082, -18.94818515844563933 ) ) ;
#20171 = DIRECTION ( 'NONE',  ( 0.000000000000000000, 0.000000000000000000, -1.000000000000000000 ) ) ;
#20172 = PLANE ( 'NONE',  #28683 ) ;
#20173 = DIRECTION ( 'NONE',  ( 1.000000000000000000, 0.000000000000000000, 0.000000000000000000 ) ) ;
#20174 = ORIENTED_EDGE ( 'NONE', *, *, #28630, .T. ) ;
#20175 = CARTESIAN_POINT ( 'NONE',  ( 14.24751785689744743, 24.58680083500108182, -12.54074944469350683 ) ) ;
#20176 = ORIENTED_EDGE ( 'NONE', *, *, #26288, .F. ) ;
#20177 = CARTESIAN_POINT ( 'NONE',  ( -14.73975063325908152, 24.40991067048773644, -11.61570129997859269 ) ) ;
#20178 = CARTESIAN_POINT ( 'NONE',  ( -28.20105441993478834, -17.62361288429907802, 19.99202127657073191 ) ) ;
#20179 = EDGE_CURVE ( 'NONE', #31776, #21244, #35024, .T. ) ;
#20180 = DIRECTION ( 'NONE',  ( 1.000000000000000000, 0.000000000000000000, 0.000000000000000000 ) ) ;
#20181 = CARTESIAN_POINT ( 'NONE',  ( 14.96335647831743287, 25.71149453912319771, -9.710330481890405707 ) ) ;
#20182 = ORIENTED_EDGE ( 'NONE', *, *, #33614, .T. ) ;
#20183 = CARTESIAN_POINT ( 'NONE',  ( 19.07715750984440817, -9.791667150159778288, -25.58058246820311865 ) ) ;
#20184 = VECTOR ( 'NONE', #37553, 1000.000000000000000 ) ;
#20185 = ORIENTED_EDGE ( 'NONE', *, *, #29148, .T. ) ;
#20187 = CARTESIAN_POINT ( 'NONE',  ( -4.817371740575545402, 23.83900317890010001, 23.00000000000000000 ) ) ;
#20186 = CARTESIAN_POINT ( 'NONE',  ( -11.67086652466456087, 19.61581206493572438, -21.57501891504949398 ) ) ;
#20188 = CARTESIAN_POINT ( 'NONE',  ( -13.21758073316063431, -21.34862723106953197, -18.29696183777072704 ) ) ;
#20189 = FACE_OUTER_BOUND ( 'NONE', #15450, .T. ) ;
#20190 = VERTEX_POINT ( 'NONE', #7310 ) ;
#20191 = CARTESIAN_POINT ( 'NONE',  ( -19.06849745787630468, -8.585213063630757091, -26.98300186761300878 ) ) ;
#20192 = CARTESIAN_POINT ( 'NONE',  ( -11.91314923935176928, -22.03502826895537936, -17.47013640216600905 ) ) ;
#20193 = CARTESIAN_POINT ( 'NONE',  ( 19.30730118283910457, -16.27608008926517513, 23.00000000000000000 ) ) ;
#20194 = CARTESIAN_POINT ( 'NONE',  ( 17.13680108443139716, 20.87122319733086329, -7.868605303123856309 ) ) ;
#20195 = VERTEX_POINT ( 'NONE', #12270 ) ;
#20196 = CARTESIAN_POINT ( 'NONE',  ( 26.51973020456226493, 3.772046466887580607, -10.27100251072616288 ) ) ;
#20197 = CARTESIAN_POINT ( 'NONE',  ( 1.605696033269625955, 17.55816537872232530, 6.000000000000000000 ) ) ;
#20198 = DIRECTION ( 'NONE',  ( -0.4067366430757888285, 0.9135454576426059736, -0.000000000000000000 ) ) ;
#20199 = EDGE_LOOP ( 'NONE', ( #28445, #27518, #4497, #18692 ) ) ;
#20200 = CARTESIAN_POINT ( 'NONE',  ( -29.52555509693227265, -0.1188359627376792682, -10.63800653123224293 ) ) ;
#20201 = CARTESIAN_POINT ( 'NONE',  ( 24.79371228178270314, -0.05885538004481753738, -18.38622137752647134 ) ) ;
#20202 = VECTOR ( 'NONE', #40034, 1000.000000000000000 ) ;
#20203 = CARTESIAN_POINT ( 'NONE',  ( 28.60197298177003589, -19.58586899272799187, 19.27171037444191271 ) ) ;
#20204 = CIRCLE ( 'NONE', #35096, 6.000000000000003553 ) ;
#20205 = EDGE_CURVE ( 'NONE', #26597, #20501, #24657, .T. ) ;
#20206 = ORIENTED_EDGE ( 'NONE', *, *, #1223, .F. ) ;
#20207 = CARTESIAN_POINT ( 'NONE',  ( -20.44235121065545613, 1.535337040937289066, -29.36017822837253988 ) ) ;
#20208 = CARTESIAN_POINT ( 'NONE',  ( -11.10756861982300947, 19.59949212537556562, -20.90349153980999830 ) ) ;
#20209 = CARTESIAN_POINT ( 'NONE',  ( -5.440908595777638190, 35.94977745735568675, 11.00000000000000000 ) ) ;
#20210 = DIRECTION ( 'NONE',  ( 0.8090169943749426773, -0.5877852522924796874, -0.000000000000000000 ) ) ;
#20211 = ADVANCED_FACE ( 'NONE', ( #15314 ), #37251, .F. ) ;
#20212 = EDGE_CURVE ( 'NONE', #39810, #23537, #1235, .T. ) ;
#20213 = CARTESIAN_POINT ( 'NONE',  ( 0.6237317017440463518, 25.43444280220171194, 6.000000000000000000 ) ) ;
#20214 = CARTESIAN_POINT ( 'NONE',  ( -8.315274455032216849, 10.01576150750520888, 7.000000000000000000 ) ) ;
#20215 = CARTESIAN_POINT ( 'NONE',  ( 5.440908595777817602, 35.94977745735560859, 7.000000000000000000 ) ) ;
#20216 = ORIENTED_EDGE ( 'NONE', *, *, #39284, .T. ) ;
#20217 = CARTESIAN_POINT ( 'NONE',  ( -21.97373458415457037, 5.076385617489679980, -19.92418931931740644 ) ) ;
#20218 = DIRECTION ( 'NONE',  ( 0.4067366430757984874, 0.9135454576426016438, -2.081668171172158416E-14 ) ) ;
#20219 = LINE ( 'NONE', #29351, #27856 ) ;
#20220 = CARTESIAN_POINT ( 'NONE',  ( 28.35230428231212230, -24.61827297795788638, -5.439370354368517013 ) ) ;
#20221 = FACE_OUTER_BOUND ( 'NONE', #20123, .T. ) ;
#20222 = CARTESIAN_POINT ( 'NONE',  ( -14.41430201638242714, 20.48224166989796302, 11.00000000000000355 ) ) ;
#20223 = CARTESIAN_POINT ( 'NONE',  ( 15.24739647947424714, 27.26377957105179917, -5.940767840820030621 ) ) ;
#20224 =( NAMED_UNIT ( * ) SI_UNIT ( $, .STERADIAN. ) SOLID_ANGLE_UNIT ( ) );
#20225 = ORIENTED_EDGE ( 'NONE', *, *, #37697, .F. ) ;
#20226 = AXIS2_PLACEMENT_3D ( 'NONE', #24155, #39197, #20914 ) ;
#20227 = CARTESIAN_POINT ( 'NONE',  ( -16.88103042039869450, 19.95524105454239816, -10.77970369993180277 ) ) ;
#20228 = CARTESIAN_POINT ( 'NONE',  ( -24.37759566069507855, -10.08322588119029817, 20.99999999999999645 ) ) ;
#20229 = AXIS2_PLACEMENT_3D ( 'NONE', #40186, #6260, #3018 ) ;
#20230 = EDGE_CURVE ( 'NONE', #16334, #33648, #13615, .T. ) ;
#20231 = CARTESIAN_POINT ( 'NONE',  ( 9.910011124334165089, -18.83656552785947724, -25.02100245519685018 ) ) ;
#20232 = EDGE_CURVE ( 'NONE', #30940, #24654, #31139, .T. ) ;
#20233 = LINE ( 'NONE', #7825, #12658 ) ;
#20234 = CARTESIAN_POINT ( 'NONE',  ( 11.08571900862292026, 17.49394017797068557, -27.44878439575566631 ) ) ;
#20235 = ORIENTED_EDGE ( 'NONE', *, *, #892, .F. ) ;
#20236 = CARTESIAN_POINT ( 'NONE',  ( 11.29809999771842932, 18.04734829986520950, -25.01294377573191952 ) ) ;
#20237 = ORIENTED_EDGE ( 'NONE', *, *, #5391, .T. ) ;
#20239 = CARTESIAN_POINT ( 'NONE',  ( -20.23296131041716706, 28.12381335138030636, 3.000000000000000000 ) ) ;
#20238 = CARTESIAN_POINT ( 'NONE',  ( -11.83932568694060450, 19.43865753690332809, -21.60690038723429751 ) ) ;
#20240 = CARTESIAN_POINT ( 'NONE',  ( -10.20105000702817932, -19.17274393931131371, -23.85688496074367393 ) ) ;
#20241 = CARTESIAN_POINT ( 'NONE',  ( -37.07075634848843038, -14.79048025366256169, 12.14047268033097282 ) ) ;
#20242 = CARTESIAN_POINT ( 'NONE',  ( -17.41815810822877353, -11.99257218473442776, -26.26776909220020784 ) ) ;
#20243 = CARTESIAN_POINT ( 'NONE',  ( -7.781299079984965061, -22.59512116915117375, -16.77857488574911571 ) ) ;
#20244 = CARTESIAN_POINT ( 'NONE',  ( 15.76470487440841062, 24.68801468592181791, -7.838331335750884143 ) ) ;
#20245 = ORIENTED_EDGE ( 'NONE', *, *, #22187, .T. ) ;
#20246 = CARTESIAN_POINT ( 'NONE',  ( 21.20949775426257844, 8.625473678353458240, -16.95001661513558844 ) ) ;
#20247 = CARTESIAN_POINT ( 'NONE',  ( 20.23296131041715640, 28.12381335138032412, 0.000000000000000000 ) ) ;
#20248 = AXIS2_PLACEMENT_3D ( 'NONE', #12389, #2457, #14844 ) ;
#20249 = CARTESIAN_POINT ( 'NONE',  ( -12.12384649078149934, -25.96922316649875739, -5.000000000000000888 ) ) ;
#20250 = PLANE ( 'NONE',  #5679 ) ;
#20251 = ORIENTED_EDGE ( 'NONE', *, *, #14856, .T. ) ;
#20252 = CARTESIAN_POINT ( 'NONE',  ( -21.46822025407879408, -1.246220581431492391, -24.79526857062417733 ) ) ;
#20253 = CARTESIAN_POINT ( 'NONE',  ( -25.98021325959403072, -4.875178728618521973, 20.50957957746029336 ) ) ;
#20254 = CARTESIAN_POINT ( 'NONE',  ( 26.04175756481604509, -10.41789154269857320, 20.94377226548378346 ) ) ;
#20255 = CARTESIAN_POINT ( 'NONE',  ( 6.282361020112160688, 14.70372268239673197, 10.50000000000000000 ) ) ;
#20256 = EDGE_CURVE ( 'NONE', #6396, #33348, #28855, .T. ) ;
#20257 = DIRECTION ( 'NONE',  ( -0.9781476007338069101, -0.2079116908177532363, 0.000000000000000000 ) ) ;
#20258 = CARTESIAN_POINT ( 'NONE',  ( 34.01930034203780906, -17.43549634978032969, -6.697537572123588134 ) ) ;
#20259 = DIRECTION ( 'NONE',  ( -1.000000000000000000, 0.000000000000000000, 0.000000000000000000 ) ) ;
#20260 = ORIENTED_EDGE ( 'NONE', *, *, #5443, .T. ) ;
#20261 = CARTESIAN_POINT ( 'NONE',  ( -3.000488737322915878, 30.46850471150003159, 7.000000000000000000 ) ) ;
#20262 = DIRECTION ( 'NONE',  ( 0.000000000000000000, 0.7071067811865500152, -0.7071067811865451302 ) ) ;
#20263 = CARTESIAN_POINT ( 'NONE',  ( 6.557822374958315770, 35.99981354310111215, 10.50000000000000000 ) ) ;
#20264 = EDGE_LOOP ( 'NONE', ( #25128, #37146, #27440, #4046 ) ) ;
#20265 = CARTESIAN_POINT ( 'NONE',  ( 0.9672072501420434509, 23.74532692743124329, -21.84035651827026214 ) ) ;
#20266 = CARTESIAN_POINT ( 'NONE',  ( -14.96930490892015797, 21.54088032874991399, 7.500000000000004441 ) ) ;
#20267 = FACE_OUTER_BOUND ( 'NONE', #1574, .T. ) ;
#20268 = AXIS2_PLACEMENT_3D ( 'NONE', #39926, #2168, #8252 ) ;
#20269 = CARTESIAN_POINT ( 'NONE',  ( 13.64210930126480115, 24.20081211342298744, 13.00000000000000178 ) ) ;
#20270 = CARTESIAN_POINT ( 'NONE',  ( -9.917741276437942233, 30.52956727630665057, 6.000000000000000000 ) ) ;
#20271 = CARTESIAN_POINT ( 'NONE',  ( -3.587667106213709101, 35.31811204475769728, 13.00000000000000178 ) ) ;
#20272 = CARTESIAN_POINT ( 'NONE',  ( 14.23294558246579022, 29.80882899807581055, -5.461287637657078697 ) ) ;
#20273 = DIRECTION ( 'NONE',  ( -0.3090169943749560000, -0.9510565162951507556, 0.000000000000000000 ) ) ;
#20274 = VERTEX_POINT ( 'NONE', #4271 ) ;
#20275 = VECTOR ( 'NONE', #9446, 1000.000000000000000 ) ;
#20277 = CARTESIAN_POINT ( 'NONE',  ( -10.78894649379783388, 21.72623886970244911, 12.00000000000000000 ) ) ;
#20276 = CARTESIAN_POINT ( 'NONE',  ( -20.19236039815038808, 14.65651441764425833, -5.965904664850079087 ) ) ;
#20278 = CARTESIAN_POINT ( 'NONE',  ( -0.4999999999999964473, 37.50000000000000711, 10.49999999999999822 ) ) ;
#20279 = CARTESIAN_POINT ( 'NONE',  ( 15.01100859456593817, -25.99757226175481861, -9.236802265591313343 ) ) ;
#20280 = DIRECTION ( 'NONE',  ( 0.7071067811865499042, 0.000000000000000000, 0.7071067811865451302 ) ) ;
#20281 = CARTESIAN_POINT ( 'NONE',  ( 14.26815522538843872, 24.53214742665168302, -12.54540486666444643 ) ) ;
#20282 = CARTESIAN_POINT ( 'NONE',  ( -19.79815887584811307, 19.84782313723621883, -13.42901749168595771 ) ) ;
#20283 = CARTESIAN_POINT ( 'NONE',  ( 12.41947502333593967, 43.35441443594645250, 7.000000000000000000 ) ) ;
#20284 = EDGE_CURVE ( 'NONE', #20274, #1646, #18570, .T. ) ;
#20285 = CARTESIAN_POINT ( 'NONE',  ( -26.47200088153462261, -24.85570260301889789, -8.022744550273097630 ) ) ;
#20286 = CIRCLE ( 'NONE', #17690, 1.000000000000000888 ) ;
#20287 = CARTESIAN_POINT ( 'NONE',  ( 4.020749035821322259, -24.85085155051347883, -5.964422724544506060 ) ) ;
#20288 = CARTESIAN_POINT ( 'NONE',  ( 15.04807939094960290, 25.45191101363087682, -9.714351570550116222 ) ) ;
#20289 = CARTESIAN_POINT ( 'NONE',  ( 17.67233557286219892, 11.74463701656010706, -23.32306369647684363 ) ) ;
#20290 = CARTESIAN_POINT ( 'NONE',  ( -5.440908595777636414, 35.94977745735568675, 9.000000000000001776 ) ) ;
#20291 = ORIENTED_EDGE ( 'NONE', *, *, #31121, .F. ) ;
#20292 = CARTESIAN_POINT ( 'NONE',  ( -4.679325431169941929, 23.08454507055297711, -21.96044281907038354 ) ) ;
#20293 = EDGE_LOOP ( 'NONE', ( #1004, #30696, #4948, #37811, #28828, #3141 ) ) ;
#20294 = CIRCLE ( 'NONE', #12506, 1.000000000000000888 ) ;
#20295 = CARTESIAN_POINT ( 'NONE',  ( -11.77091082532341204, 29.60251629318183575, 13.00000000000000178 ) ) ;
#20296 = ORIENTED_EDGE ( 'NONE', *, *, #33374, .F. ) ;
#20297 = DIRECTION ( 'NONE',  ( -0.2079116908177664202, -0.9781476007338041345, 0.000000000000000000 ) ) ;
#20298 = CIRCLE ( 'NONE', #33274, 1.000000000000000000 ) ;
#20299 = LINE ( 'NONE', #36140, #29748 ) ;
#20300 = ORIENTED_EDGE ( 'NONE', *, *, #10007, .F. ) ;
#20301 = CARTESIAN_POINT ( 'NONE',  ( -20.47417334391911936, 1.028570030172704985, -30.00000000000000000 ) ) ;
#20302 = EDGE_CURVE ( 'NONE', #19765, #32281, #31156, .T. ) ;
#20303 = ORIENTED_EDGE ( 'NONE', *, *, #32474, .T. ) ;
#20304 = CARTESIAN_POINT ( 'NONE',  ( 19.84734553509363053, -6.000422723447369044, -27.77669457348836701 ) ) ;
#20305 = AXIS2_PLACEMENT_3D ( 'NONE', #8140, #14435, #29280 ) ;
#20306 = EDGE_CURVE ( 'NONE', #9166, #11008, #21804, .T. ) ;
#20307 = ORIENTED_EDGE ( 'NONE', *, *, #31638, .F. ) ;
#20308 = CARTESIAN_POINT ( 'NONE',  ( 13.97943872024082346, 27.84235072122924137, 10.49999999999999467 ) ) ;
#20309 = EDGE_LOOP ( 'NONE', ( #9877, #32732, #8161, #15482 ) ) ;
#20310 = DIRECTION ( 'NONE',  ( 0.000000000000000000, 0.000000000000000000, 1.000000000000000000 ) ) ;
#20311 = DIRECTION ( 'NONE',  ( -0.000000000000000000, -0.000000000000000000, -1.000000000000000000 ) ) ;
#20312 = AXIS2_PLACEMENT_3D ( 'NONE', #30422, #35711, #7865 ) ;
#20313 = CARTESIAN_POINT ( 'NONE',  ( 3.110808594360203738, 36.60201144129485584, 17.92354375535251876 ) ) ;
#20314 = EDGE_CURVE ( 'NONE', #8575, #36455, #4541, .T. ) ;
#20315 = DIRECTION ( 'NONE',  ( 0.4067366430758010409, 0.9135454576426005335, -0.000000000000000000 ) ) ;
#20316 = ORIENTED_EDGE ( 'NONE', *, *, #15575, .F. ) ;
#20317 = CARTESIAN_POINT ( 'NONE',  ( 6.064564986133971658, 13.54338174056915456, 12.00000000000000000 ) ) ;
#20318 = FACE_OUTER_BOUND ( 'NONE', #3949, .T. ) ;
#20319 = DIRECTION ( 'NONE',  ( 0.000000000000000000, 0.000000000000000000, 1.000000000000000000 ) ) ;
#20320 = CARTESIAN_POINT ( 'NONE',  ( 17.86751023708650976, 15.56654134878274753, -14.86208373478310563 ) ) ;
#20321 = AXIS2_PLACEMENT_3D ( 'NONE', #23899, #35493, #20665 ) ;
#20322 = CARTESIAN_POINT ( 'NONE',  ( 11.67450463981393405, 33.32297107450499141, -6.328599700080098422 ) ) ;
#20323 = ORIENTED_EDGE ( 'NONE', *, *, #15204, .T. ) ;
#20324 = CARTESIAN_POINT ( 'NONE',  ( 0.000000000000000000, 22.50000000000000355, 10.00000000000000000 ) ) ;
#20325 = PLANE ( 'NONE',  #20769 ) ;
#20326 = VECTOR ( 'NONE', #3926, 1000.000000000000000 ) ;
#20327 = CARTESIAN_POINT ( 'NONE',  ( 15.72657732487407323, -26.77584194611982937, -5.943392230339449078 ) ) ;
#20328 = CARTESIAN_POINT ( 'NONE',  ( 18.03924190088524782, -16.85603499720511422, 20.99999999999998934 ) ) ;
#20329 = EDGE_CURVE ( 'NONE', #2112, #28965, #33764, .T. ) ;
#20330 = EDGE_CURVE ( 'NONE', #35813, #32704, #18180, .T. ) ;
#20331 = DIRECTION ( 'NONE',  ( -0.9945218953682742891, -0.1045284632676437564, 0.000000000000000000 ) ) ;
#20332 = EDGE_CURVE ( 'NONE', #34846, #26679, #19920, .T. ) ;
#20333 = ORIENTED_EDGE ( 'NONE', *, *, #6989, .F. ) ;
#20334 = CARTESIAN_POINT ( 'NONE',  ( -15.33156057601598654, 26.64116238436768214, -6.887479782135956796 ) ) ;
#20335 = CIRCLE ( 'NONE', #15767, 1.000000000000007772 ) ;
#20336 = CARTESIAN_POINT ( 'NONE',  ( -34.65585262756959395, -3.900084976043918239, 15.13084544680213561 ) ) ;
#20337 = CARTESIAN_POINT ( 'NONE',  ( 13.92713108795117449, -25.88915498332963594, -8.779116367686647493 ) ) ;
#20338 = DIRECTION ( 'NONE',  ( 0.2079116908177533474, -0.9781476007338067991, 0.000000000000000000 ) ) ;
#20339 = VERTEX_POINT ( 'NONE', #19509 ) ;
#20340 = EDGE_LOOP ( 'NONE', ( #20296, #13482, #16617, #3703 ) ) ;
#20341 = CARTESIAN_POINT ( 'NONE',  ( -7.677290147211063065, 19.01944725762398392, -29.28149183438886993 ) ) ;
#20342 = CARTESIAN_POINT ( 'NONE',  ( 14.97009266215792778, 21.42933399866928568, 11.00000000000000000 ) ) ;
#20343 = CIRCLE ( 'NONE', #16449, 0.9999999999999995559 ) ;
#20344 = FACE_BOUND ( 'NONE', #6912, .T. ) ;
#20345 = CARTESIAN_POINT ( 'NONE',  ( -32.50609658070614216, -5.122312372317453288, -10.36378763344411169 ) ) ;
#20346 = CARTESIAN_POINT ( 'NONE',  ( -14.97283171447380390, 21.48159823030330884, 11.00000000000000000 ) ) ;
#20347 = VERTEX_POINT ( 'NONE', #37450 ) ;
#20348 = CARTESIAN_POINT ( 'NONE',  ( 22.20197406284108510, 0.7415789608456136994, -22.74446640454221225 ) ) ;
#20349 = DIRECTION ( 'NONE',  ( 0.8090169943749504489, 0.5877852522924689183, 0.000000000000000000 ) ) ;
#20350 = DIRECTION ( 'NONE',  ( 0.000000000000000000, 0.000000000000000000, 1.000000000000000000 ) ) ;
#20351 = CARTESIAN_POINT ( 'NONE',  ( -2.141014423450144033, 7.887532638883575586, 10.49999999999999822 ) ) ;
#20352 = ORIENTED_EDGE ( 'NONE', *, *, #19600, .T. ) ;
#20353 = CARTESIAN_POINT ( 'NONE',  ( -24.55940606212222121, 0.4314668635417708287, -18.45227070181689299 ) ) ;
#20354 = DIRECTION ( 'NONE',  ( 0.1045284632676436315, -0.9945218953682742891, 0.000000000000000000 ) ) ;
#20355 = EDGE_CURVE ( 'NONE', #35442, #29211, #15558, .T. ) ;
#20356 = ORIENTED_EDGE ( 'NONE', *, *, #38437, .T. ) ;
#20357 = CARTESIAN_POINT ( 'NONE',  ( 27.51989245245352578, -3.247923778376513582, -16.07734993535055779 ) ) ;
#20358 = VECTOR ( 'NONE', #28347, 1000.000000000000114 ) ;
#20359 = CARTESIAN_POINT ( 'NONE',  ( 31.24272016125166829, 0.2902395683485590738, 15.72805884748940031 ) ) ;
#20360 = EDGE_CURVE ( 'NONE', #4426, #12819, #6169, .T. ) ;
#20361 = VERTEX_POINT ( 'NONE', #31902 ) ;
#20362 = AXIS2_PLACEMENT_3D ( 'NONE', #22532, #13598, #26191 ) ;
#20363 = CARTESIAN_POINT ( 'NONE',  ( 17.01882136418227986, 27.23043334310844443, 13.32518128616608877 ) ) ;
#20364 = B_SPLINE_CURVE_WITH_KNOTS ( 'NONE', 3,
 ( #22314, #25560, #37362, #34714 ),
 .UNSPECIFIED., .F., .F.,
 ( 4, 4 ),
 ( 0.000000000000000000, 0.3999999999265801964 ),
 .UNSPECIFIED. ) ;
#20365 = CARTESIAN_POINT ( 'NONE',  ( 10.51283450065148273, -24.98199432654207897, 16.87380292611226551 ) ) ;
#20366 = DIRECTION ( 'NONE',  ( 0.000000000000000000, 0.000000000000000000, 1.000000000000000000 ) ) ;
#20367 = CARTESIAN_POINT ( 'NONE',  ( 6.978241445790387409, 28.42397159967988429, 20.50957957746029336 ) ) ;
#20368 = AXIS2_PLACEMENT_3D ( 'NONE', #26394, #23553, #38188 ) ;
#20369 = DIRECTION ( 'NONE',  ( 0.000000000000000000, 0.000000000000000000, 1.000000000000000000 ) ) ;
#20370 = EDGE_LOOP ( 'NONE', ( #29629, #4669, #29153 ) ) ;
#20371 = DIRECTION ( 'NONE',  ( -0.9510565162951504226, 0.3090169943749573322, 0.000000000000000000 ) ) ;
#20372 = CARTESIAN_POINT ( 'NONE',  ( 2.122071298695014541, 21.02571388690864751, -26.27783819818665734 ) ) ;
#20373 = LINE ( 'NONE', #4925, #25572 ) ;
#20374 = AXIS2_PLACEMENT_3D ( 'NONE', #39693, #36453, #31152 ) ;
#20375 = CARTESIAN_POINT ( 'NONE',  ( 9.576215452290895769, 12.54651180042800718, 20.99999999999999645 ) ) ;
#20376 = CARTESIAN_POINT ( 'NONE',  ( 19.37949815655151298, -26.73439600029011487, -8.164662001533008251 ) ) ;
#20377 = DIRECTION ( 'NONE',  ( 0.000000000000000000, 0.000000000000000000, 1.000000000000000000 ) ) ;
#20378 = PLANE ( 'NONE',  #38433 ) ;
#20379 = CARTESIAN_POINT ( 'NONE',  ( -11.78894649379783388, 21.72623886970244911, 12.00000000000000000 ) ) ;
#20380 = ORIENTED_EDGE ( 'NONE', *, *, #23289, .T. ) ;
#20381 = CARTESIAN_POINT ( 'NONE',  ( 10.95089924463749220, 17.48332310871153794, -28.07209419957614216 ) ) ;
#20382 = ORIENTED_EDGE ( 'NONE', *, *, #27929, .F. ) ;
#20383 = CARTESIAN_POINT ( 'NONE',  ( -13.83645454411932718, 22.14850785795266574, -15.49917614834808077 ) ) ;
#20384 = CARTESIAN_POINT ( 'NONE',  ( -30.13477841296696269, -9.898407001806557304, 19.99202127657103389 ) ) ;
#20385 = CARTESIAN_POINT ( 'NONE',  ( -14.17145697063249088, 26.57885438195673444, 10.94387467463493735 ) ) ;
#20386 = CARTESIAN_POINT ( 'NONE',  ( 12.69086781283033893, 20.99879331917208347, -18.45872641518607793 ) ) ;
#20387 = EDGE_LOOP ( 'NONE', ( #12163, #13444, #30645, #15252, #29730, #13794, #20946, #23581 ) ) ;
#20388 = CARTESIAN_POINT ( 'NONE',  ( 31.77418123208467549, -18.80321225436984633, -9.280942705184974884 ) ) ;
#20389 = EDGE_CURVE ( 'NONE', #21146, #2261, #32107, .T. ) ;
#20390 = ORIENTED_EDGE ( 'NONE', *, *, #23510, .F. ) ;
#20392 = CARTESIAN_POINT ( 'NONE',  ( -2.853172919594720192, 21.57294901687549427, 6.000000000000000000 ) ) ;
#20391 = CARTESIAN_POINT ( 'NONE',  ( -14.61013790624355302, 27.97863390761640900, -8.234326149446673071 ) ) ;
#20393 = CARTESIAN_POINT ( 'NONE',  ( -10.34184770646355922, -17.97369560806122735, -27.39515243922713594 ) ) ;
#20394 = CARTESIAN_POINT ( 'NONE',  ( -5.706342468480190000, 20.64589803375067945, 13.00000000000000178 ) ) ;
#20395 = CIRCLE ( 'NONE', #28180, 0.4999999999999986122 ) ;
#20396 = ORIENTED_EDGE ( 'NONE', *, *, #10139, .F. ) ;
#20397 = CARTESIAN_POINT ( 'NONE',  ( -25.39605442066326901, -11.39641072833809865, -17.62077034726572577 ) ) ;
#20398 = CARTESIAN_POINT ( 'NONE',  ( -14.96511953850379939, -26.58463093893972484, -5.946192477338447802 ) ) ;
#20399 = DIRECTION ( 'NONE',  ( 0.000000000000000000, 0.000000000000000000, 1.000000000000000000 ) ) ;
#20400 = CARTESIAN_POINT ( 'NONE',  ( 15.73537490736885402, 20.22929917737018712, -13.69120337137130861 ) ) ;
#20401 = ORIENTED_EDGE ( 'NONE', *, *, #10628, .F. ) ;
#20402 = CARTESIAN_POINT ( 'NONE',  ( 28.74059262234505852, 2.003791175848793849, -7.369499878552438155 ) ) ;
#20403 = CARTESIAN_POINT ( 'NONE',  ( -8.412270287199723029, 10.07085245822962349, 10.49999999999999112 ) ) ;
#20404 = CARTESIAN_POINT ( 'NONE',  ( -37.88915195766744404, -19.37406375362002464, 23.00000000000093792 ) ) ;
#20405 = ORIENTED_EDGE ( 'NONE', *, *, #10877, .F. ) ;
#20406 = CARTESIAN_POINT ( 'NONE',  ( -30.44000904125844187, -0.09666380877237282232, -8.292869882052704256 ) ) ;
#20407 = CARTESIAN_POINT ( 'NONE',  ( 31.30187684039734819, -0.7690320538238586412, -7.331994754779891821 ) ) ;
#20408 = VECTOR ( 'NONE', #15063, 1000.000000000000000 ) ;
#20409 = CARTESIAN_POINT ( 'NONE',  ( 27.04163063101144715, -21.95895612274795283, 18.87996532025750795 ) ) ;
#20410 = EDGE_LOOP ( 'NONE', ( #32444, #20260, #11998, #10700 ) ) ;
#20411 = CARTESIAN_POINT ( 'NONE',  ( -29.05832138661633124, 1.740516625605465828, -6.894049278760337351 ) ) ;
#20412 = CARTESIAN_POINT ( 'NONE',  ( -1.775381057445013511E-14, 40.84107189184581443, -14.51648065752882566 ) ) ;
#20413 = VECTOR ( 'NONE', #30273, 1000.000000000000114 ) ;
#20414 = CARTESIAN_POINT ( 'NONE',  ( 14.70623423376107475, 19.54590544129782614, 7.000000000000000000 ) ) ;
#20415 = DIRECTION ( 'NONE',  ( 1.000000000000000000, 0.000000000000000000, 0.000000000000000000 ) ) ;
#20416 = AXIS2_PLACEMENT_3D ( 'NONE', #39836, #33952, #6109 ) ;
#20417 = CARTESIAN_POINT ( 'NONE',  ( -8.505700342264141511, 22.10876900990917804, 9.000000000000001776 ) ) ;
#20418 = DIRECTION ( 'NONE',  ( 0.000000000000000000, 0.000000000000000000, 1.000000000000000000 ) ) ;
#20419 = CYLINDRICAL_SURFACE ( 'NONE', #39288, 1.000000000000000888 ) ;
#20420 = EDGE_LOOP ( 'NONE', ( #27913, #24348, #33180, #8639 ) ) ;
#20421 = CARTESIAN_POINT ( 'NONE',  ( -20.05673146015622521, 4.300176513202893958, -29.39846272892710388 ) ) ;
#20422 = CARTESIAN_POINT ( 'NONE',  ( -1.829593030691901284E-15, 22.50000000000001066, 23.00000000000000000 ) ) ;
#20423 = DIRECTION ( 'NONE',  ( 0.000000000000000000, 0.000000000000000000, 1.000000000000000000 ) ) ;
#20424 = CARTESIAN_POINT ( 'NONE',  ( 15.35557683603447465, -14.15435181208574988, -27.05163929191509098 ) ) ;
#20425 = DIRECTION ( 'NONE',  ( 1.000000000000000000, 0.000000000000000000, 0.000000000000000000 ) ) ;
#20426 = DIRECTION ( 'NONE',  ( 0.7032331762534049791, 0.07391278520355976100, -0.7071067811865475727 ) ) ;
#20427 = CARTESIAN_POINT ( 'NONE',  ( 15.25529914957406952, 27.06982126769854347, -6.410865638208865569 ) ) ;
#20428 = DIRECTION ( 'NONE',  ( 0.1564344650402246795, -0.9876883405951386585, 0.000000000000000000 ) ) ;
#20429 = ORIENTED_EDGE ( 'NONE', *, *, #29925, .T. ) ;
#20430 = CARTESIAN_POINT ( 'NONE',  ( -16.60320053658520578, 21.21075288159243399, -9.787007994218763329 ) ) ;
#20431 = CARTESIAN_POINT ( 'NONE',  ( -23.74914942275198015, -8.582573258223680668, 20.99999999999999645 ) ) ;
#20432 = EDGE_CURVE ( 'NONE', #23885, #1824, #24371, .T. ) ;
#20433 = CARTESIAN_POINT ( 'NONE',  ( 10.16741497705453767, -19.18446152325294918, -23.86097873014023563 ) ) ;
#20434 = CARTESIAN_POINT ( 'NONE',  ( -13.30736835487442349, 15.68301270189233954, 11.00000000000000000 ) ) ;
#20435 = CARTESIAN_POINT ( 'NONE',  ( 15.24022193870092323, 26.37920915382371945, -7.827918218439406495 ) ) ;
#20436 = ORIENTED_EDGE ( 'NONE', *, *, #7533, .F. ) ;
#20437 = CARTESIAN_POINT ( 'NONE',  ( -13.95683075005230123, 28.08631143191951551, 10.49999999999999822 ) ) ;
#20438 = ORIENTED_EDGE ( 'NONE', *, *, #5751, .F. ) ;
#20440 = DIRECTION ( 'NONE',  ( -0.000000000000000000, -0.000000000000000000, -1.000000000000000000 ) ) ;
#20439 = CARTESIAN_POINT ( 'NONE',  ( -12.84659171310743808, 21.78875632697887355, -17.41907714049541411 ) ) ;
#20441 = CARTESIAN_POINT ( 'NONE',  ( -15.10428467780321604, -26.15168814349211956, -8.766821641356482786 ) ) ;
#20442 = CARTESIAN_POINT ( 'NONE',  ( -31.38526299860031088, -24.75545609243350853, 11.00000000000000000 ) ) ;
#20443 = AXIS2_PLACEMENT_3D ( 'NONE', #37958, #32680, #20280 ) ;
#20444 = CARTESIAN_POINT ( 'NONE',  ( -23.93117376754405612, -14.45163223871617042, -17.59434270118057242 ) ) ;
#20445 = CARTESIAN_POINT ( 'NONE',  ( -4.698712440877560681, -19.95451542538867784, -29.41287879531005345 ) ) ;
#20446 = CARTESIAN_POINT ( 'NONE',  ( 15.40307908694031802, 23.98740442282029761, -10.21161987371616142 ) ) ;
#20447 = EDGE_CURVE ( 'NONE', #34816, #1059, #11282, .T. ) ;
#20448 = ORIENTED_EDGE ( 'NONE', *, *, #25241, .F. ) ;
#20449 = CARTESIAN_POINT ( 'NONE',  ( 19.71920213142633571, 7.415869230238018694, -24.35972737311789516 ) ) ;
#20450 = DIRECTION ( 'NONE',  ( 1.000000000000000000, 0.000000000000000000, 0.000000000000000000 ) ) ;
#20451 = CARTESIAN_POINT ( 'NONE',  ( -15.33886719106936170, -26.70425067113273698, -5.000000000000000000 ) ) ;
#20452 = EDGE_CURVE ( 'NONE', #9748, #25178, #35764, .T. ) ;
#20453 = DIRECTION ( 'NONE',  ( -0.000000000000000000, -0.000000000000000000, -1.000000000000000000 ) ) ;
#20454 = AXIS2_PLACEMENT_3D ( 'NONE', #17186, #38500, #16777 ) ;
#20455 = VERTEX_POINT ( 'NONE', #8527 ) ;
#20456 = CARTESIAN_POINT ( 'NONE',  ( -20.49395421059513467, -1.780101454358719915, -28.61385821411536767 ) ) ;
#20457 = AXIS2_PLACEMENT_3D ( 'NONE', #7251, #29602, #35298 ) ;
#20458 = CARTESIAN_POINT ( 'NONE',  ( -6.462764152204137247, 17.91932574235844555, 20.99999999999999645 ) ) ;
#20459 = CARTESIAN_POINT ( 'NONE',  ( 24.20198940123945519, -6.620595927254128377, 20.94377226548378346 ) ) ;
#20460 = CARTESIAN_POINT ( 'NONE',  ( 19.30730118283910812, -16.27608008926517869, 20.99999999999999645 ) ) ;
#20461 = DIRECTION ( 'NONE',  ( 0.000000000000000000, -0.5906904945688817854, 0.8068982213550663918 ) ) ;
#20462 = CARTESIAN_POINT ( 'NONE',  ( 28.24618586764199080, -13.39106098617326168, -14.74144434279989468 ) ) ;
#20463 = DIRECTION ( 'NONE',  ( -0.000000000000000000, -0.000000000000000000, -1.000000000000000000 ) ) ;
#20464 = EDGE_CURVE ( 'NONE', #20641, #15085, #11681, .T. ) ;
#20465 = ORIENTED_EDGE ( 'NONE', *, *, #32081, .T. ) ;
#20466 = ADVANCED_FACE ( 'NONE', ( #4477, #20527 ), #20325, .T. ) ;
#20467 = DIRECTION ( 'NONE',  ( 1.000000000000000000, 0.000000000000000000, 0.000000000000000000 ) ) ;
#20468 = VECTOR ( 'NONE', #23176, 1000.000000000000227 ) ;
#20469 = DIRECTION ( 'NONE',  ( 0.7431448254773863615, -0.6691306063588671194, 0.000000000000000000 ) ) ;
#20470 = DIRECTION ( 'NONE',  ( 1.000000000000000000, 0.000000000000000000, 0.000000000000000000 ) ) ;
#20471 = CARTESIAN_POINT ( 'NONE',  ( 0.9279571259586922860, 22.81800067625227157, -22.98705170056795311 ) ) ;
#20472 = DIRECTION ( 'NONE',  ( 0.000000000000000000, 0.000000000000000000, 1.000000000000000000 ) ) ;
#20473 = CARTESIAN_POINT ( 'NONE',  ( 0.5000000000000005551, 33.00000000000000000, 10.50000000000000000 ) ) ;
#20474 = AXIS2_PLACEMENT_3D ( 'NONE', #9230, #2933, #15721 ) ;
#20475 = CARTESIAN_POINT ( 'NONE',  ( 1.000000000000000666, 32.50000000000000000, 10.50000000000000178 ) ) ;
#20476 = CYLINDRICAL_SURFACE ( 'NONE', #17098, 62.00000000000014211 ) ;
#20477 = CARTESIAN_POINT ( 'NONE',  ( 6.354454053420411697, 35.54304081427980577, 9.000000000000001776 ) ) ;
#20478 = CARTESIAN_POINT ( 'NONE',  ( 9.842964772816607422, 17.98588232539188425, -30.00000000000000000 ) ) ;
#20480 = VECTOR ( 'NONE', #21406, 1000.000000000000114 ) ;
#20479 = DIRECTION ( 'NONE',  ( -0.9510565162951507556, 0.3090169943749560000, 0.000000000000000000 ) ) ;
#20481 = EDGE_LOOP ( 'NONE', ( #23990, #30826, #32496 ) ) ;
#20484 = DIRECTION ( 'NONE',  ( 0.2185080122244080769, -0.6724985119639556030, -0.7071067811865499042 ) ) ;
#20483 = AXIS2_PLACEMENT_3D ( 'NONE', #404, #18690, #18888 ) ;
#20482 = CARTESIAN_POINT ( 'NONE',  ( -19.11280093006975989, 16.54705272908905656, -7.416057572179566293 ) ) ;
#20485 = CARTESIAN_POINT ( 'NONE',  ( -0.8223886111233146279, 37.39061994947693535, 10.49999999999999822 ) ) ;
#20486 = CARTESIAN_POINT ( 'NONE',  ( 9.523339034571952411, -18.15368110581538019, -29.34782467990711652 ) ) ;
#20487 = DIRECTION ( 'NONE',  ( -0.000000000000000000, -0.000000000000000000, -1.000000000000000000 ) ) ;
#20488 = CARTESIAN_POINT ( 'NONE',  ( 14.52155348942260815, 25.00168942016326667, -11.59674793591240949 ) ) ;
#20489 = CARTESIAN_POINT ( 'NONE',  ( -14.97277451176450924, 21.48159783397892397, 10.49999999999999822 ) ) ;
#20490 = ADVANCED_FACE ( 'NONE', ( #36164 ), #10981, .T. ) ;
#20491 = CARTESIAN_POINT ( 'NONE',  ( -13.53057405073934838, 22.08338764125509002, 10.50000000000000000 ) ) ;
#20492 = CARTESIAN_POINT ( 'NONE',  ( -17.73299320380208144, -16.64144535103558553, -20.85865150295031967 ) ) ;
#20493 = CARTESIAN_POINT ( 'NONE',  ( 2.749517794474013233, -20.36689819698734993, -30.00000000000001421 ) ) ;
#20494 = CARTESIAN_POINT ( 'NONE',  ( 15.54167675008477723, 26.33752833710220997, -5.474103952296149878 ) ) ;
#20495 = CARTESIAN_POINT ( 'NONE',  ( 16.72854773719623012, 11.96534557194348913, -28.29306212330370585 ) ) ;
#20496 = DIRECTION ( 'NONE',  ( 0.000000000000000000, 0.000000000000000000, 1.000000000000000000 ) ) ;
#20497 = ORIENTED_EDGE ( 'NONE', *, *, #31463, .T. ) ;
#20498 = CARTESIAN_POINT ( 'NONE',  ( -5.263199493313895694, 30.38423091068325732, -14.78917777124115318 ) ) ;
#20499 = ORIENTED_EDGE ( 'NONE', *, *, #25393, .T. ) ;
#20500 = CYLINDRICAL_SURFACE ( 'NONE', #28032, 0.4999999999999997780 ) ;
#20501 = VERTEX_POINT ( 'NONE', #16882 ) ;
#20502 = LINE ( 'NONE', #17461, #25200 ) ;
#20503 = CARTESIAN_POINT ( 'NONE',  ( 5.330070799514983193, 27.28854476845134513, 6.000000000000000000 ) ) ;
#20504 = ORIENTED_EDGE ( 'NONE', *, *, #8115, .F. ) ;
#20505 = AXIS2_PLACEMENT_3D ( 'NONE', #836, #10183, #31715 ) ;
#20506 = CARTESIAN_POINT ( 'NONE',  ( -26.37949901244907380, 0.4700838887049326176, -15.46553941099261742 ) ) ;
#20507 = ORIENTED_EDGE ( 'NONE', *, *, #33558, .T. ) ;
#20508 = CARTESIAN_POINT ( 'NONE',  ( 25.18967108100165220, -7.598938349516441981, -18.76223645604332191 ) ) ;
#20509 = VECTOR ( 'NONE', #37950, 1000.000000000000000 ) ;
#20510 = AXIS2_PLACEMENT_3D ( 'NONE', #31418, #2791, #34470 ) ;
#20511 = AXIS2_PLACEMENT_3D ( 'NONE', #11581, #32317, #39604 ) ;
#20512 = ORIENTED_EDGE ( 'NONE', *, *, #21052, .F. ) ;
#20513 = DIRECTION ( 'NONE',  ( 1.000000000000000000, 0.000000000000000000, 0.000000000000000000 ) ) ;
#20514 = VERTEX_POINT ( 'NONE', #29261 ) ;
#20515 = EDGE_CURVE ( 'NONE', #39304, #2159, #23370, .T. ) ;
#20516 = DIRECTION ( 'NONE',  ( 0.000000000000000000, 0.000000000000000000, 1.000000000000000000 ) ) ;
#20517 = DIRECTION ( 'NONE',  ( 1.224646799147353207E-16, 1.000000000000000000, -0.000000000000000000 ) ) ;
#20518 = CARTESIAN_POINT ( 'NONE',  ( -5.440908595777636414, 35.94977745735568675, 9.000000000000001776 ) ) ;
#20519 = VERTEX_POINT ( 'NONE', #5278 ) ;
#20520 = DIRECTION ( 'NONE',  ( 1.000000000000000000, 0.000000000000000000, 0.000000000000000000 ) ) ;
#20521 = CARTESIAN_POINT ( 'NONE',  ( -3.370709253380788084E-06, 22.50000000000031264, 13.00000000000000178 ) ) ;
#20522 = CARTESIAN_POINT ( 'NONE',  ( -2.113580199870562559, 27.06415334822006002, 23.00000000000000355 ) ) ;
#20523 = CARTESIAN_POINT ( 'NONE',  ( 18.59382115548298131, 17.96292538557851515, -5.479430875336894324 ) ) ;
#20524 = CARTESIAN_POINT ( 'NONE',  ( 10.90930865498974178, 30.88252674679933918, -11.23868371367947283 ) ) ;
#20525 = ORIENTED_EDGE ( 'NONE', *, *, #12742, .F. ) ;
#20526 = DIRECTION ( 'NONE',  ( 0.000000000000000000, 0.000000000000000000, 1.000000000000000000 ) ) ;
#20527 = FACE_BOUND ( 'NONE', #39172, .T. ) ;
#20528 = CARTESIAN_POINT ( 'NONE',  ( 14.86587968135671112, -25.51001094038641526, -10.63804553132061237 ) ) ;
#20529 = DIRECTION ( 'NONE',  ( 0.000000000000000000, 0.000000000000000000, 1.000000000000000000 ) ) ;
#20530 = AXIS2_PLACEMENT_3D ( 'NONE', #7528, #10993, #23579 ) ;
#20531 = CARTESIAN_POINT ( 'NONE',  ( 22.52744239175980567, -0.1803094636422790109, -30.00000000000000000 ) ) ;
#20532 = EDGE_CURVE ( 'NONE', #28626, #33852, #2042, .T. ) ;
#20533 = CARTESIAN_POINT ( 'NONE',  ( -13.48645580646731545, 22.82557474682550946, -15.44962328438105281 ) ) ;
#20534 = AXIS2_PLACEMENT_3D ( 'NONE', #39514, #14534, #21034 ) ;
#20535 = CARTESIAN_POINT ( 'NONE',  ( -34.36758591766905369, -1.941406924250941302, 13.92931973827763059 ) ) ;
#20536 = CARTESIAN_POINT ( 'NONE',  ( 11.27276115634963105, -22.55032744237014697, -16.54627474825828770 ) ) ;
#20537 = EDGE_CURVE ( 'NONE', #19050, #10078, #35560, .T. ) ;
#20538 = AXIS2_PLACEMENT_3D ( 'NONE', #1096, #35423, #23234 ) ;
#20539 = CARTESIAN_POINT ( 'NONE',  ( 14.09933648065468503, 26.02968990214155198, 9.500000000000000000 ) ) ;
#20540 = ORIENTED_EDGE ( 'NONE', *, *, #34226, .T. ) ;
#20541 = ORIENTED_EDGE ( 'NONE', *, *, #35490, .T. ) ;
#20542 = CARTESIAN_POINT ( 'NONE',  ( -10.56723897001253931, 29.14243252867948186, -13.10880484156706238 ) ) ;
#20543 = DIRECTION ( 'NONE',  ( 0.8090169943749426773, -0.5877852522924797984, 0.000000000000000000 ) ) ;
#20544 = LINE ( 'NONE', #18295, #5560 ) ;
#20545 = ADVANCED_FACE ( 'NONE', ( #5081 ), #14018, .T. ) ;
#20546 = CARTESIAN_POINT ( 'NONE',  ( -20.99207129727855303, -3.171358742653616059, -25.88939096934664263 ) ) ;
#20547 = CARTESIAN_POINT ( 'NONE',  ( -12.80736835487442349, 15.68301270189233954, 7.000000000000000000 ) ) ;
#20548 = ORIENTED_EDGE ( 'NONE', *, *, #4738, .T. ) ;
#20549 = CARTESIAN_POINT ( 'NONE',  ( 25.82638031820449953, 0.3809398316192084688, -16.44928196465088988 ) ) ;
#20550 = FACE_OUTER_BOUND ( 'NONE', #24885, .T. ) ;
#20551 = DIRECTION ( 'NONE',  ( 0.000000000000000000, 0.000000000000000000, 1.000000000000000000 ) ) ;
#20552 = DIRECTION ( 'NONE',  ( 0.000000000000000000, 0.000000000000000000, 1.000000000000000000 ) ) ;
#20553 = ORIENTED_EDGE ( 'NONE', *, *, #9753, .T. ) ;
#20554 = CARTESIAN_POINT ( 'NONE',  ( -22.72740238869282692, 0.6216207654525480741, -21.61878617671870018 ) ) ;
#20555 = PLANE ( 'NONE',  #17054 ) ;
#20556 = ORIENTED_EDGE ( 'NONE', *, *, #36254, .T. ) ;
#20557 = CARTESIAN_POINT ( 'NONE',  ( 33.18519186262097520, -5.002662412273467751, -9.016556272618601042 ) ) ;
#20558 = CARTESIAN_POINT ( 'NONE',  ( 34.64424588159074148, -17.94331620955155771, 15.72805884748941097 ) ) ;
#20559 = ORIENTED_EDGE ( 'NONE', *, *, #14664, .T. ) ;
#20560 = CARTESIAN_POINT ( 'NONE',  ( 15.23841289164144541, 30.59360923276694777, 14.53008259254005985 ) ) ;
#20561 = ADVANCED_FACE ( 'NONE', ( #17288 ), #29661, .F. ) ;
#20562 = CARTESIAN_POINT ( 'NONE',  ( -5.531500846456688159, -21.05812563137664739, 19.27171037444156809 ) ) ;
#20563 = ADVANCED_FACE ( 'NONE', ( #1843 ), #38940, .T. ) ;
#20564 = DIRECTION ( 'NONE',  ( -0.6691306063588653430, -0.7431448254773878048, 0.000000000000000000 ) ) ;
#20565 = EDGE_CURVE ( 'NONE', #31137, #21311, #32453, .T. ) ;
#20566 = CARTESIAN_POINT ( 'NONE',  ( -6.700679222775207610E-14, 30.76432767446199534, 20.69868183039781329 ) ) ;
#20567 = AXIS2_PLACEMENT_3D ( 'NONE', #9053, #23888, #11900 ) ;
#20568 = AXIS2_PLACEMENT_3D ( 'NONE', #4741, #14076, #35823 ) ;
#20569 = CARTESIAN_POINT ( 'NONE',  ( -3.607749162633401951, 7.931741834401822899, 10.63089969389957190 ) ) ;
#20570 = EDGE_LOOP ( 'NONE', ( #34428, #15214, #1668, #37274 ) ) ;
#20571 = CARTESIAN_POINT ( 'NONE',  ( -9.806982162272253944, 13.84996144622306247, 6.000000000000000000 ) ) ;
#20572 = CARTESIAN_POINT ( 'NONE',  ( -4.625823320348136036, 31.66047261929882950, 10.75000000000000888 ) ) ;
#20573 = CARTESIAN_POINT ( 'NONE',  ( 5.518227685048840314, 33.48242281877398341, -12.00997661136522510 ) ) ;
#20574 = CARTESIAN_POINT ( 'NONE',  ( 8.118377661053324701, 10.47536095541698486, 7.000000000000000000 ) ) ;
#20575 = CARTESIAN_POINT ( 'NONE',  ( 23.18043107533613068, 0.3100950997233969386, 19.99202127658098505 ) ) ;
#20576 = CARTESIAN_POINT ( 'NONE',  ( 12.27390640609045036, -16.43329545370340838, -29.99999999999998934 ) ) ;
#20577 = LINE ( 'NONE', #32973, #4806 ) ;
#20578 = CARTESIAN_POINT ( 'NONE',  ( -13.14565529531520127, 15.48770264576553402, 10.82238833324609750 ) ) ;
#20579 = DIRECTION ( 'NONE',  ( 0.000000000000000000, 0.000000000000000000, 1.000000000000000000 ) ) ;
#20580 = VERTEX_POINT ( 'NONE', #11179 ) ;
#20581 = EDGE_CURVE ( 'NONE', #10337, #33798, #5181, .T. ) ;
#20582 = CARTESIAN_POINT ( 'NONE',  ( 14.79314896790873135, 25.75459063161006767, -10.17147167629895144 ) ) ;
#20584 = VERTEX_POINT ( 'NONE', #10775 ) ;
#20583 = EDGE_CURVE ( 'NONE', #37593, #10104, #35965, .T. ) ;
#20585 = CARTESIAN_POINT ( 'NONE',  ( -11.29390458575034373, 17.10922195600983997, -29.35494707390875746 ) ) ;
#20586 = CARTESIAN_POINT ( 'NONE',  ( -20.42855823444361363, -24.24606183460709374, 18.87996532025784902 ) ) ;
#20587 = ADVANCED_FACE ( 'NONE', ( #11382 ), #27017, .F. ) ;
#20588 = CARTESIAN_POINT ( 'NONE',  ( 12.03640989728592459, 29.14264673470096767, 6.000000000000000000 ) ) ;
#20589 = CARTESIAN_POINT ( 'NONE',  ( 14.89811268554684176, 25.43506582924968029, -10.18359384596507056 ) ) ;
#20590 = ORIENTED_EDGE ( 'NONE', *, *, #36600, .F. ) ;
#20591 = CARTESIAN_POINT ( 'NONE',  ( 32.18353893966516921, -20.39468426946134016, -7.117916671018453378 ) ) ;
#20592 = ORIENTED_EDGE ( 'NONE', *, *, #25093, .T. ) ;
#20594 = LINE ( 'NONE', #5143, #37433 ) ;
#20593 = CARTESIAN_POINT ( 'NONE',  ( -14.36325139127783501, 27.43616443481291256, -9.622046172864397562 ) ) ;
#20595 = CARTESIAN_POINT ( 'NONE',  ( -16.93610668433033339, -26.60906881091851872, -8.235790559075788053 ) ) ;
#20596 = DIRECTION ( 'NONE',  ( 1.000000000000000000, 0.000000000000000000, 0.000000000000000000 ) ) ;
#20597 = CONICAL_SURFACE ( 'NONE', #38082, 0.5000000000000002220, 0.7853981633974517207 ) ;
#20598 = ORIENTED_EDGE ( 'NONE', *, *, #29827, .F. ) ;
#20599 = CARTESIAN_POINT ( 'NONE',  ( -19.74691339681017865, -6.824302415588217485, -27.02994878819155034 ) ) ;
#20600 = CARTESIAN_POINT ( 'NONE',  ( -14.39692894930127487, -25.73270398672122994, -9.716188519315773320 ) ) ;
#20601 = CARTESIAN_POINT ( 'NONE',  ( 20.92112759555542922, -16.07000418475249859, 23.00000000000000000 ) ) ;
#20602 = ORIENTED_EDGE ( 'NONE', *, *, #37982, .T. ) ;
#20603 = CARTESIAN_POINT ( 'NONE',  ( 20.36878409817081703, 2.417852450439662348, -29.37451754486702171 ) ) ;
#20604 = CARTESIAN_POINT ( 'NONE',  ( -12.68475447279705115, 27.14725768220950286, 7.000000000000000000 ) ) ;
#20605 = CARTESIAN_POINT ( 'NONE',  ( 6.557822374958316658, 35.99981354310111215, 7.000000000000000000 ) ) ;
#20606 = CONICAL_SURFACE ( 'NONE', #25772, 0.4999999999999961142, 0.7853981633974463916 ) ;
#20607 = VERTEX_POINT ( 'NONE', #33530 ) ;
#20608 = CARTESIAN_POINT ( 'NONE',  ( -20.48447659325206516, 0.7979435291051002466, -29.34725074627716879 ) ) ;
#20609 = CARTESIAN_POINT ( 'NONE',  ( 20.86812861272620978, 0.01623219257051957895, -26.76714782918698532 ) ) ;
#20610 = AXIS2_PLACEMENT_3D ( 'NONE', #18028, #38952, #1990 ) ;
#20611 = CARTESIAN_POINT ( 'NONE',  ( 29.77271197308713724, -3.128983846829581861, 18.87996532025967511 ) ) ;
#20612 = ORIENTED_EDGE ( 'NONE', *, *, #30393, .F. ) ;
#20613 = CARTESIAN_POINT ( 'NONE',  ( -24.19505052999625150, 1.198773395227752836, -18.53314538056739025 ) ) ;
#20614 = CARTESIAN_POINT ( 'NONE',  ( -19.79815887584811307, 19.84782313723621883, -13.42901749168595771 ) ) ;
#20615 = EDGE_CURVE ( 'NONE', #36809, #22772, #15159, .T. ) ;
#20616 = CARTESIAN_POINT ( 'NONE',  ( 14.78558495942256990, 19.97203773654679537, 7.338691926023217071 ) ) ;
#20617 = CARTESIAN_POINT ( 'NONE',  ( -15.27443809246124218, -27.57253143578281041, 15.13084544680213739 ) ) ;
#20618 = AXIS2_PLACEMENT_3D ( 'NONE', #40016, #12194, #24589 ) ;
#20619 = AXIS2_PLACEMENT_3D ( 'NONE', #28127, #2751, #21830 ) ;
#20620 = CARTESIAN_POINT ( 'NONE',  ( -1.974612014229268020, 7.629979921222117767, 7.203056206335834766 ) ) ;
#20621 = DIRECTION ( 'NONE',  ( 0.000000000000000000, 0.000000000000000000, 1.000000000000000000 ) ) ;
#20622 = CARTESIAN_POINT ( 'NONE',  ( 3.357189294653307954, 32.49896394832310165, 10.49999999999999467 ) ) ;
#20623 = ORIENTED_EDGE ( 'NONE', *, *, #28381, .F. ) ;
#20624 = CARTESIAN_POINT ( 'NONE',  ( -26.03581645590561422, 5.301338185016732929, -7.395082201969008118 ) ) ;
#20625 = FACE_OUTER_BOUND ( 'NONE', #23580, .T. ) ;
#20626 = FACE_OUTER_BOUND ( 'NONE', #12962, .T. ) ;
#20627 = CARTESIAN_POINT ( 'NONE',  ( 18.00180999299007212, -17.62873692815191617, -19.82092202452991003 ) ) ;
#20628 = DIRECTION ( 'NONE',  ( 1.000000000000000000, 0.000000000000000000, 0.000000000000000000 ) ) ;
#20629 = CARTESIAN_POINT ( 'NONE',  ( -14.86556419889029890, 20.43481210330121556, 10.50000000000000000 ) ) ;
#20630 = CARTESIAN_POINT ( 'NONE',  ( 10.63104621300768216, 17.52826713075782905, -30.00000000000000355 ) ) ;
#20631 = AXIS2_PLACEMENT_3D ( 'NONE', #22033, #28326, #22421 ) ;
#20632 = CARTESIAN_POINT ( 'NONE',  ( -10.09822582592804174, -27.41751403069116222, 11.55979286845328069 ) ) ;
#20633 = ORIENTED_EDGE ( 'NONE', *, *, #17533, .F. ) ;
#20634 = CARTESIAN_POINT ( 'NONE',  ( -16.99205359343081057, 21.87216257061389157, -5.475577676556287798 ) ) ;
#20635 = CARTESIAN_POINT ( 'NONE',  ( -23.81569860407211436, -13.74999999999980105, 20.99999999999999645 ) ) ;
#20636 = EDGE_CURVE ( 'NONE', #29833, #10872, #15022, .T. ) ;
#20637 = CARTESIAN_POINT ( 'NONE',  ( 13.97557076678965693, 21.53386246193694475, 7.000000000000000000 ) ) ;
#20638 = CARTESIAN_POINT ( 'NONE',  ( 11.90609510123815262, 19.36740028416927828, -21.61948926389480263 ) ) ;
#20639 = ORIENTED_EDGE ( 'NONE', *, *, #15796, .F. ) ;
#20640 = FACE_OUTER_BOUND ( 'NONE', #11643, .T. ) ;
#20641 = VERTEX_POINT ( 'NONE', #33328 ) ;
#20643 = CARTESIAN_POINT ( 'NONE',  ( 19.48557158514988075, -11.24999999999998224, 6.000000000000000000 ) ) ;
#20642 = CARTESIAN_POINT ( 'NONE',  ( -12.30182166038729008, 20.60945325276725271, -19.47751875586111581 ) ) ;
#20644 = CARTESIAN_POINT ( 'NONE',  ( -9.798063751231428142, -18.55837220631304518, -26.22365102716438656 ) ) ;
#20645 = CARTESIAN_POINT ( 'NONE',  ( -35.07402885326978037, -20.24999999999986855, 11.55979286843934872 ) ) ;
#20646 = CARTESIAN_POINT ( 'NONE',  ( -19.90297529439527935, -11.21068947634444513, -22.98220968216354265 ) ) ;
#20647 = CARTESIAN_POINT ( 'NONE',  ( -8.349547994803288020, -23.65591986291670423, -13.74762987334840680 ) ) ;
#20648 = CARTESIAN_POINT ( 'NONE',  ( 5.305271391459043251, 36.43775379931900460, 10.49999999999999822 ) ) ;
#20649 = CARTESIAN_POINT ( 'NONE',  ( 11.73765114802458953, 17.34560416271227012, -26.28214589256836575 ) ) ;
#20650 = ORIENTED_EDGE ( 'NONE', *, *, #5317, .F. ) ;
#20651 = CARTESIAN_POINT ( 'NONE',  ( 25.32158894843077945, 6.480252874148680675, -5.000000000000003553 ) ) ;
#20652 = DIRECTION ( 'NONE',  ( -1.000000000000000000, 0.000000000000000000, 0.000000000000000000 ) ) ;
#20653 = LINE ( 'NONE', #14346, #38740 ) ;
#20654 = DIRECTION ( 'NONE',  ( 0.7275037805841029215, 0.3706816908109982767, 0.5773502691896289507 ) ) ;
#20655 = VECTOR ( 'NONE', #34559, 1000.000000000000227 ) ;
#20656 = ORIENTED_EDGE ( 'NONE', *, *, #15801, .T. ) ;
#20657 = CARTESIAN_POINT ( 'NONE',  ( -31.69836596977474485, -1.611888971326790099, -8.225968294365550548 ) ) ;
#20659 = CARTESIAN_POINT ( 'NONE',  ( 29.49705578473263756, -0.08617031093297387867, -10.64064826169365752 ) ) ;
#20658 = AXIS2_PLACEMENT_3D ( 'NONE', #25529, #37733, #37928 ) ;
#20660 = VECTOR ( 'NONE', #12838, 1000.000000000000114 ) ;
#20661 = DIRECTION ( 'NONE',  ( 1.000000000000000000, 0.000000000000000000, -0.000000000000000000 ) ) ;
#20662 = CARTESIAN_POINT ( 'NONE',  ( 24.42249384534429169, -8.161410322277701468, 21.00000000000004619 ) ) ;
#20663 = DIRECTION ( 'NONE',  ( 0.000000000000000000, 0.000000000000000000, -1.000000000000000000 ) ) ;
#20664 = AXIS2_PLACEMENT_3D ( 'NONE', #36447, #8005, #8613 ) ;
#20665 = DIRECTION ( 'NONE',  ( 0.000000000000000000, -0.5778781230734075791, -0.8161230758121935658 ) ) ;
#20667 = VECTOR ( 'NONE', #14648, 1000.000000000000000 ) ;
#20666 = LINE ( 'NONE', #35897, #31695 ) ;
#20668 = ADVANCED_FACE ( 'NONE', ( #39799 ), #5674, .T. ) ;
#20669 = VERTEX_POINT ( 'NONE', #36560 ) ;
#20670 = DIRECTION ( 'NONE',  ( 1.000000000000000000, 0.000000000000000000, 0.000000000000000000 ) ) ;
#20671 = DIRECTION ( 'NONE',  ( -0.000000000000000000, 0.000000000000000000, 1.000000000000000000 ) ) ;
#20672 = EDGE_LOOP ( 'NONE', ( #1821, #20291, #33197, #20781 ) ) ;
#20673 = CARTESIAN_POINT ( 'NONE',  ( 0.3724352543551862627, 34.47678155200587469, -11.97407239485822039 ) ) ;
#20674 = LINE ( 'NONE', #27159, #23695 ) ;
#20675 = DIRECTION ( 'NONE',  ( 0.9781476007338070211, 0.2079116908177534029, -0.000000000000000000 ) ) ;
#20676 = EDGE_CURVE ( 'NONE', #39686, #37976, #27000, .T. ) ;
#20677 = FACE_OUTER_BOUND ( 'NONE', #14657, .T. ) ;
#20678 = CARTESIAN_POINT ( 'NONE',  ( 5.440908595777819379, 35.94977745735560859, 11.00000000000000000 ) ) ;
#20679 = CARTESIAN_POINT ( 'NONE',  ( -7.929471891321301591, 25.60217271033470610, 7.000000000000000000 ) ) ;
#20680 = CARTESIAN_POINT ( 'NONE',  ( 8.917734535019441466, 14.47043272369397116, 12.00000000000000000 ) ) ;
#20681 = VECTOR ( 'NONE', #31465, 999.9999999999998863 ) ;
#20682 = CARTESIAN_POINT ( 'NONE',  ( 10.00001779673401714, 18.34526635362476554, -26.72599099279598889 ) ) ;
#20683 = DIRECTION ( 'NONE',  ( -0.000000000000000000, -0.000000000000000000, -1.000000000000000000 ) ) ;
#20684 = VECTOR ( 'NONE', #4631, 999.9999999999998863 ) ;
#20685 = ORIENTED_EDGE ( 'NONE', *, *, #1717, .T. ) ;
#20687 = CARTESIAN_POINT ( 'NONE',  ( 14.98890121934614506, -28.67928442654198307, -5.000000000000000000 ) ) ;
#20686 = CARTESIAN_POINT ( 'NONE',  ( -16.75542722950669372, 12.74032028316595699, -24.38506794022037383 ) ) ;
#20688 = CARTESIAN_POINT ( 'NONE',  ( -14.08246327825354349, 27.69965426814084353, 10.49999999999999822 ) ) ;
#20689 = CARTESIAN_POINT ( 'NONE',  ( 14.99547355802778981, -25.99396817878668031, -9.237562226852288561 ) ) ;
#20690 = CARTESIAN_POINT ( 'NONE',  ( 1.871201846650637046, 31.30332840660451765, 12.00000000000000000 ) ) ;
#20691 = CARTESIAN_POINT ( 'NONE',  ( 13.75556773078374029, 23.42751890104277024, -14.47297052992422550 ) ) ;
#20692 = DIRECTION ( 'NONE',  ( -0.3090169943749448977, 0.9510565162951543083, 0.000000000000000000 ) ) ;
#20693 = CARTESIAN_POINT ( 'NONE',  ( 5.440908595777814050, 35.94977745735560859, 7.000000000000000000 ) ) ;
#20694 = CIRCLE ( 'NONE', #29664, 56.99999999999991473 ) ;
#20695 = CARTESIAN_POINT ( 'NONE',  ( -27.46546245186472390, -24.32166980333147066, -8.008947335190420347 ) ) ;
#20696 = CARTESIAN_POINT ( 'NONE',  ( 2.964953114717667759, -21.10545243889943734, -23.30365150309269850 ) ) ;
#20697 = CARTESIAN_POINT ( 'NONE',  ( 11.64865060427507082, 18.29505130955256575, -23.87876004802710739 ) ) ;
#20698 = CARTESIAN_POINT ( 'NONE',  ( 18.69768069937141419, 10.45728937905904665, -22.25138797246191302 ) ) ;
#20699 = DIRECTION ( 'NONE',  ( 1.000000000000000000, 0.000000000000000000, 0.000000000000000000 ) ) ;
#20700 = EDGE_CURVE ( 'NONE', #38335, #26227, #8731, .T. ) ;
#20701 = ORIENTED_EDGE ( 'NONE', *, *, #35230, .T. ) ;
#20702 = CARTESIAN_POINT ( 'NONE',  ( -7.186746356396819024, 35.16721044838237020, -9.326795472630500683 ) ) ;
#20703 = ORIENTED_EDGE ( 'NONE', *, *, #8610, .T. ) ;
#20704 = CARTESIAN_POINT ( 'NONE',  ( 5.267154670482129930, 36.54499619867781490, 7.382773698552470343 ) ) ;
#20705 = ORIENTED_EDGE ( 'NONE', *, *, #9512, .F. ) ;
#20706 = DIRECTION ( 'NONE',  ( 1.000000000000000000, 0.000000000000000000, 0.000000000000000000 ) ) ;
#20707 = FACE_OUTER_BOUND ( 'NONE', #26866, .T. ) ;
#20708 = ORIENTED_EDGE ( 'NONE', *, *, #19233, .F. ) ;
#20709 = CARTESIAN_POINT ( 'NONE',  ( -20.68187284593733111, 1.006734202109016429, -27.45854716128443229 ) ) ;
#20710 = EDGE_LOOP ( 'NONE', ( #35167, #22812, #13547, #30525 ) ) ;
#20711 = CARTESIAN_POINT ( 'NONE',  ( 19.87733292414454667, -5.354748204895443564, -28.50879837906193970 ) ) ;
#20712 = CIRCLE ( 'NONE', #20063, 6.000000000000005329 ) ;
#20713 = CIRCLE ( 'NONE', #16170, 1.000000000000000888 ) ;
#20714 = ORIENTED_EDGE ( 'NONE', *, *, #22401, .T. ) ;
#20715 = APPLICATION_PROTOCOL_DEFINITION ( 'draft international standard', 'automotive_design', 1998, #14524 ) ;
#20716 = CARTESIAN_POINT ( 'NONE',  ( 13.60579549876902483, 27.97225316470530387, 10.49999999999999645 ) ) ;
#20717 = ORIENTED_EDGE ( 'NONE', *, *, #29090, .T. ) ;
#20718 = CIRCLE ( 'NONE', #31718, 0.4999999999999989453 ) ;
#20719 = DIRECTION ( 'NONE',  ( 1.000000000000000000, 0.000000000000000000, 0.000000000000000000 ) ) ;
#20720 = CARTESIAN_POINT ( 'NONE',  ( 28.79337657215624446, 4.963436916936688093, 10.99999999998960831 ) ) ;
#20721 = ADVANCED_FACE ( 'NONE', ( #30868 ), #27611, .T. ) ;
#20722 = DIRECTION ( 'NONE',  ( 1.000000000000000000, 0.000000000000000000, 0.000000000000000000 ) ) ;
#20723 = VERTEX_POINT ( 'NONE', #39996 ) ;
#20724 = SURFACE_SIDE_STYLE ('',( #11374 ) ) ;
#20725 = DIRECTION ( 'NONE',  ( 0.000000000000000000, 0.000000000000000000, 1.000000000000000000 ) ) ;
#20726 = CARTESIAN_POINT ( 'NONE',  ( -8.927394655428429360, 11.06314620770957013, 7.000000000000000000 ) ) ;
#20727 = EDGE_CURVE ( 'NONE', #6144, #18451, #6272, .T. ) ;
#20728 = LINE ( 'NONE', #30263, #5906 ) ;
#20729 = CARTESIAN_POINT ( 'NONE',  ( 15.39201892520244641, 13.81047332064365740, -27.12305683531639389 ) ) ;
#20730 = CARTESIAN_POINT ( 'NONE',  ( 12.14007034441317856, 31.71921406358307038, -8.558348499896236916 ) ) ;
#20731 = ORIENTED_EDGE ( 'NONE', *, *, #35845, .F. ) ;
#20732 = CARTESIAN_POINT ( 'NONE',  ( -19.68060073398973842, 9.708938446362566310, -20.11576684351307520 ) ) ;
#20733 = CARTESIAN_POINT ( 'NONE',  ( 8.238488885696289898, 24.65111619403943877, 9.000000000000001776 ) ) ;
#20734 = DIRECTION ( 'NONE',  ( -0.000000000000000000, -0.000000000000000000, -1.000000000000000000 ) ) ;
#20735 = CARTESIAN_POINT ( 'NONE',  ( 11.00987194897382970, -19.94983946540193998, -21.59411760730909080 ) ) ;
#20736 = CARTESIAN_POINT ( 'NONE',  ( 16.77267017469755217, -29.13948811618736912, -5.000000000000003553 ) ) ;
#20737 = DIRECTION ( 'NONE',  ( -0.9510565162951543083, -0.3090169943749450088, -0.000000000000000000 ) ) ;
#20739 = AXIS2_PLACEMENT_3D ( 'NONE', #15564, #25102, #525 ) ;
#20738 = CARTESIAN_POINT ( 'NONE',  ( -11.30484249362164384, 18.04208246058641052, -25.01387445287749145 ) ) ;
#20740 = CARTESIAN_POINT ( 'NONE',  ( -34.08416769313322447, -19.67850339273479676, 15.13084544680213561 ) ) ;
#20741 = CARTESIAN_POINT ( 'NONE',  ( 10.95693405366107953, -22.07055394455351305, -17.55030168376832123 ) ) ;
#20742 = EDGE_CURVE ( 'NONE', #15678, #27267, #13355, .T. ) ;
#20743 = CARTESIAN_POINT ( 'NONE',  ( 13.32679399471731685, 28.40733119287944319, 7.000000000000000000 ) ) ;
#20744 = ADVANCED_FACE ( 'NONE', ( #2833 ), #29619, .T. ) ;
#20745 = EDGE_LOOP ( 'NONE', ( #25782, #3656, #10894, #12274 ) ) ;
#20746 = VERTEX_POINT ( 'NONE', #25354 ) ;
#20747 = CIRCLE ( 'NONE', #33714, 1.000000000000000888 ) ;
#20748 = CARTESIAN_POINT ( 'NONE',  ( -8.456281551504293503, 23.21296397863146410, -20.00008365536006494 ) ) ;
#20749 = DIRECTION ( 'NONE',  ( 0.8090169943749426773, -0.5877852522924797984, 0.000000000000000000 ) ) ;
#20750 = CARTESIAN_POINT ( 'NONE',  ( 9.892954722048896699, 20.95745441963929423, 10.50000000000000533 ) ) ;
#20751 = CARTESIAN_POINT ( 'NONE',  ( -3.211402178667006169, 32.38366924255629442, 12.00000000000000000 ) ) ;
#20752 = EDGE_LOOP ( 'NONE', ( #16748, #12382, #5523, #36005 ) ) ;
#20753 = CARTESIAN_POINT ( 'NONE',  ( 23.28981712441201779, 0.6280063682916672274, -20.55124257728155257 ) ) ;
#20754 = CARTESIAN_POINT ( 'NONE',  ( 6.064564986133971658, 13.54338174056915456, 13.00000000000000178 ) ) ;
#20755 = CARTESIAN_POINT ( 'NONE',  ( -6.778507894852238813, 14.44616049828245785, 10.75000000000001066 ) ) ;
#20756 = CARTESIAN_POINT ( 'NONE',  ( 10.16520467992603294, 20.33931832809677331, 13.00000000000000178 ) ) ;
#20757 = ORIENTED_EDGE ( 'NONE', *, *, #22458, .T. ) ;
#20758 = CARTESIAN_POINT ( 'NONE',  ( -23.30969975423458962, 0.5725924327717566431, -20.54455488908562799 ) ) ;
#20759 = CARTESIAN_POINT ( 'NONE',  ( 11.11016527260166420, 31.83082137946473367, 11.00000000000000000 ) ) ;
#20760 = ORIENTED_EDGE ( 'NONE', *, *, #37842, .T. ) ;
#20761 = CARTESIAN_POINT ( 'NONE',  ( 32.55711526567240810, -3.964017815489828678, -9.499260478695129351 ) ) ;
#20762 = CARTESIAN_POINT ( 'NONE',  ( 30.82617745331448944, -24.12092658898442110, 14.53008259254011492 ) ) ;
#20763 = VERTEX_POINT ( 'NONE', #34912 ) ;
#20764 = CARTESIAN_POINT ( 'NONE',  ( 3.717128218779132798, 39.34929362537322817, 14.53008259254021439 ) ) ;
#20765 = CARTESIAN_POINT ( 'NONE',  ( -17.42101839919755690, -19.25229542401750038, 20.69868183039781329 ) ) ;
#20766 = DIRECTION ( 'NONE',  ( 0.4067366430757889395, -0.9135454576426059736, 0.000000000000000000 ) ) ;
#20767 = EDGE_CURVE ( 'NONE', #839, #36138, #36087, .T. ) ;
#20768 = CARTESIAN_POINT ( 'NONE',  ( 7.164929079093869113, 24.49151390636890824, 20.82122704794079837 ) ) ;
#20769 = AXIS2_PLACEMENT_3D ( 'NONE', #26408, #4873, #29457 ) ;
#20770 = DIRECTION ( 'NONE',  ( 0.000000000000000000, 0.000000000000000000, 1.000000000000000000 ) ) ;
#20771 = ORIENTED_EDGE ( 'NONE', *, *, #31988, .F. ) ;
#20772 = CARTESIAN_POINT ( 'NONE',  ( 14.70623423376107475, 19.54590544129782614, 7.000000000000000000 ) ) ;
#20773 = CYLINDRICAL_SURFACE ( 'NONE', #32531, 0.5000000000000007772 ) ;
#20774 = CARTESIAN_POINT ( 'NONE',  ( 8.026644466976325276, 35.55948074244522417, -8.017818322552109578 ) ) ;
#20775 = DIRECTION ( 'NONE',  ( -0.000000000000000000, -0.000000000000000000, 1.000000000000000000 ) ) ;
#20776 = CARTESIAN_POINT ( 'NONE',  ( 13.32472804388164000, 14.30980730578316873, 20.25080042701575778 ) ) ;
#20777 = CARTESIAN_POINT ( 'NONE',  ( 12.01726265205634725, -17.15496393756174953, -26.62634840083233101 ) ) ;
#20778 = CARTESIAN_POINT ( 'NONE',  ( -4.524139159579191549, 31.43208625488816566, 10.50000000000000000 ) ) ;
#20779 = DIRECTION ( 'NONE',  ( -0.9781476007338072431, -0.2079116908177518208, 0.000000000000000000 ) ) ;
#20780 = LINE ( 'NONE', #2881, #1239 ) ;
#20781 = ORIENTED_EDGE ( 'NONE', *, *, #29494, .T. ) ;
#20782 = CARTESIAN_POINT ( 'NONE',  ( 15.33163471202798789, 26.81437899606220299, -6.414921594359186408 ) ) ;
#20783 = ORIENTED_EDGE ( 'NONE', *, *, #34421, .F. ) ;
#20784 = CARTESIAN_POINT ( 'NONE',  ( -11.37750526317191735, 17.29471388271799981, -27.47106155913822434 ) ) ;
#20785 = CARTESIAN_POINT ( 'NONE',  ( -16.23042486173915933, -23.86708630543300202, 18.87996532025784546 ) ) ;
#20786 = CARTESIAN_POINT ( 'NONE',  ( -14.26801110064877776, 26.12045026487111343, 10.49999999999999822 ) ) ;
#20787 = CARTESIAN_POINT ( 'NONE',  ( 11.39223802988129997, 17.97370404759189810, -25.02557645429753919 ) ) ;
#20788 = ORIENTED_EDGE ( 'NONE', *, *, #28504, .F. ) ;
#20789 = CARTESIAN_POINT ( 'NONE',  ( 31.15403848181932744, -18.43678299216485073, -10.17193552462277850 ) ) ;
#20790 = ORIENTED_EDGE ( 'NONE', *, *, #3908, .F. ) ;
#20792 = CARTESIAN_POINT ( 'NONE',  ( -13.24038105676664401, 15.43301270189234486, 7.000000000000000000 ) ) ;
#20791 = CARTESIAN_POINT ( 'NONE',  ( -15.00988142436982997, 27.11442454588856421, -7.804806528538684063 ) ) ;
#20793 = CARTESIAN_POINT ( 'NONE',  ( -17.26829665777506762, -27.06560434691794015, -5.929067903965382413 ) ) ;
#20794 = LINE ( 'NONE', #11840, #37345 ) ;
#20795 = EDGE_CURVE ( 'NONE', #26036, #22756, #23105, .T. ) ;
#20796 = ORIENTED_EDGE ( 'NONE', *, *, #7684, .T. ) ;
#20797 = CARTESIAN_POINT ( 'NONE',  ( -34.77897381664745069, -11.95873854617616239, -8.005595432382110133 ) ) ;
#20798 = CARTESIAN_POINT ( 'NONE',  ( -14.68417942092947825, -26.35066116812440740, -7.360212364853471634 ) ) ;
#20799 = CARTESIAN_POINT ( 'NONE',  ( 18.76090689389208066, -16.22676322417240868, 23.00000000000000000 ) ) ;
#20800 = EDGE_LOOP ( 'NONE', ( #39169, #11238, #10595 ) ) ;
#20801 = CARTESIAN_POINT ( 'NONE',  ( 20.42176732625024016, 3.104454087777909432, -27.57334092644989099 ) ) ;
#20802 = DIRECTION ( 'NONE',  ( 1.000000000000000000, 0.000000000000000000, 0.000000000000000000 ) ) ;
#20803 = DIRECTION ( 'NONE',  ( 0.000000000000000000, 0.000000000000000000, 1.000000000000000000 ) ) ;
#20804 = ORIENTED_EDGE ( 'NONE', *, *, #19251, .F. ) ;
#20805 = CARTESIAN_POINT ( 'NONE',  ( -27.19884774959017193, 0.1546446106993354663, -14.46771215221622597 ) ) ;
#20806 = ORIENTED_EDGE ( 'NONE', *, *, #15873, .T. ) ;
#20807 = CARTESIAN_POINT ( 'NONE',  ( 31.32859553683839238, -0.9615075054642621133, -7.789356384682906587 ) ) ;
#20808 = CARTESIAN_POINT ( 'NONE',  ( 21.83515197098677163, -24.14400021536937047, 18.87996532025784546 ) ) ;
#20809 = ORIENTED_EDGE ( 'NONE', *, *, #3564, .T. ) ;
#20810 = CARTESIAN_POINT ( 'NONE',  ( -20.21274638685197900, 3.602405235153209873, -28.78677028190584863 ) ) ;
#20811 = CARTESIAN_POINT ( 'NONE',  ( 1.247466774197339978, 28.36888560440311480, 13.00000000000000178 ) ) ;
#20812 = EDGE_CURVE ( 'NONE', #16261, #26640, #39325, .T. ) ;
#20813 = CARTESIAN_POINT ( 'NONE',  ( -13.24038105676664401, 15.43301270189234486, 10.49999999999999822 ) ) ;
#20814 = CIRCLE ( 'NONE', #21443, 0.5000000000000004441 ) ;
#20815 = LINE ( 'NONE', #2126, #36258 ) ;
#20816 = EDGE_CURVE ( 'NONE', #39980, #12345, #19461, .T. ) ;
#20817 = EDGE_CURVE ( 'NONE', #17093, #26001, #411, .T. ) ;
#20818 = DIRECTION ( 'NONE',  ( 1.000000000000000000, 0.000000000000000000, 0.000000000000000000 ) ) ;
#20819 = CYLINDRICAL_SURFACE ( 'NONE', #32703, 0.5000000000000004441 ) ;
#20820 = LINE ( 'NONE', #11672, #20480 ) ;
#20821 = ORIENTED_EDGE ( 'NONE', *, *, #21798, .F. ) ;
#20822 = CARTESIAN_POINT ( 'NONE',  ( -25.50981415929211948, 6.214348039242530319, -5.957670977875550555 ) ) ;
#20823 = DIRECTION ( 'NONE',  ( 1.000000000000000000, 0.000000000000000000, 0.000000000000000000 ) ) ;
#20824 = DIRECTION ( 'NONE',  ( -0.8660254037844364872, 0.5000000000000038858, -0.000000000000000000 ) ) ;
#20825 = CARTESIAN_POINT ( 'NONE',  ( 20.78379507624259759, -21.64473465098445359, -14.89368447040524401 ) ) ;
#20826 = AXIS2_PLACEMENT_3D ( 'NONE', #18273, #27208, #2233 ) ;
#20827 = DIRECTION ( 'NONE',  ( 0.000000000000000000, 0.000000000000000000, 1.000000000000000000 ) ) ;
#20828 = CARTESIAN_POINT ( 'NONE',  ( -14.55573640795744872, 20.46737631633130405, 10.96580508970282253 ) ) ;
#20829 = CARTESIAN_POINT ( 'NONE',  ( 11.21809837322889258, 18.66389468805340357, -23.81189286561465934 ) ) ;
#20830 = CARTESIAN_POINT ( 'NONE',  ( 15.00437666251164792, -28.61930095463398160, 12.14047268033097460 ) ) ;
#20831 = ORIENTED_EDGE ( 'NONE', *, *, #33414, .F. ) ;
#20832 = CARTESIAN_POINT ( 'NONE',  ( -16.52695952976914739, 21.08173666875514130, -10.27124637523843909 ) ) ;
#20833 = CARTESIAN_POINT ( 'NONE',  ( -24.85114452701394328, -15.17411596029591969, 20.94377226548368398 ) ) ;
#20834 = DIRECTION ( 'NONE',  ( -0.000000000000000000, -0.000000000000000000, -1.000000000000000000 ) ) ;
#20835 = CARTESIAN_POINT ( 'NONE',  ( 15.24827013184445335, 26.35192645322203475, -7.828065716477629721 ) ) ;
#20836 = EDGE_LOOP ( 'NONE', ( #7694, #15032, #511, #25592 ) ) ;
#20837 = CARTESIAN_POINT ( 'NONE',  ( -14.81003276707474292, 21.44615697153889755, 10.87262190629285108 ) ) ;
#20838 = ORIENTED_EDGE ( 'NONE', *, *, #1445, .F. ) ;
#20840 = CARTESIAN_POINT ( 'NONE',  ( -4.440836655099179353, 34.39106106163288246, 13.00000000000000178 ) ) ;
#20839 = CARTESIAN_POINT ( 'NONE',  ( -12.59192885307270160, 21.14500111850274777, -18.43868266935661637 ) ) ;
#20841 = ADVANCED_FACE ( 'NONE', ( #3825 ), #36746, .T. ) ;
#20842 = CARTESIAN_POINT ( 'NONE',  ( -14.64184591927359058, -25.46469159694181172, -10.65210004618737472 ) ) ;
#20843 = DIRECTION ( 'NONE',  ( 1.000000000000000000, 0.000000000000000000, 0.000000000000000000 ) ) ;
#20844 = EDGE_CURVE ( 'NONE', #26114, #7930, #22308, .T. ) ;
#20845 = CIRCLE ( 'NONE', #23410, 1.000000000000002665 ) ;
#20846 = CARTESIAN_POINT ( 'NONE',  ( -30.88206088769906188, -17.38511845617157547, -11.06633628945596826 ) ) ;
#20847 = CARTESIAN_POINT ( 'NONE',  ( -6.708033934598859993, -24.40127542935700333, -10.82077489312179708 ) ) ;
#20848 = DIRECTION ( 'NONE',  ( 1.000000000000000000, 0.000000000000000000, 0.000000000000000000 ) ) ;
#20849 = CARTESIAN_POINT ( 'NONE',  ( 12.15869668810743853, 16.64054837370678896, -28.13968978295428514 ) ) ;
#20850 = EDGE_LOOP ( 'NONE', ( #10710, #39661, #26128, #38273 ) ) ;
#20851 = CARTESIAN_POINT ( 'NONE',  ( 24.66102986608180103, 7.389241230280822137, -5.479742525773724893 ) ) ;
#20852 = VECTOR ( 'NONE', #6546, 1000.000000000000000 ) ;
#20853 = CARTESIAN_POINT ( 'NONE',  ( -5.198706521309195416, 29.65540566576573767, 7.000000000000000000 ) ) ;
#20854 = FACE_OUTER_BOUND ( 'NONE', #4690, .T. ) ;
#20855 = CARTESIAN_POINT ( 'NONE',  ( -7.312041872459064784, 25.58773265502866678, 13.00000000000000178 ) ) ;
#20856 = ORIENTED_EDGE ( 'NONE', *, *, #1717, .F. ) ;
#20857 = CARTESIAN_POINT ( 'NONE',  ( -30.88014466036690564, -0.7593947357035598644, -8.724960917509704927 ) ) ;
#20858 = CARTESIAN_POINT ( 'NONE',  ( 20.61252707005384721, 0.8134334096382831447, -28.07566294656438544 ) ) ;
#20859 = DIRECTION ( 'NONE',  ( 0.000000000000000000, 0.000000000000000000, -1.000000000000000000 ) ) ;
#20860 = CARTESIAN_POINT ( 'NONE',  ( 24.40183261524840574, -16.82966968839916433, 20.82122704794079837 ) ) ;
#20861 = AXIS2_PLACEMENT_3D ( 'NONE', #29404, #10720, #13965 ) ;
#20862 = CARTESIAN_POINT ( 'NONE',  ( 31.47283671532267846, -25.12609584734865464, -5.000000000000006217 ) ) ;
#20863 = EDGE_CURVE ( 'NONE', #5593, #12092, #5595, .T. ) ;
#20864 = DIRECTION ( 'NONE',  ( -0.000000000000000000, -0.000000000000000000, -1.000000000000000000 ) ) ;
#20865 = EDGE_CURVE ( 'NONE', #32523, #31286, #34766, .T. ) ;
#20866 = ORIENTED_EDGE ( 'NONE', *, *, #10413, .T. ) ;
#20867 = DIRECTION ( 'NONE',  ( 0.000000000000000000, 0.000000000000000000, 1.000000000000000000 ) ) ;
#20868 = CIRCLE ( 'NONE', #2048, 1.000000000000000000 ) ;
#20869 = DIRECTION ( 'NONE',  ( 0.000000000000000000, 0.000000000000000000, 1.000000000000000000 ) ) ;
#20870 = ORIENTED_EDGE ( 'NONE', *, *, #15975, .F. ) ;
#20871 = CARTESIAN_POINT ( 'NONE',  ( 0.2990765050996653796, 27.93411067714205487, -17.59605008320459874 ) ) ;
#20872 = DIRECTION ( 'NONE',  ( -0.000000000000000000, -0.000000000000000000, -1.000000000000000000 ) ) ;
#20873 = FACE_OUTER_BOUND ( 'NONE', #38253, .T. ) ;
#20874 = DIRECTION ( 'NONE',  ( 0.000000000000000000, 0.000000000000000000, 1.000000000000000000 ) ) ;
#20875 = CARTESIAN_POINT ( 'NONE',  ( -13.32151712420406220, 20.09434385051854122, 10.50000000000000000 ) ) ;
#20876 = LINE ( 'NONE', #26564, #26152 ) ;
#20877 = CYLINDRICAL_SURFACE ( 'NONE', #19704, 0.5000000000000004441 ) ;
#20878 = CARTESIAN_POINT ( 'NONE',  ( 14.20869267691362836, 26.79038709246419714, -10.56660588343595464 ) ) ;
#20879 = CARTESIAN_POINT ( 'NONE',  ( 9.421923923747751672, 10.82814555784876731, 7.455686640544903376 ) ) ;
#20880 = ORIENTED_EDGE ( 'NONE', *, *, #9132, .F. ) ;
#20882 = DIRECTION ( 'NONE',  ( -0.3090169943749450643, 0.9510565162951544194, 0.000000000000000000 ) ) ;
#20881 = CARTESIAN_POINT ( 'NONE',  ( -16.37425825659163792, 12.35560620482834970, -29.42542551771414594 ) ) ;
#20883 = LINE ( 'NONE', #30225, #8853 ) ;
#20884 = AXIS2_PLACEMENT_3D ( 'NONE', #11400, #1861, #39221 ) ;
#20885 = CARTESIAN_POINT ( 'NONE',  ( 9.713596357440627216, -18.43027871082647096, -26.82846153584012683 ) ) ;
#20886 = CARTESIAN_POINT ( 'NONE',  ( 25.38348611796500975, -5.460896781496693109, 20.69868183039781329 ) ) ;
#20887 = CARTESIAN_POINT ( 'NONE',  ( 15.08986029823985930, 26.17666856099242878, -8.765926281638572348 ) ) ;
#20888 = CARTESIAN_POINT ( 'NONE',  ( -14.97191702109866718, 21.44669161452688044, 10.49999999999999822 ) ) ;
#20889 = LINE ( 'NONE', #2792, #600 ) ;
#20890 = CARTESIAN_POINT ( 'NONE',  ( -29.78193569813405261, -23.30844690436251909, -6.284807164236900334 ) ) ;
#20891 = CARTESIAN_POINT ( 'NONE',  ( 1.807847150130388103, -24.69116081338074764, -6.940716909664599754 ) ) ;
#20892 = CARTESIAN_POINT ( 'NONE',  ( 11.21279839779214171, 17.40770563166403306, -27.45855351148847845 ) ) ;
#20893 = CARTESIAN_POINT ( 'NONE',  ( 17.51797765111094307, 10.67563444151121033, -29.42969723541586191 ) ) ;
#20894 = CARTESIAN_POINT ( 'NONE',  ( 9.427394962683440127, 11.06314620782477753, 10.49999999999999822 ) ) ;
#20895 = EDGE_CURVE ( 'NONE', #23748, #33425, #15974, .T. ) ;
#20896 = CARTESIAN_POINT ( 'NONE',  ( -4.855647265510516064, 23.93711347774053522, -20.81528965570410250 ) ) ;
#20897 = EDGE_LOOP ( 'NONE', ( #4649, #30539, #14530, #5485 ) ) ;
#20898 = CARTESIAN_POINT ( 'NONE',  ( -5.953812613386785912, 14.77701242934787906, 12.00000000000000000 ) ) ;
#20899 = ORIENTED_EDGE ( 'NONE', *, *, #23335, .T. ) ;
#20900 = FACE_OUTER_BOUND ( 'NONE', #23950, .T. ) ;
#20901 = CARTESIAN_POINT ( 'NONE',  ( 9.359089477944728230, 11.31962006718884162, 10.49999999999999822 ) ) ;
#20902 = CARTESIAN_POINT ( 'NONE',  ( -29.17550845323054887, 0.2804399698490122605, -10.65921175933714515 ) ) ;
#20903 = CARTESIAN_POINT ( 'NONE',  ( 24.07628088510988462, -8.068220623474307018, -19.75074122426856604 ) ) ;
#20904 = VERTEX_POINT ( 'NONE', #9532 ) ;
#20905 = CIRCLE ( 'NONE', #3378, 0.5000000000000024425 ) ;
#20906 = CARTESIAN_POINT ( 'NONE',  ( 10.24940219216491677, 33.45281357907897046, 7.102637441331450141 ) ) ;
#20907 = EDGE_LOOP ( 'NONE', ( #15207, #10175 ) ) ;
#20908 = CARTESIAN_POINT ( 'NONE',  ( -8.007761790012255076, 9.776959832083379709, 10.50000000000000711 ) ) ;
#20909 = CARTESIAN_POINT ( 'NONE',  ( 6.811226782241714517, 35.33967249274190436, 10.49999999999999822 ) ) ;
#20910 = AXIS2_PLACEMENT_3D ( 'NONE', #3734, #38471, #28719 ) ;
#20911 = CARTESIAN_POINT ( 'NONE',  ( -4.003810537522578983, 8.420815593655365916, 10.49999999999999822 ) ) ;
#20912 = ORIENTED_EDGE ( 'NONE', *, *, #12408, .T. ) ;
#20913 = CARTESIAN_POINT ( 'NONE',  ( -5.644276917315534270, 36.40655018617698602, 10.63089969389957190 ) ) ;
#20914 = DIRECTION ( 'NONE',  ( 1.224646799147351235E-16, -1.000000000000000000, 0.000000000000000000 ) ) ;
#20915 = EDGE_CURVE ( 'NONE', #7288, #32493, #4927, .T. ) ;
#20916 = CARTESIAN_POINT ( 'NONE',  ( -13.37378135583788463, 20.59160479820268108, 9.500000000000000000 ) ) ;
#20917 = CARTESIAN_POINT ( 'NONE',  ( 19.53446308848797841, 15.92845161367016971, -5.964120103321279842 ) ) ;
#20918 = CARTESIAN_POINT ( 'NONE',  ( 11.37375446201378359, 32.31738641217482666, -8.978749375577956826 ) ) ;
#20919 = VERTEX_POINT ( 'NONE', #13768 ) ;
#20920 = CARTESIAN_POINT ( 'NONE',  ( -18.99707236034979019, 8.589053938987861514, -25.49571320823188003 ) ) ;
#20921 = CARTESIAN_POINT ( 'NONE',  ( 10.81260707898150386, 32.90853150812154837, 10.63089969389957190 ) ) ;
#20922 = VECTOR ( 'NONE', #16314, 1000.000000000000114 ) ;
#20923 = CARTESIAN_POINT ( 'NONE',  ( -1.082972213713690346, 27.41125570341915463, 23.00000000000000000 ) ) ;
#20924 = CARTESIAN_POINT ( 'NONE',  ( 15.24497472440922863, -25.75736537240847568, -10.15205319649687077 ) ) ;
#20925 = DIRECTION ( 'NONE',  ( 1.000000000000000000, 0.000000000000000000, 0.000000000000000000 ) ) ;
#20926 = CARTESIAN_POINT ( 'NONE',  ( 30.41237130417911771, 3.314011747244131723, -13.58461195433497437 ) ) ;
#20927 = CARTESIAN_POINT ( 'NONE',  ( -15.22675634102432873, 26.42529409424080455, -7.827145395733679401 ) ) ;
#20928 = CARTESIAN_POINT ( 'NONE',  ( -13.12770624849639844, -15.75833046460326692, -29.27147291310542698 ) ) ;
#20929 = CARTESIAN_POINT ( 'NONE',  ( 13.49652603687809815, -25.99346187903743299, -7.838242035372235073 ) ) ;
#20930 = EDGE_CURVE ( 'NONE', #1258, #29599, #38961, .T. ) ;
#20931 = VECTOR ( 'NONE', #209, 1000.000000000000114 ) ;
#20932 = CARTESIAN_POINT ( 'NONE',  ( 11.11016527260166242, 31.83082137946473367, 10.99999999999999645 ) ) ;
#20933 = ORIENTED_EDGE ( 'NONE', *, *, #10569, .F. ) ;
#20934 = ORIENTED_EDGE ( 'NONE', *, *, #1413, .F. ) ;
#20935 = CARTESIAN_POINT ( 'NONE',  ( -11.63680257515883554, 32.30205350153836008, -8.540093277045761155 ) ) ;
#20936 = CARTESIAN_POINT ( 'NONE',  ( -12.80736835487442349, 15.68301270189233954, 9.500000000000000000 ) ) ;
#20937 = CARTESIAN_POINT ( 'NONE',  ( 10.36702044712426840, 31.16169077310587809, 10.50000000000000000 ) ) ;
#20938 = AXIS2_PLACEMENT_3D ( 'NONE', #31526, #7130, #22771 ) ;
#20939 = DIRECTION ( 'NONE',  ( -0.000000000000000000, -0.000000000000000000, -1.000000000000000000 ) ) ;
#20940 = ORIENTED_EDGE ( 'NONE', *, *, #8002, .T. ) ;
#20941 = CARTESIAN_POINT ( 'NONE',  ( 30.10059063360280263, 0.1020349076090372453, -8.768825504575827878 ) ) ;
#20942 = ADVANCED_FACE ( 'NONE', ( #7677 ), #15846, .T. ) ;
#20943 = DIRECTION ( 'NONE',  ( -0.9945218953682730678, 0.1045284632676569819, -0.000000000000000000 ) ) ;
#20944 = CARTESIAN_POINT ( 'NONE',  ( -2.575189371470781197, 7.979819372998155913, 10.94387467463494090 ) ) ;
#20945 = EDGE_CURVE ( 'NONE', #40046, #7967, #37379, .T. ) ;
#20946 = ORIENTED_EDGE ( 'NONE', *, *, #24265, .F. ) ;
#20947 = CARTESIAN_POINT ( 'NONE',  ( -21.27402184835637300, 0.7928451952627717514, -25.01640619516613384 ) ) ;
#20948 = DIRECTION ( 'NONE',  ( 1.000000000000000000, 0.000000000000000000, 0.000000000000000000 ) ) ;
#20949 = VERTEX_POINT ( 'NONE', #36120 ) ;
#20950 = CARTESIAN_POINT ( 'NONE',  ( 20.38971234282849565, -2.225416161360934897, -29.29214770260603373 ) ) ;
#20951 = CARTESIAN_POINT ( 'NONE',  ( 36.96658581397633014, -12.84323481469944994, 13.92931973827817238 ) ) ;
#20952 = ORIENTED_EDGE ( 'NONE', *, *, #992, .F. ) ;
#20953 = CARTESIAN_POINT ( 'NONE',  ( -8.901509289504682343, 37.28103075694416901, 14.53008259253942924 ) ) ;
#20954 = DIRECTION ( 'NONE',  ( -1.000000000000000000, 0.000000000000000000, 0.000000000000000000 ) ) ;
#20955 = CARTESIAN_POINT ( 'NONE',  ( 15.00000000000000000, 22.50000000000000711, 7.000000000000000000 ) ) ;
#20956 = CARTESIAN_POINT ( 'NONE',  ( -2.148627388802350158, 32.24135036777339991, 20.25080042701565475 ) ) ;
#20957 = AXIS2_PLACEMENT_3D ( 'NONE', #14315, #24063, #39698 ) ;
#20958 = CARTESIAN_POINT ( 'NONE',  ( -12.39464589777671044, 26.66807349098043289, 13.00000000000000178 ) ) ;
#20959 = VERTEX_POINT ( 'NONE', #14174 ) ;
#20960 = DIRECTION ( 'NONE',  ( 0.000000000000000000, 0.000000000000000000, 1.000000000000000000 ) ) ;
#20961 = EDGE_CURVE ( 'NONE', #17675, #36412, #13974, .T. ) ;
#20962 = VECTOR ( 'NONE', #28048, 1000.000000000000000 ) ;
#20963 = DIRECTION ( 'NONE',  ( 0.1045284632676570929, 0.9945218953682729568, 0.000000000000000000 ) ) ;
#20964 = EDGE_CURVE ( 'NONE', #12988, #22962, #23747, .T. ) ;
#20965 = CARTESIAN_POINT ( 'NONE',  ( 4.836963073857364570, 24.95738821058018075, -19.74021435415385639 ) ) ;
#20966 = AXIS2_PLACEMENT_3D ( 'NONE', #19905, #17476, #32509 ) ;
#20967 = DIRECTION ( 'NONE',  ( 1.000000000000000000, 0.000000000000000000, 0.000000000000000000 ) ) ;
#20968 = CARTESIAN_POINT ( 'NONE',  ( 16.32868373051637079, 2.489249428701628464, 20.94377226548377280 ) ) ;
#20969 = CARTESIAN_POINT ( 'NONE',  ( 18.49299501565283776, -27.00900116835392950, -7.282676274710347286 ) ) ;
#20970 = CARTESIAN_POINT ( 'NONE',  ( 3.900486991066248077, 40.17991855518007327, 11.00000000000019718 ) ) ;
#20971 = LINE ( 'NONE', #15069, #6632 ) ;
#20972 = CARTESIAN_POINT ( 'NONE',  ( -5.706342468480190000, 20.64589803375067945, 13.00000000000000178 ) ) ;
#20973 = VERTEX_POINT ( 'NONE', #17241 ) ;
#20974 = AXIS2_PLACEMENT_3D ( 'NONE', #27558, #19011, #11924 ) ;
#20975 = CARTESIAN_POINT ( 'NONE',  ( 15.37925838865456996, 26.91354363167639363, -5.000000000000000000 ) ) ;
#20976 = ORIENTED_EDGE ( 'NONE', *, *, #18839, .T. ) ;
#20977 = CARTESIAN_POINT ( 'NONE',  ( -11.43474607271607724, 17.01453699462772207, -29.99999999999999645 ) ) ;
#20978 = CARTESIAN_POINT ( 'NONE',  ( -17.59613548593113208, -24.21943298483451201, 18.87996532025787033 ) ) ;
#20979 = CARTESIAN_POINT ( 'NONE',  ( -3.998603647808162798, 8.333314792924266357, 10.49999999999999822 ) ) ;
#20980 = CARTESIAN_POINT ( 'NONE',  ( 12.47124741220967969, 20.38495263699950044, -19.51041991144671428 ) ) ;
#20981 = VERTEX_POINT ( 'NONE', #5032 ) ;
#20982 = CARTESIAN_POINT ( 'NONE',  ( 27.40575770944601075, -17.37578260266968044, -13.80665597063403460 ) ) ;
#20983 = EDGE_LOOP ( 'NONE', ( #25133, #36689 ) ) ;
#20985 = CARTESIAN_POINT ( 'NONE',  ( 7.293999462566144842, 11.53598992149257008, 13.00000000000000178 ) ) ;
#20984 = CARTESIAN_POINT ( 'NONE',  ( -14.84116226840152564, 28.49513596198176657, -5.928569375116603091 ) ) ;
#20986 = CARTESIAN_POINT ( 'NONE',  ( -16.19293341369543171, -24.29526116618816189, -13.31600924498339822 ) ) ;
#20987 = ADVANCED_FACE ( 'NONE', ( #4832 ), #26765, .T. ) ;
#20988 = LINE ( 'NONE', #9190, #25081 ) ;
#20989 = AXIS2_PLACEMENT_3D ( 'NONE', #32051, #773, #31258 ) ;
#20990 = ORIENTED_EDGE ( 'NONE', *, *, #10758, .F. ) ;
#20991 = CARTESIAN_POINT ( 'NONE',  ( -19.95518743367748726, -6.895742946619512814, -26.33169168298753604 ) ) ;
#20992 = CARTESIAN_POINT ( 'NONE',  ( -14.64167027567601487, -25.91586225274019029, -9.242477963831079890 ) ) ;
#20993 = CARTESIAN_POINT ( 'NONE',  ( 24.37759566069541250, -10.08322588119074936, 23.00000000000000000 ) ) ;
#20994 = ORIENTED_EDGE ( 'NONE', *, *, #35569, .F. ) ;
#20995 = CARTESIAN_POINT ( 'NONE',  ( 20.26233914688108229, 3.111977874782128062, -30.00000000000000000 ) ) ;
#20996 = DIRECTION ( 'NONE',  ( -0.9510565162951503115, 0.3090169943749573322, 0.000000000000000000 ) ) ;
#20997 = COLOUR_RGB ( '', 0.31764706, 0.68627451, 0.89019608) ;
#20998 = CARTESIAN_POINT ( 'NONE',  ( -29.22254794994711702, -28.85350742528316204, 11.00000000000000000 ) ) ;
#20999 = EDGE_LOOP ( 'NONE', ( #27074, #12032 ) ) ;
#21000 = CARTESIAN_POINT ( 'NONE',  ( -24.59124188716270609, 0.3669073574842401930, -18.44339233438290293 ) ) ;
#21001 = ORIENTED_EDGE ( 'NONE', *, *, #15553, .F. ) ;
#21002 = CARTESIAN_POINT ( 'NONE',  ( 32.12080372859628596, -1.419867088699604984, -5.466234668651527073 ) ) ;
#21003 = AXIS2_PLACEMENT_3D ( 'NONE', #32659, #1167, #13954 ) ;
#21004 = CARTESIAN_POINT ( 'NONE',  ( 31.65150718622346915, -20.14649908112952303, 17.42190598798391932 ) ) ;
#21005 = EDGE_LOOP ( 'NONE', ( #30803, #18885 ) ) ;
#21006 = CARTESIAN_POINT ( 'NONE',  ( -27.98824911009742422, 2.633740639151773255, -8.327080751032047701 ) ) ;
#21007 = CARTESIAN_POINT ( 'NONE',  ( 11.11016527260166420, 31.83082137946473367, 7.000000000000000000 ) ) ;
#21008 = CARTESIAN_POINT ( 'NONE',  ( -9.806982162272253944, 13.84996144622306247, 6.000000000000000000 ) ) ;
#21009 = CIRCLE ( 'NONE', #34632, 17.99999999999990052 ) ;
#21010 = CARTESIAN_POINT ( 'NONE',  ( -16.05557028316514945, -24.54483004364972132, 18.42518152272108978 ) ) ;
#21011 = CARTESIAN_POINT ( 'NONE',  ( 8.293999462566144842, 11.53598992149257008, 12.00000000000000000 ) ) ;
#21012 = EDGE_CURVE ( 'NONE', #23396, #8563, #26545, .T. ) ;
#21013 = AXIS2_PLACEMENT_3D ( 'NONE', #8274, #8069, #7669 ) ;
#21014 = FACE_BOUND ( 'NONE', #8743, .T. ) ;
#21015 = DIRECTION ( 'NONE',  ( -0.8090169943749430104, 0.5877852522924791323, 0.000000000000000000 ) ) ;
#21016 = ORIENTED_EDGE ( 'NONE', *, *, #39040, .F. ) ;
#21017 = CARTESIAN_POINT ( 'NONE',  ( -25.42975317007962488, 6.206975593436134808, -6.919413500419955732 ) ) ;
#21018 = CARTESIAN_POINT ( 'NONE',  ( 15.41558956984165363, 26.78481017248027740, 0.000000000000000000 ) ) ;
#21019 = CARTESIAN_POINT ( 'NONE',  ( -0.2655091840902661926, 8.754836972118123839, 13.00000000000000178 ) ) ;
#21020 = CARTESIAN_POINT ( 'NONE',  ( 26.28907122124725149, -25.68141371849936405, -5.873759093919935559 ) ) ;
#21021 = DIRECTION ( 'NONE',  ( 1.000000000000000000, 0.000000000000000000, 0.000000000000000000 ) ) ;
#21022 = CARTESIAN_POINT ( 'NONE',  ( 14.86242357273094683, 26.45546649154326246, -9.214439520639988501 ) ) ;
#21023 = CARTESIAN_POINT ( 'NONE',  ( 4.234589283516844012E-14, -26.22849730612247754, 13.92931973827808712 ) ) ;
#21024 = ORIENTED_EDGE ( 'NONE', *, *, #39842, .F. ) ;
#21025 = VECTOR ( 'NONE', #12699, 1000.000000000000000 ) ;
#21026 = CARTESIAN_POINT ( 'NONE',  ( -16.27617705945219839, 20.65743945337694853, -11.73023920987073510 ) ) ;
#21027 = CARTESIAN_POINT ( 'NONE',  ( -26.04175756481620496, -10.41789154269907058, 20.94377226548378346 ) ) ;
#21028 = CARTESIAN_POINT ( 'NONE',  ( 0.5000000000000002220, 36.50000000000000711, 9.500000000000000000 ) ) ;
#21029 = CARTESIAN_POINT ( 'NONE',  ( 14.04032970691909732, 23.91029121590017681, -13.51430497135585895 ) ) ;
#21030 = ORIENTED_EDGE ( 'NONE', *, *, #35387, .T. ) ;
#21031 = CARTESIAN_POINT ( 'NONE',  ( -14.61656768153253694, 21.96308928146571660, 10.49999999999999822 ) ) ;
#21032 = EDGE_LOOP ( 'NONE', ( #3882, #37315 ) ) ;
#21034 = DIRECTION ( 'NONE',  ( 1.000000000000000000, 0.000000000000000000, 0.000000000000000000 ) ) ;
#21033 = CARTESIAN_POINT ( 'NONE',  ( -15.35513899590904430, 26.99708482749830907, -5.473155708056963498 ) ) ;
#21035 = CARTESIAN_POINT ( 'NONE',  ( -9.836635315125095147, -18.54107557745045654, -26.21993274389535244 ) ) ;
#21036 = ADVANCED_FACE ( 'NONE', ( #23325 ), #608, .T. ) ;
#21037 = CARTESIAN_POINT ( 'NONE',  ( 1.000000000000000000, 37.50000000000000711, 10.49999999999999822 ) ) ;
#21038 = CARTESIAN_POINT ( 'NONE',  ( -17.55945971783640758, -10.59693620792911872, -30.00000000000001421 ) ) ;
#21039 = CARTESIAN_POINT ( 'NONE',  ( -9.876522206958991745, -22.96841405707892037, -15.64990654850994822 ) ) ;
#21040 = CARTESIAN_POINT ( 'NONE',  ( -19.30730118283921470, -16.27608008926401340, 21.00000000000001421 ) ) ;
#21041 = CARTESIAN_POINT ( 'NONE',  ( 12.18916105282683304, 16.70401724222313788, -27.52870704815159186 ) ) ;
#21043 = EDGE_CURVE ( 'NONE', #24994, #14246, #2987, .T. ) ;
#21042 = VERTEX_POINT ( 'NONE', #24322 ) ;
#21044 = CARTESIAN_POINT ( 'NONE',  ( 20.57897257680733460, 5.989271796650077029, -23.20797897217266126 ) ) ;
#21045 = CARTESIAN_POINT ( 'NONE',  ( 9.665073660139013256, 25.11464168560187460, 10.50000000000000533 ) ) ;
#21046 = DIRECTION ( 'NONE',  ( 0.000000000000000000, 0.000000000000000000, 1.000000000000000000 ) ) ;
#21047 = DIRECTION ( 'NONE',  ( 0.000000000000000000, 0.000000000000000000, -1.000000000000000000 ) ) ;
#21048 = ORIENTED_EDGE ( 'NONE', *, *, #2137, .T. ) ;
#21049 = CARTESIAN_POINT ( 'NONE',  ( -21.42004826045867816, -0.5745119313267001981, -24.86738022874436638 ) ) ;
#21050 = CIRCLE ( 'NONE', #24294, 1.000000000000000888 ) ;
#21051 = CARTESIAN_POINT ( 'NONE',  ( 20.69644567353984499, 0.8041823441500935976, -27.44559075125846093 ) ) ;
#21052 = EDGE_CURVE ( 'NONE', #18778, #25278, #2593, .T. ) ;
#21053 = PLANE ( 'NONE',  #9214 ) ;
#21054 = CARTESIAN_POINT ( 'NONE',  ( 25.74508523780477987, -9.012467239717258494, 20.94377226548369819 ) ) ;
#21055 = DIRECTION ( 'NONE',  ( 1.000000000000000000, 0.000000000000000000, 0.000000000000000000 ) ) ;
#21056 = CARTESIAN_POINT ( 'NONE',  ( 32.84658669524301189, -23.46788009898371641, 10.99999999999997335 ) ) ;
#21057 = VECTOR ( 'NONE', #13498, 1000.000000000000000 ) ;
#21058 = ORIENTED_EDGE ( 'NONE', *, *, #23443, .F. ) ;
#21059 = EDGE_CURVE ( 'NONE', #38584, #19377, #21078, .T. ) ;
#21060 = LINE ( 'NONE', #2576, #12608 ) ;
#21061 = EDGE_CURVE ( 'NONE', #26362, #11564, #5437, .T. ) ;
#21062 = EDGE_CURVE ( 'NONE', #8150, #15766, #9083, .T. ) ;
#21063 = DIRECTION ( 'NONE',  ( 0.2876062384759507928, 0.6459741880212497289, -0.7071067811865487940 ) ) ;
#21064 = VERTEX_POINT ( 'NONE', #39952 ) ;
#21065 = CARTESIAN_POINT ( 'NONE',  ( 1.544216759713194165, 37.43288271813057833, -8.405430002237888942 ) ) ;
#21066 = CARTESIAN_POINT ( 'NONE',  ( -4.724378136954611840, 12.76962061027129458, 12.00000000000000000 ) ) ;
#21067 = CARTESIAN_POINT ( 'NONE',  ( 19.73557158514996246, 33.31698729810761250, 11.00000000000000000 ) ) ;
#21068 = DIRECTION ( 'NONE',  ( 0.000000000000000000, 0.000000000000000000, 1.000000000000000000 ) ) ;
#21069 = CARTESIAN_POINT ( 'NONE',  ( 14.52509594610761923, 21.97885917798724975, 10.50000000000000355 ) ) ;
#21070 = DIRECTION ( 'NONE',  ( 0.000000000000000000, 0.000000000000000000, 1.000000000000000000 ) ) ;
#21071 = CARTESIAN_POINT ( 'NONE',  ( 14.22382948751891441, 26.07014013211499659, 10.49999999999999822 ) ) ;
#21072 = AXIS2_PLACEMENT_3D ( 'NONE', #33920, #36765, #24168 ) ;
#21073 = CARTESIAN_POINT ( 'NONE',  ( 9.553997640115609258, 18.14112040201965925, -29.99999999999999645 ) ) ;
#21074 = CARTESIAN_POINT ( 'NONE',  ( 2.494936919103933448, 34.23777120880591696, 12.00000000000000000 ) ) ;
#21075 = VERTEX_POINT ( 'NONE', #5627 ) ;
#21077 = DIRECTION ( 'NONE',  ( -0.2079116908177663647, -0.9781476007338042455, 0.000000000000000000 ) ) ;
#21076 = CARTESIAN_POINT ( 'NONE',  ( -18.56352605694899083, 15.93433109089512101, -11.84711699134787111 ) ) ;
#21078 = LINE ( 'NONE', #24119, #7526 ) ;
#21079 = CARTESIAN_POINT ( 'NONE',  ( 10.53369465903642244, -19.57651849404395961, -22.73532858526640510 ) ) ;
#21080 = CARTESIAN_POINT ( 'NONE',  ( 32.33143948541787438, 1.358872982501792226, 11.00000000000000000 ) ) ;
#21081 = CARTESIAN_POINT ( 'NONE',  ( 11.16181463136529040, 17.77262720094327975, -26.22243848669149813 ) ) ;
#21082 = ORIENTED_EDGE ( 'NONE', *, *, #10390, .T. ) ;
#21083 = CARTESIAN_POINT ( 'NONE',  ( 15.29245034862073460, 32.56469986092002955, -13.99876745781544685 ) ) ;
#21084 = DIRECTION ( 'NONE',  ( 0.000000000000000000, 0.000000000000000000, 1.000000000000000000 ) ) ;
#21085 = EDGE_CURVE ( 'NONE', #6918, #36141, #15374, .T. ) ;
#21086 = AXIS2_PLACEMENT_3D ( 'NONE', #4622, #17020, #22695 ) ;
#21087 = CARTESIAN_POINT ( 'NONE',  ( -28.62642820236494501, -22.44600169765076814, -9.303848538514403188 ) ) ;
#21088 = CARTESIAN_POINT ( 'NONE',  ( -2.525287455661448632, -24.41780038572089850, -9.392889257882757192 ) ) ;
#21089 = CARTESIAN_POINT ( 'NONE',  ( 12.15359677241966629, 19.10405381618496889, -21.66180759330809380 ) ) ;
#21090 = EDGE_CURVE ( 'NONE', #26812, #24016, #39754, .T. ) ;
#21091 = CARTESIAN_POINT ( 'NONE',  ( 17.94274596522729937, 10.05102289979594232, -28.30046506151757768 ) ) ;
#21092 = DIRECTION ( 'NONE',  ( 1.000000000000000000, 0.000000000000000000, 0.000000000000000000 ) ) ;
#21093 = CARTESIAN_POINT ( 'NONE',  ( -4.680396452074460534, 32.75778677526109561, -12.91952194480230176 ) ) ;
#21094 = VERTEX_POINT ( 'NONE', #5833 ) ;
#21095 = CARTESIAN_POINT ( 'NONE',  ( -20.48347041321339290, 17.67745015982535861, 12.73282698324691609 ) ) ;
#21096 = ORIENTED_EDGE ( 'NONE', *, *, #4707, .T. ) ;
#21097 = DIRECTION ( 'NONE',  ( -0.9781476007338069101, -0.2079116908177532363, 0.000000000000000000 ) ) ;
#21098 = CARTESIAN_POINT ( 'NONE',  ( -9.788946493797832105, 21.72623886970244911, 13.00000000000000178 ) ) ;
#21099 = CARTESIAN_POINT ( 'NONE',  ( -30.36706297773999097, 0.4086613843392599699, -6.417692154602818277 ) ) ;
#21100 = CARTESIAN_POINT ( 'NONE',  ( 31.93250169833669716, -9.587213356856551627, -12.05150297994976327 ) ) ;
#21101 = CIRCLE ( 'NONE', #39909, 1.000000000000000888 ) ;
#21102 = ORIENTED_EDGE ( 'NONE', *, *, #16751, .T. ) ;
#21103 = CONTEXT_DEPENDENT_SHAPE_REPRESENTATION ( #12447, #26248 ) ;
#21104 = CARTESIAN_POINT ( 'NONE',  ( 10.16122020288883299, 33.53402030034401804, 7.000000000000000000 ) ) ;
#21105 = ORIENTED_EDGE ( 'NONE', *, *, #29866, .F. ) ;
#21106 = CARTESIAN_POINT ( 'NONE',  ( -3.503793317224518145, 8.420815634768723967, 7.000000000000000000 ) ) ;
#21107 = AXIS2_PLACEMENT_3D ( 'NONE', #32630, #38712, #23273 ) ;
#21108 = DIRECTION ( 'NONE',  ( 1.000000000000000000, 0.000000000000000000, 0.000000000000000000 ) ) ;
#21109 = CONICAL_SURFACE ( 'NONE', #10085, 1.000000000000002665, 0.7853981633974548293 ) ;
#21110 = VECTOR ( 'NONE', #15237, 1000.000000000000000 ) ;
#21111 = CARTESIAN_POINT ( 'NONE',  ( -3.718716484603639572, 7.955328666817546690, 10.49999999999999645 ) ) ;
#21112 = ORIENTED_EDGE ( 'NONE', *, *, #9858, .T. ) ;
#21113 = CYLINDRICAL_SURFACE ( 'NONE', #15886, 1.000000000000000888 ) ;
#21114 = CARTESIAN_POINT ( 'NONE',  ( 3.357189294653307954, 32.49896394832310165, 10.49999999999999645 ) ) ;
#21115 = DIRECTION ( 'NONE',  ( 1.000000000000000000, 0.000000000000000000, 0.000000000000000000 ) ) ;
#21116 = CARTESIAN_POINT ( 'NONE',  ( 29.26826387686844910, -23.91120845623157010, -5.438285388144263877 ) ) ;
#21117 = CARTESIAN_POINT ( 'NONE',  ( 19.95486563595593310, 14.86767224104078977, -7.423818949657161603 ) ) ;
#21118 = CARTESIAN_POINT ( 'NONE',  ( 12.41906572600498926, 32.58765353250298347, -4.999999999999998224 ) ) ;
#21119 = ORIENTED_EDGE ( 'NONE', *, *, #28494, .T. ) ;
#21120 = CARTESIAN_POINT ( 'NONE',  ( -21.60396578388440858, 10.50237655917392310, -11.87878979233392762 ) ) ;
#21121 = CARTESIAN_POINT ( 'NONE',  ( -8.577547685840080760, 11.84256962714647798, 12.00000000000000000 ) ) ;
#21122 = DIRECTION ( 'NONE',  ( -0.5877852522924797984, -0.8090169943749426773, 0.000000000000000000 ) ) ;
#21123 = CARTESIAN_POINT ( 'NONE',  ( 9.902073939236615274, -18.51143114917217503, -26.21360673141550635 ) ) ;
#21124 = DIRECTION ( 'NONE',  ( 0.000000000000000000, 0.000000000000000000, 1.000000000000000000 ) ) ;
#21125 = CARTESIAN_POINT ( 'NONE',  ( 16.24796006241085422, 15.88921519459651144, -30.00000000000001421 ) ) ;
#21126 = CARTESIAN_POINT ( 'NONE',  ( -12.91698160810270934, 21.67206672448811133, -17.43500531611570636 ) ) ;
#21127 = CARTESIAN_POINT ( 'NONE',  ( -24.70057832354312666, -26.06393885949841760, -7.180590994032729490 ) ) ;
#21128 = CARTESIAN_POINT ( 'NONE',  ( 13.69821889811312410, -26.30560278297641830, -5.474065301971783981 ) ) ;
#21129 = CARTESIAN_POINT ( 'NONE',  ( 4.082600654608392610, 21.41965916404854298, 12.00000000000000000 ) ) ;
#21130 = VERTEX_POINT ( 'NONE', #6227 ) ;
#21131 = ORIENTED_EDGE ( 'NONE', *, *, #37609, .F. ) ;
#21132 = CARTESIAN_POINT ( 'NONE',  ( -6.249731466780908740, 20.89879465126994518, -24.45472809205353926 ) ) ;
#21133 = CIRCLE ( 'NONE', #34130, 1.000000000000000000 ) ;
#21134 = DIRECTION ( 'NONE',  ( 1.000000000000000000, 0.000000000000000000, 0.000000000000000000 ) ) ;
#21135 = CARTESIAN_POINT ( 'NONE',  ( 12.80736835487433289, 15.68301270189216545, 7.499999999999997335 ) ) ;
#21136 = VECTOR ( 'NONE', #4568, 999.9999999999998863 ) ;
#21137 = AXIS2_PLACEMENT_3D ( 'NONE', #2598, #36124, #33087 ) ;
#21138 = CARTESIAN_POINT ( 'NONE',  ( -12.99377146717201192, 26.19620116591435277, 10.00000000000000000 ) ) ;
#21139 = ORIENTED_EDGE ( 'NONE', *, *, #2616, .F. ) ;
#21140 = CARTESIAN_POINT ( 'NONE',  ( 30.28856303283004081, 0.06353136651604823770, -8.298345987469021523 ) ) ;
#21141 = CARTESIAN_POINT ( 'NONE',  ( -37.48557158514985588, -11.24999999999982414, 3.000000000000000000 ) ) ;
#21142 = CARTESIAN_POINT ( 'NONE',  ( -2.596139932171949383, 7.881254734312912902, 10.87262190629277292 ) ) ;
#21143 = VERTEX_POINT ( 'NONE', #31019 ) ;
#21144 = CARTESIAN_POINT ( 'NONE',  ( -29.35000585794652395, 0.07926546081450050463, -10.65361827406238149 ) ) ;
#21145 = CYLINDRICAL_SURFACE ( 'NONE', #39743, 0.5000000000000004441 ) ;
#21146 = VERTEX_POINT ( 'NONE', #37113 ) ;
#21147 = CARTESIAN_POINT ( 'NONE',  ( 21.47608197099559391, -2.388604051638352654, -24.67957022850504956 ) ) ;
#21148 = CARTESIAN_POINT ( 'NONE',  ( 33.43067318719201353, -0.2406684815405015221, 13.32518128616727537 ) ) ;
#21149 = ORIENTED_EDGE ( 'NONE', *, *, #5808, .T. ) ;
#21150 = CARTESIAN_POINT ( 'NONE',  ( 5.571153519068981375, 39.03845596069754009, 13.92931973827808889 ) ) ;
#21151 = CARTESIAN_POINT ( 'NONE',  ( 4.309332716386178631E-14, -16.21345324574345170, 20.82122704794080192 ) ) ;
#21152 = CYLINDRICAL_SURFACE ( 'NONE', #28628, 1.000000000000000000 ) ;
#21153 = CARTESIAN_POINT ( 'NONE',  ( 3.166027244385917427, 31.89862848374664495, 20.25080042701565830 ) ) ;
#21154 = CARTESIAN_POINT ( 'NONE',  ( 5.082600654608392610, 21.41965916404854298, 13.00000000000000178 ) ) ;
#21155 = ORIENTED_EDGE ( 'NONE', *, *, #40024, .F. ) ;
#21156 = EDGE_CURVE ( 'NONE', #31697, #8563, #25295, .T. ) ;
#21157 = CARTESIAN_POINT ( 'NONE',  ( 10.72501808743029095, 33.00580893829960161, 10.49999999999999822 ) ) ;
#21158 = DIRECTION ( 'NONE',  ( 0.000000000000000000, 0.000000000000000000, -1.000000000000000000 ) ) ;
#21159 = VECTOR ( 'NONE', #17699, 1000.000000000000227 ) ;
#21160 = CARTESIAN_POINT ( 'NONE',  ( 8.119369784788442956, 36.07111323917224865, -6.725600398549506309 ) ) ;
#21161 = CIRCLE ( 'NONE', #20534, 1.000000000000000888 ) ;
#21162 = FACE_OUTER_BOUND ( 'NONE', #37093, .T. ) ;
#21163 = EDGE_CURVE ( 'NONE', #21833, #12134, #40152, .T. ) ;
#21164 = CARTESIAN_POINT ( 'NONE',  ( 17.69280599716815416, 3.437614796730258160, 20.69868183039776710 ) ) ;
#21165 = AXIS2_PLACEMENT_3D ( 'NONE', #27172, #6025, #33286 ) ;
#21166 = EDGE_CURVE ( 'NONE', #15751, #33185, #30250, .T. ) ;
#21167 = CARTESIAN_POINT ( 'NONE',  ( 12.46065444517352283, -16.66684880058570073, -27.23723484178347221 ) ) ;
#21168 = CARTESIAN_POINT ( 'NONE',  ( 8.843266739736572291, 16.81698729810774395, 10.50000000000000000 ) ) ;
#21169 = DIRECTION ( 'NONE',  ( -0.9510565162951504226, 0.3090169943749573322, 0.000000000000000000 ) ) ;
#21170 = LINE ( 'NONE', #2288, #21996 ) ;
#21171 = ORIENTED_EDGE ( 'NONE', *, *, #14892, .F. ) ;
#21172 = CARTESIAN_POINT ( 'NONE',  ( 12.09851136747228217, 19.96279823048476132, -20.53435459044266054 ) ) ;
#21173 = ORIENTED_EDGE ( 'NONE', *, *, #17972, .T. ) ;
#21174 = CARTESIAN_POINT ( 'NONE',  ( -15.42498320908520704, 26.75103934920171511, -5.000000000000002665 ) ) ;
#21175 = CARTESIAN_POINT ( 'NONE',  ( -31.82689352098154600, -6.837796194681720507, 18.87996532025821850 ) ) ;
#21176 = CARTESIAN_POINT ( 'NONE',  ( 9.458291886585664443, -18.18766449894053849, -30.00000000000000000 ) ) ;
#21177 = CARTESIAN_POINT ( 'NONE',  ( 3.963760424820348405, 8.194319839800193961, 10.49999999999999822 ) ) ;
#21178 = CARTESIAN_POINT ( 'NONE',  ( 15.07386490424905467, 25.79242186437713613, -9.240524828524506518 ) ) ;
#21179 = VERTEX_POINT ( 'NONE', #12326 ) ;
#21180 = CARTESIAN_POINT ( 'NONE',  ( 22.16801406757617343, -13.11526815166102544, -19.62611364897102106 ) ) ;
#21181 = VERTEX_POINT ( 'NONE', #9281 ) ;
#21183 = CARTESIAN_POINT ( 'NONE',  ( -6.774334011769939323, 35.84443018111166879, 10.49999999999999467 ) ) ;
#21182 = CARTESIAN_POINT ( 'NONE',  ( -14.80950393188541092, 28.42383370304063916, -6.390113609832926755 ) ) ;
#21184 = CARTESIAN_POINT ( 'NONE',  ( -11.41242022595238126, -17.75887984712721845, -26.06507157920607654 ) ) ;
#21185 = CARTESIAN_POINT ( 'NONE',  ( -13.30736835487441638, 16.54903810567678235, 7.000000000000000000 ) ) ;
#21186 = VERTEX_POINT ( 'NONE', #26972 ) ;
#21187 = CARTESIAN_POINT ( 'NONE',  ( -25.85792922089648371, -9.778323470226343517, -17.66350960614173715 ) ) ;
#21188 = CARTESIAN_POINT ( 'NONE',  ( -15.05356374896470584, -26.34688506717603929, -7.828843382777417759 ) ) ;
#21189 = CARTESIAN_POINT ( 'NONE',  ( 14.52509594610761923, 21.97885917798724975, 7.000000000000000000 ) ) ;
#21190 = VERTEX_POINT ( 'NONE', #23923 ) ;
#21191 = CARTESIAN_POINT ( 'NONE',  ( 28.97456723585821692, 1.148426348366920591, -9.256809715960919505 ) ) ;
#21192 = CARTESIAN_POINT ( 'NONE',  ( 9.197066986886593298, 11.25907462514027202, 10.66666666666666430 ) ) ;
#21193 = EDGE_CURVE ( 'NONE', #30652, #12596, #12720, .T. ) ;
#21194 = CARTESIAN_POINT ( 'NONE',  ( -37.88915195766834643, -19.37406375362053979, 11.00000000000000000 ) ) ;
#21195 = EDGE_CURVE ( 'NONE', #31103, #22349, #1721, .T. ) ;
#21196 = EDGE_LOOP ( 'NONE', ( #5061, #19736, #31440, #30642 ) ) ;
#21197 = CARTESIAN_POINT ( 'NONE',  ( -30.97418125221157226, -0.1138930278413790714, -4.999999999999999112 ) ) ;
#21198 = ORIENTED_EDGE ( 'NONE', *, *, #26662, .T. ) ;
#21199 = CARTESIAN_POINT ( 'NONE',  ( 30.43325519101775356, -1.251503160527801528, -10.55494845371857693 ) ) ;
#21200 = CARTESIAN_POINT ( 'NONE',  ( 17.40362039086722135, -25.54020003774037662, 17.92354375535206756 ) ) ;
#21201 = ORIENTED_EDGE ( 'NONE', *, *, #14822, .T. ) ;
#21202 = CARTESIAN_POINT ( 'NONE',  ( -24.96329531792162726, 3.513752566392065901, -14.68029723533687303 ) ) ;
#21203 = DIRECTION ( 'NONE',  ( -2.168404344971006896E-16, 1.000000000000000000, 0.000000000000000000 ) ) ;
#21204 = CARTESIAN_POINT ( 'NONE',  ( 3.025308588020339862, 26.48089285804714876, 20.99999999999999645 ) ) ;
#21205 = PLANE ( 'NONE',  #38187 ) ;
#21206 = DIRECTION ( 'NONE',  ( 0.4156269377774484686, -0.5720614028176835841, -0.7071067811865511255 ) ) ;
#21207 = EDGE_CURVE ( 'NONE', #12323, #2692, #20883, .T. ) ;
#21208 = FACE_BOUND ( 'NONE', #26422, .T. ) ;
#21209 = DIRECTION ( 'NONE',  ( 0.4731467892558125499, -0.5254827454987578417, -0.7071067811865499042 ) ) ;
#21210 = ORIENTED_EDGE ( 'NONE', *, *, #18987, .F. ) ;
#21211 = CARTESIAN_POINT ( 'NONE',  ( -24.18815070014865398, 8.032309469253892331, -5.962252224280692126 ) ) ;
#21212 = LINE ( 'NONE', #4772, #15101 ) ;
#21213 = CYLINDRICAL_SURFACE ( 'NONE', #20122, 1.000000000000000888 ) ;
#21214 = CARTESIAN_POINT ( 'NONE',  ( 20.14663775004962076, -19.75195631921120665, -16.78371938112692519 ) ) ;
#21215 = DIRECTION ( 'NONE',  ( -1.000000000000000000, 0.000000000000000000, 0.000000000000000000 ) ) ;
#21216 = CARTESIAN_POINT ( 'NONE',  ( 10.89766637450477837, 17.61927834571792317, -27.43414935101323948 ) ) ;
#21217 = VECTOR ( 'NONE', #34328, 1000.000000000000000 ) ;
#21218 = CARTESIAN_POINT ( 'NONE',  ( 5.078902502065831825, -26.44091005802452798, 13.32518128616608877 ) ) ;
#21219 = EDGE_LOOP ( 'NONE', ( #2310, #26884, #8201 ) ) ;
#21221 = CIRCLE ( 'NONE', #25735, 15.00000000000000000 ) ;
#21220 = CARTESIAN_POINT ( 'NONE',  ( -16.92840057844002644, 21.76311522583030822, -6.905117785391271745 ) ) ;
#21222 = CARTESIAN_POINT ( 'NONE',  ( -17.62780868050729666, -18.45076755199299257, 20.82122704794079837 ) ) ;
#21223 = CARTESIAN_POINT ( 'NONE',  ( -6.354454053420243831, 35.54304081427989814, 11.00000000000000000 ) ) ;
#21224 = CARTESIAN_POINT ( 'NONE',  ( 11.00857322187251164, 17.29338995577434446, -29.34887577826749805 ) ) ;
#21225 = EDGE_LOOP ( 'NONE', ( #37347, #32747 ) ) ;
#21226 = CARTESIAN_POINT ( 'NONE',  ( -14.70981814587872094, 21.45668995266216683, 10.94387467463488051 ) ) ;
#21227 = ORIENTED_EDGE ( 'NONE', *, *, #905, .T. ) ;
#21229 = DIRECTION ( 'NONE',  ( 0.6691306063588571273, -0.7431448254773952433, 0.000000000000000000 ) ) ;
#21228 = CARTESIAN_POINT ( 'NONE',  ( -12.32989360994015549, 20.57215784758508548, -19.48341777572011324 ) ) ;
#21230 = CARTESIAN_POINT ( 'NONE',  ( -15.50788136758524693, -26.74767648567673817, -5.474109841062610116 ) ) ;
#21231 = CARTESIAN_POINT ( 'NONE',  ( -3.118678732975735279, 7.827785988993307242, 6.000000000000000000 ) ) ;
#21232 = AXIS2_PLACEMENT_3D ( 'NONE', #5428, #8271, #17433 ) ;
#21233 = CARTESIAN_POINT ( 'NONE',  ( -18.08564274236685776, -10.18792848139066543, -27.70420942370164141 ) ) ;
#21234 = CARTESIAN_POINT ( 'NONE',  ( -7.966395251936380539, -19.90518285585014979, -24.10536815931465426 ) ) ;
#21235 = DIRECTION ( 'NONE',  ( -1.000000000000000000, 0.000000000000000000, 0.000000000000000000 ) ) ;
#21236 = CARTESIAN_POINT ( 'NONE',  ( 12.11158980248019645, 16.54297856518634902, -29.37115136132677762 ) ) ;
#21237 = ORIENTED_EDGE ( 'NONE', *, *, #13340, .T. ) ;
#21238 = CARTESIAN_POINT ( 'NONE',  ( 20.85536741361552160, 6.013920567586717780, -22.11640438643503614 ) ) ;
#21239 = CARTESIAN_POINT ( 'NONE',  ( -5.237540274239744775, 35.49300472853438038, 7.500000000000000888 ) ) ;
#21240 = ADVANCED_FACE ( 'NONE', ( #33486 ), #18435, .T. ) ;
#21241 = DIRECTION ( 'NONE',  ( 0.000000000000000000, 0.000000000000000000, 1.000000000000000000 ) ) ;
#21242 = EDGE_CURVE ( 'NONE', #16160, #21540, #22253, .T. ) ;
#21243 = LINE ( 'NONE', #34236, #11553 ) ;
#21244 = VERTEX_POINT ( 'NONE', #31409 ) ;
#21245 = CARTESIAN_POINT ( 'NONE',  ( -30.25467497739411726, -0.7069905369280371499, -10.12455798544348440 ) ) ;
#21246 = CARTESIAN_POINT ( 'NONE',  ( 30.63389016003661780, -0.1680630686027007048, -7.820899855639765086 ) ) ;
#21247 = CARTESIAN_POINT ( 'NONE',  ( -19.48557158514985588, -11.25000000000002309, 3.000000000000000000 ) ) ;
#21248 = CARTESIAN_POINT ( 'NONE',  ( 22.09885373566428868, -20.02268770624830552, 20.50957957746051719 ) ) ;
#21249 = CARTESIAN_POINT ( 'NONE',  ( 30.41237130417911771, 3.314011747244134387, -4.999999999999999112 ) ) ;
#21250 = CYLINDRICAL_SURFACE ( 'NONE', #13471, 0.5000000000000004441 ) ;
#21251 = AXIS2_PLACEMENT_3D ( 'NONE', #10241, #23032, #14091 ) ;
#21252 = AXIS2_PLACEMENT_3D ( 'NONE', #32487, #16434, #22922 ) ;
#21253 = EDGE_LOOP ( 'NONE', ( #28368, #1149, #22641, #11045 ) ) ;
#21254 = CARTESIAN_POINT ( 'NONE',  ( 14.97837590057439527, 21.69185896976586037, 7.455686640544910482 ) ) ;
#21255 = CIRCLE ( 'NONE', #3725, 0.5000000000000001110 ) ;
#21256 = ADVANCED_FACE ( 'NONE', ( #12525 ), #6610, .F. ) ;
#21257 = AXIS2_PLACEMENT_3D ( 'NONE', #14751, #10698, #4602 ) ;
#21258 = FACE_OUTER_BOUND ( 'NONE', #12679, .T. ) ;
#21259 = CARTESIAN_POINT ( 'NONE',  ( 1.000000000000000666, 33.00000000000000000, 11.00000000000000000 ) ) ;
#21260 = CARTESIAN_POINT ( 'NONE',  ( 3.871220829879935099, 38.02450267464935507, -5.436529868897947537 ) ) ;
#21261 = DIRECTION ( 'NONE',  ( 0.2079116908177533751, -0.9781476007338067991, 0.000000000000000000 ) ) ;
#21262 = CARTESIAN_POINT ( 'NONE',  ( 17.01882136418227986, 27.23043334310844799, 13.32518128616608877 ) ) ;
#21263 = LINE ( 'NONE', #12120, #21997 ) ;
#21264 = LINE ( 'NONE', #32416, #5016 ) ;
#21265 = FACE_OUTER_BOUND ( 'NONE', #3350, .T. ) ;
#21266 = DIRECTION ( 'NONE',  ( 1.000000000000000000, 0.000000000000000000, 0.000000000000000000 ) ) ;
#21267 = CARTESIAN_POINT ( 'NONE',  ( 13.18225496512505757, 24.59173741764900356, -14.35579410304919534 ) ) ;
#21268 = CARTESIAN_POINT ( 'NONE',  ( 9.729305141884044161, 11.08259174741900033, 7.203056206335836542 ) ) ;
#21269 = ORIENTED_EDGE ( 'NONE', *, *, #8283, .T. ) ;
#21271 = CARTESIAN_POINT ( 'NONE',  ( -34.47241746879593904, 3.460351812918829761, 3.000000000000000000 ) ) ;
#21270 = CARTESIAN_POINT ( 'NONE',  ( -16.06070315713033025, 13.11638197811575246, -26.58602791737893156 ) ) ;
#21272 = CARTESIAN_POINT ( 'NONE',  ( 9.356056665764066693, 26.06569820189703179, 10.49999999999999645 ) ) ;
#21273 = CARTESIAN_POINT ( 'NONE',  ( 14.96192828012108578, -25.98634713340315017, -9.238541611499263340 ) ) ;
#21274 = CARTESIAN_POINT ( 'NONE',  ( -20.76418541913865923, -26.08974834292795109, -9.464979353182689792 ) ) ;
#21275 = CARTESIAN_POINT ( 'NONE',  ( 29.28423149095877420, -1.632116715646417138, 18.42518152272108622 ) ) ;
#21276 = CARTESIAN_POINT ( 'NONE',  ( 15.09217338382007689, 26.16895268490867821, -8.766269268417817173 ) ) ;
#21277 = VECTOR ( 'NONE', #34365, 1000.000000000000000 ) ;
#21278 = ORIENTED_EDGE ( 'NONE', *, *, #17215, .F. ) ;
#21279 = PLANE ( 'NONE',  #21137 ) ;
#21280 = CARTESIAN_POINT ( 'NONE',  ( 38.66460482429456391, -17.32098562631985672, 11.00000000000000178 ) ) ;
#21281 = AXIS2_PLACEMENT_3D ( 'NONE', #16247, #19897, #22726 ) ;
#21282 = AXIS2_PLACEMENT_3D ( 'NONE', #17613, #11307, #5800 ) ;
#21283 = CARTESIAN_POINT ( 'NONE',  ( -22.05305370367605278, -18.37986245703921284, -16.69510183025791505 ) ) ;
#21284 = CARTESIAN_POINT ( 'NONE',  ( -0.3897205959626178773, -24.77793770357540737, -5.000000000000000888 ) ) ;
#21285 = CARTESIAN_POINT ( 'NONE',  ( 13.70661370344850560, 22.39768893898365221, -15.48108906342483415 ) ) ;
#21286 = CARTESIAN_POINT ( 'NONE',  ( 22.20551005480023576, 11.09721735243621588, -5.966899065133762114 ) ) ;
#21287 = CARTESIAN_POINT ( 'NONE',  ( 10.80697542085375140, 31.15003855377755571, 13.00000000000000178 ) ) ;
#21288 = CARTESIAN_POINT ( 'NONE',  ( -3.735156488784892481, 26.39161017904735829, -18.66586346394144158 ) ) ;
#21289 = VECTOR ( 'NONE', #18756, 1000.000000000000000 ) ;
#21290 = EDGE_CURVE ( 'NONE', #13694, #3751, #3577, .T. ) ;
#21291 = VERTEX_POINT ( 'NONE', #7010 ) ;
#21292 = CARTESIAN_POINT ( 'NONE',  ( -34.41928798828883629, -5.508411629658334974, -5.895573557013064736 ) ) ;
#21293 = EDGE_CURVE ( 'NONE', #13267, #16446, #32584, .T. ) ;
#21294 = AXIS2_PLACEMENT_3D ( 'NONE', #18892, #3050, #27834 ) ;
#21295 = CARTESIAN_POINT ( 'NONE',  ( -20.16616670141840828, 17.52816929147905967, 13.92931973827678682 ) ) ;
#21296 = ORIENTED_EDGE ( 'NONE', *, *, #31835, .F. ) ;
#21297 = CARTESIAN_POINT ( 'NONE',  ( 12.62435565298211593, 16.36602540378438420, 9.500000000000000000 ) ) ;
#21298 = DIRECTION ( 'NONE',  ( 0.9945218953682729568, -0.1045284632676570929, -0.000000000000000000 ) ) ;
#21299 = CARTESIAN_POINT ( 'NONE',  ( -23.18519655538999658, 0.9190088410037334787, -20.58602323490189789 ) ) ;
#21300 = CARTESIAN_POINT ( 'NONE',  ( 33.79199353566443875, -13.57530639058761679, -9.302689660099131785 ) ) ;
#21301 = EDGE_LOOP ( 'NONE', ( #16178, #13554 ) ) ;
#21302 = DIRECTION ( 'NONE',  ( -0.1045284632676437564, 0.9945218953682744001, 0.000000000000000000 ) ) ;
#21303 = ORIENTED_EDGE ( 'NONE', *, *, #14228, .F. ) ;
#21304 = B_SPLINE_CURVE_WITH_KNOTS ( 'NONE', 3,
 ( #3988, #17205, #13734, #952, #16390, #29582, #32231, #10904, #22873, #23291, #28776, #26125, #25723, #1760, #35076, #13534, #25519, #37920 ),
 .UNSPECIFIED., .F., .F.,
 ( 4, 2, 2, 2, 2, 2, 2, 2, 4 ),
 ( 0.000000000000000000, 0.1250000000000000278, 0.2500000000000000555, 0.3750000000000001110, 0.5000000000000000000, 0.6250000000000000000, 0.7500000000000000000, 0.8750000000000001110, 1.000000000000000000 ),
 .UNSPECIFIED. ) ;
#21305 = DIRECTION ( 'NONE',  ( 0.3090169943749448977, -0.9510565162951543083, 0.000000000000000000 ) ) ;
#21306 = CARTESIAN_POINT ( 'NONE',  ( 32.33143948541787438, 1.358872982501792226, 11.00000000000000000 ) ) ;
#21307 = ADVANCED_FACE ( 'NONE', ( #38099 ), #19613, .F. ) ;
#21308 = AXIS2_PLACEMENT_3D ( 'NONE', #6249, #12548, #15794 ) ;
#21309 = VECTOR ( 'NONE', #7591, 999.9999999999998863 ) ;
#21310 = CYLINDRICAL_SURFACE ( 'NONE', #4520, 60.00000000000007816 ) ;
#21311 = VERTEX_POINT ( 'NONE', #15973 ) ;
#21312 = ADVANCED_FACE ( 'NONE', ( #9484 ), #6421, .F. ) ;
#21313 = CARTESIAN_POINT ( 'NONE',  ( -1.746686391856493215, 21.93407269432965379, -24.23685970402688383 ) ) ;
#21314 = CARTESIAN_POINT ( 'NONE',  ( -5.622359283595719681, 36.35732237484531026, 10.76099332938163755 ) ) ;
#21315 = DIRECTION ( 'NONE',  ( 0.3090169943749450643, -0.9510565162951544194, 0.000000000000000000 ) ) ;
#21316 = CIRCLE ( 'NONE', #14178, 0.4999999999999997780 ) ;
#21317 = CARTESIAN_POINT ( 'NONE',  ( 2.590671895605813901, 26.81128010880988199, 23.00000000000000355 ) ) ;
#21318 = CARTESIAN_POINT ( 'NONE',  ( 27.74479198965729410, -21.38649675605601885, -11.08839524368410601 ) ) ;
#21319 = CARTESIAN_POINT ( 'NONE',  ( 20.01142798620482921, 14.91867193257671431, -6.451173775806654298 ) ) ;
#21320 = CARTESIAN_POINT ( 'NONE',  ( 11.04322220929187104, 28.65258582978126256, -13.13952990371131513 ) ) ;
#21321 = ORIENTED_EDGE ( 'NONE', *, *, #23505, .F. ) ;
#21322 = EDGE_CURVE ( 'NONE', #20949, #17265, #17269, .T. ) ;
#21323 = CARTESIAN_POINT ( 'NONE',  ( -18.43203766348224804, 9.199961657135451887, -27.73406356219650704 ) ) ;
#21324 = DIRECTION ( 'NONE',  ( -1.000000000000000000, 0.000000000000000000, 0.000000000000000000 ) ) ;
#21325 = CARTESIAN_POINT ( 'NONE',  ( 12.04973099137657755, -21.47510576933752091, -18.43454808460629124 ) ) ;
#21326 = LINE ( 'NONE', #5878, #310 ) ;
#21327 = DIRECTION ( 'NONE',  ( -1.000000000000000000, 0.000000000000000000, 0.000000000000000000 ) ) ;
#21328 = CARTESIAN_POINT ( 'NONE',  ( -11.87729697930262951, 19.39812291060849603, -21.61417898203982801 ) ) ;
#21329 = CARTESIAN_POINT ( 'NONE',  ( -13.82671766433831095, -15.58877518772614046, -27.14361040387732160 ) ) ;
#21330 = CARTESIAN_POINT ( 'NONE',  ( 8.649194241449905007, -18.71206457532732514, -28.12513526114011952 ) ) ;
#21331 = CARTESIAN_POINT ( 'NONE',  ( 11.14453731054108765, 31.86177010143591204, 10.99999999999999645 ) ) ;
#21332 = ORIENTED_EDGE ( 'NONE', *, *, #20863, .F. ) ;
#21333 = ORIENTED_EDGE ( 'NONE', *, *, #11260, .F. ) ;
#21334 = CARTESIAN_POINT ( 'NONE',  ( -9.013010211479819844, 27.20962005112951942, -15.91364778940325486 ) ) ;
#21335 = EDGE_CURVE ( 'NONE', #35565, #23735, #15770, .T. ) ;
#21336 = CARTESIAN_POINT ( 'NONE',  ( -14.31603901957233660, 19.98981538725089990, 10.49999999999999467 ) ) ;
#21337 = CARTESIAN_POINT ( 'NONE',  ( 10.16520467992603294, 20.33931832809677331, 13.00000000000000178 ) ) ;
#21338 = EDGE_CURVE ( 'NONE', #10384, #3967, #14153, .T. ) ;
#21339 = VECTOR ( 'NONE', #10705, 1000.000000000000000 ) ;
#21340 = CIRCLE ( 'NONE', #37547, 0.4999999999999997780 ) ;
#21341 = CARTESIAN_POINT ( 'NONE',  ( 10.49474413300069386, 21.89971208337373909, 10.50000000000000000 ) ) ;
#21342 = EDGE_LOOP ( 'NONE', ( #13622, #8988, #24537, #11856 ) ) ;
#21343 = CARTESIAN_POINT ( 'NONE',  ( 23.31464182441019872, 0.5588091542327003891, -20.54288570421724458 ) ) ;
#21344 = LINE ( 'NONE', #5492, #39471 ) ;
#21345 = CARTESIAN_POINT ( 'NONE',  ( -2.247473515615844075, 16.63111439559750693, 13.00000000000000178 ) ) ;
#21346 = AXIS2_PLACEMENT_3D ( 'NONE', #5118, #39637, #23607 ) ;
#21347 = ORIENTED_EDGE ( 'NONE', *, *, #14771, .F. ) ;
#21348 = CARTESIAN_POINT ( 'NONE',  ( -30.47171451085012706, 0.001944469067151908051, -7.827869195058648977 ) ) ;
#21349 = CARTESIAN_POINT ( 'NONE',  ( -6.953812613386785912, 14.77701242934787906, 6.000000000000000000 ) ) ;
#21350 = ORIENTED_EDGE ( 'NONE', *, *, #11909, .F. ) ;
#21351 = CARTESIAN_POINT ( 'NONE',  ( 27.02919598657182831, -4.767359354157993501, -16.93437983263991953 ) ) ;
#21352 = ORIENTED_EDGE ( 'NONE', *, *, #10340, .T. ) ;
#21353 = CARTESIAN_POINT ( 'NONE',  ( -10.68781676061691854, 36.56370694841923807, 13.32518128616608699 ) ) ;
#21354 = CARTESIAN_POINT ( 'NONE',  ( -11.59681349794144012, -18.61320969085484833, 20.50957957746048521 ) ) ;
#21355 = CARTESIAN_POINT ( 'NONE',  ( 9.331903152615748098, 11.35703883385568780, 10.49999999999999822 ) ) ;
#21356 = CARTESIAN_POINT ( 'NONE',  ( 5.569982264780531267, 31.74975025675623286, 19.99202127657103745 ) ) ;
#21357 = CARTESIAN_POINT ( 'NONE',  ( -3.558056881628413937, 8.165525635826545781, 10.94611345180491035 ) ) ;
#21358 = ORIENTED_EDGE ( 'NONE', *, *, #32736, .T. ) ;
#21359 = ADVANCED_FACE ( 'NONE', ( #19824 ), #32423, .T. ) ;
#21360 = CARTESIAN_POINT ( 'NONE',  ( 10.33648234394583376, 33.08013173297155873, 10.49999999999999822 ) ) ;
#21361 = DIRECTION ( 'NONE',  ( -0.3090169943749573878, -0.9510565162951503115, 0.000000000000000000 ) ) ;
#21362 = VECTOR ( 'NONE', #5723, 1000.000000000000000 ) ;
#21364 = CIRCLE ( 'NONE', #9683, 1.000000000000000888 ) ;
#21363 = CARTESIAN_POINT ( 'NONE',  ( 5.245106710023661023, 26.98899556905067598, -17.69490459739507671 ) ) ;
#21365 = FACE_OUTER_BOUND ( 'NONE', #4195, .T. ) ;
#21366 = CARTESIAN_POINT ( 'NONE',  ( 11.24817812657392224, -17.21924521237894368, -28.63632236487146798 ) ) ;
#21367 = CARTESIAN_POINT ( 'NONE',  ( -9.844611323930809732, 11.18224604797046773, 7.076227724509050354 ) ) ;
#21368 = VECTOR ( 'NONE', #34545, 1000.000000000000000 ) ;
#21369 = DIRECTION ( 'NONE',  ( 0.000000000000000000, 0.000000000000000000, 1.000000000000000000 ) ) ;
#21370 = CARTESIAN_POINT ( 'NONE',  ( 0.2655024426717602637, 36.24516302788250499, 13.00000000000000178 ) ) ;
#21371 = VERTEX_POINT ( 'NONE', #7414 ) ;
#21372 = CARTESIAN_POINT ( 'NONE',  ( -11.09715496686145819, 17.48622750951172833, -27.44966945835485816 ) ) ;
#21373 = CARTESIAN_POINT ( 'NONE',  ( -29.73172958077499572, -1.192874570366647458, 17.92354375535250810 ) ) ;
#21374 = CARTESIAN_POINT ( 'NONE',  ( 9.447256496083108246, -18.24336034194182687, -28.70984161428601666 ) ) ;
#21375 = CARTESIAN_POINT ( 'NONE',  ( 1.525645716490520387, 8.212903943950921715, 7.000000000000000000 ) ) ;
#21376 = ORIENTED_EDGE ( 'NONE', *, *, #19085, .F. ) ;
#21377 = ORIENTED_EDGE ( 'NONE', *, *, #5810, .F. ) ;
#21379 = CARTESIAN_POINT ( 'NONE',  ( 3.835130509701798918, 15.55077355964573904, 6.000000000000000000 ) ) ;
#21378 = CARTESIAN_POINT ( 'NONE',  ( -10.24004248254194316, 18.41327472192288539, -26.12338179500006419 ) ) ;
#21380 = CARTESIAN_POINT ( 'NONE',  ( -19.26074050860073328, -27.02685104100921620, -7.267539198847054571 ) ) ;
#21381 = CARTESIAN_POINT ( 'NONE',  ( 14.58123527826104215, 20.01612550765316101, 10.49999999999999467 ) ) ;
#21382 = VERTEX_POINT ( 'NONE', #17395 ) ;
#21383 = CARTESIAN_POINT ( 'NONE',  ( -30.96917735819973672, -10.61658571351321356, -12.94788124637345206 ) ) ;
#21384 = CARTESIAN_POINT ( 'NONE',  ( -11.65776438499378109, -21.50447217315263870, -18.47646201114688225 ) ) ;
#21385 = CARTESIAN_POINT ( 'NONE',  ( 39.05366788733209660, -6.582903524762724778, 22.99999999999999289 ) ) ;
#21386 = EDGE_LOOP ( 'NONE', ( #16388, #20356 ) ) ;
#21387 = CARTESIAN_POINT ( 'NONE',  ( 26.98308923628663791, 0.4609988587420678074, -14.49164037743313926 ) ) ;
#21388 = DIRECTION ( 'NONE',  ( 0.000000000000000000, 0.000000000000000000, -1.000000000000000000 ) ) ;
#21389 = LINE ( 'NONE', #24634, #21878 ) ;
#21390 = ADVANCED_FACE ( 'NONE', ( #4580 ), #38302, .F. ) ;
#21391 = ORIENTED_EDGE ( 'NONE', *, *, #14263, .T. ) ;
#21392 = CARTESIAN_POINT ( 'NONE',  ( -21.72644794604407537, 0.6368340560596529309, -23.84291411478136880 ) ) ;
#21393 = ORIENTED_EDGE ( 'NONE', *, *, #29900, .T. ) ;
#21394 = CARTESIAN_POINT ( 'NONE',  ( 31.73450339093934858, -1.000272218596043761, -5.933748666415237238 ) ) ;
#21395 = AXIS2_PLACEMENT_3D ( 'NONE', #31998, #25695, #25895 ) ;
#21396 = CARTESIAN_POINT ( 'NONE',  ( -1.590043107810763079, 12.61456814725308107, 10.50000000000000000 ) ) ;
#21397 = CARTESIAN_POINT ( 'NONE',  ( 29.73172958077661931, -1.192874570368608333, 17.92354375535250810 ) ) ;
#21398 = EDGE_LOOP ( 'NONE', ( #18072, #3016, #38510 ) ) ;
#21399 = CARTESIAN_POINT ( 'NONE',  ( -27.01695987841192093, 3.517937595036570997, -9.299659907420654292 ) ) ;
#21400 = CIRCLE ( 'NONE', #39581, 15.00000000000000000 ) ;
#21401 = LINE ( 'NONE', #36840, #14201 ) ;
#21402 = DIRECTION ( 'NONE',  ( 1.000000000000000000, 0.000000000000000000, 0.000000000000000000 ) ) ;
#21403 = CARTESIAN_POINT ( 'NONE',  ( -17.42101839920251649, -19.25229542401852001, 20.69868183039780618 ) ) ;
#21404 = DIRECTION ( 'NONE',  ( 0.000000000000000000, 0.000000000000000000, 1.000000000000000000 ) ) ;
#21405 = DIRECTION ( 'NONE',  ( -0.000000000000000000, -0.000000000000000000, -1.000000000000000000 ) ) ;
#21406 = DIRECTION ( 'NONE',  ( 0.3090169943749448977, -0.9510565162951543083, 0.000000000000000000 ) ) ;
#21407 = ORIENTED_EDGE ( 'NONE', *, *, #14496, .F. ) ;
#21408 = CARTESIAN_POINT ( 'NONE',  ( -23.81473431349828829, 6.976256285597340678, -11.82319584038477522 ) ) ;
#21409 = CARTESIAN_POINT ( 'NONE',  ( 0.000000000000000000, 22.50000000000000355, 7.000000000000000000 ) ) ;
#21410 = ADVANCED_FACE ( 'NONE', ( #10473 ), #12262, .F. ) ;
#21411 = DIRECTION ( 'NONE',  ( 0.000000000000000000, 0.000000000000000000, 1.000000000000000000 ) ) ;
#21412 = CARTESIAN_POINT ( 'NONE',  ( 14.45205179786681882, -15.04654671938721400, -27.10327764158452268 ) ) ;
#21413 = DIRECTION ( 'NONE',  ( -0.9781476007338041345, 0.2079116908177663092, 0.000000000000000000 ) ) ;
#21414 = CARTESIAN_POINT ( 'NONE',  ( 10.80899027733819295, 17.41890095272876593, -30.00000000000000000 ) ) ;
#21415 = VECTOR ( 'NONE', #22006, 1000.000000000000000 ) ;
#21416 = ORIENTED_EDGE ( 'NONE', *, *, #25775, .T. ) ;
#21417 = CARTESIAN_POINT ( 'NONE',  ( -15.42122190845770646, 23.49383705188275329, -10.69673651877608478 ) ) ;
#21418 = CARTESIAN_POINT ( 'NONE',  ( -26.93475362026834219, -11.92845428170184974, 20.82122704794080192 ) ) ;
#21419 = CARTESIAN_POINT ( 'NONE',  ( -7.014595103779441843, 35.79644522156330311, 7.000000000000000000 ) ) ;
#21420 = CARTESIAN_POINT ( 'NONE',  ( 15.18681916921612363, 26.24042416626922503, -8.298040651035869075 ) ) ;
#21421 = VERTEX_POINT ( 'NONE', #30586 ) ;
#21422 = DIRECTION ( 'NONE',  ( 0.000000000000000000, 0.000000000000000000, 1.000000000000000000 ) ) ;
#21423 = AXIS2_PLACEMENT_3D ( 'NONE', #35652, #29755, #20818 ) ;
#21424 = VERTEX_POINT ( 'NONE', #18588 ) ;
#21426 = CARTESIAN_POINT ( 'NONE',  ( -1.838889047819898037, 31.15129278236396360, 9.000000000000001776 ) ) ;
#21425 = CARTESIAN_POINT ( 'NONE',  ( -15.31970618788670180, 27.02672079109983727, -5.943192127738577746 ) ) ;
#21427 = CARTESIAN_POINT ( 'NONE',  ( -11.69740102143367544, -20.95835256283988102, -19.47752585436962036 ) ) ;
#21428 = DIRECTION ( 'NONE',  ( 0.4067366430757888840, -0.9135454576426058626, 0.000000000000000000 ) ) ;
#21429 = CARTESIAN_POINT ( 'NONE',  ( -34.01753683000946893, -17.82260201088918450, -5.856192742791406225 ) ) ;
#21430 = CARTESIAN_POINT ( 'NONE',  ( -13.89005016234717971, -26.28256486574421658, -6.419270497917506368 ) ) ;
#21431 = CARTESIAN_POINT ( 'NONE',  ( 1.449462053036050024, 12.07351642418171167, 10.74999999999999112 ) ) ;
#21432 = CARTESIAN_POINT ( 'NONE',  ( 15.50276458342831987, 23.27946725895370861, -10.70176112796715095 ) ) ;
#21433 = VERTEX_POINT ( 'NONE', #11495 ) ;
#21434 = CARTESIAN_POINT ( 'NONE',  ( 23.64686652105454812, 7.232955847004403971, -11.82926767496736353 ) ) ;
#21435 = EDGE_CURVE ( 'NONE', #8296, #8510, #11205, .T. ) ;
#21436 = DIRECTION ( 'NONE',  ( 1.000000000000000000, 0.000000000000000000, 0.000000000000000000 ) ) ;
#21437 = DIRECTION ( 'NONE',  ( 0.000000000000000000, 0.000000000000000000, 1.000000000000000000 ) ) ;
#21438 = CARTESIAN_POINT ( 'NONE',  ( -20.03448507352192465, -26.57026294638366437, -8.593633122198326646 ) ) ;
#21439 = ORIENTED_EDGE ( 'NONE', *, *, #17587, .T. ) ;
#21440 = CARTESIAN_POINT ( 'NONE',  ( -31.98245490244095635, -1.244365697959704420, -5.000000000000000000 ) ) ;
#21441 = EDGE_CURVE ( 'NONE', #2121, #30551, #39516, .T. ) ;
#21442 = CARTESIAN_POINT ( 'NONE',  ( 27.79148596755621625, 0.1202762638927254851, -13.50639119845660119 ) ) ;
#21443 = AXIS2_PLACEMENT_3D ( 'NONE', #30950, #30154, #21599 ) ;
#21444 = EDGE_CURVE ( 'NONE', #29636, #31286, #18194, .T. ) ;
#21445 = CARTESIAN_POINT ( 'NONE',  ( 25.82695510740672162, -7.282951130326176248, 20.82122704794095114 ) ) ;
#21446 = VERTEX_POINT ( 'NONE', #27327 ) ;
#21447 = EDGE_CURVE ( 'NONE', #1824, #26924, #5392, .T. ) ;
#21448 = CARTESIAN_POINT ( 'NONE',  ( 35.36940577612500647, -20.42053594592276866, -4.999999999999997335 ) ) ;
#21449 = CARTESIAN_POINT ( 'NONE',  ( 19.48557158514975285, -11.24999999999995737, 10.00000000000000000 ) ) ;
#21450 = ORIENTED_EDGE ( 'NONE', *, *, #28531, .F. ) ;
#21451 = CARTESIAN_POINT ( 'NONE',  ( -15.48853126089653642, -26.74269726827072446, -4.999999999999999112 ) ) ;
#21452 = LINE ( 'NONE', #6008, #24042 ) ;
#21453 = CARTESIAN_POINT ( 'NONE',  ( 12.89070168820767037, 15.82735026918957111, 10.83333333333333037 ) ) ;
#21454 = CARTESIAN_POINT ( 'NONE',  ( 3.763558953900551618, 36.71453398273495594, -8.854024335422799652 ) ) ;
#21455 = CARTESIAN_POINT ( 'NONE',  ( -5.362728154696096539, 13.41753630677062148, 10.50000000000000711 ) ) ;
#21456 = EDGE_CURVE ( 'NONE', #31127, #15571, #19467, .T. ) ;
#21457 = CARTESIAN_POINT ( 'NONE',  ( 14.36830325120613061, 20.48707633493483371, 10.99999999999999289 ) ) ;
#21458 = EDGE_CURVE ( 'NONE', #27468, #20584, #17806, .T. ) ;
#21459 = DIRECTION ( 'NONE',  ( 0.000000000000000000, 0.000000000000000000, -1.000000000000000000 ) ) ;
#21460 = DIRECTION ( 'NONE',  ( 0.9135454576425988682, -0.4067366430758048157, 0.000000000000000000 ) ) ;
#21461 = DIRECTION ( 'NONE',  ( -0.4999999999999920619, 0.8660254037844432595, 0.000000000000000000 ) ) ;
#21462 = CARTESIAN_POINT ( 'NONE',  ( -9.762440214458996124, -29.39637225280792521, 22.99999999999999645 ) ) ;
#21463 = CARTESIAN_POINT ( 'NONE',  ( 14.75730607214175905, 27.52521798300531586, -8.251418156868062681 ) ) ;
#21464 = LINE ( 'NONE', #27362, #22425 ) ;
#21465 = ORIENTED_EDGE ( 'NONE', *, *, #13287, .F. ) ;
#21467 = DIRECTION ( 'NONE',  ( -0.000000000000000000, -0.000000000000000000, -1.000000000000000000 ) ) ;
#21466 = CARTESIAN_POINT ( 'NONE',  ( -15.47687725686822802, 14.82734777190539077, -23.20797657644519418 ) ) ;
#21468 = CARTESIAN_POINT ( 'NONE',  ( -4.440836655099179353, 34.39106106163288246, 6.000000000000000000 ) ) ;
#21469 = AXIS2_PLACEMENT_3D ( 'NONE', #8065, #36111, #8269 ) ;
#21470 = CARTESIAN_POINT ( 'NONE',  ( 9.970553079590814605, -18.81210375092922149, -25.01410075462041149 ) ) ;
#21471 = CARTESIAN_POINT ( 'NONE',  ( -19.52232064119460375, -24.60346519530635589, -12.21144919225334213 ) ) ;
#21472 = CARTESIAN_POINT ( 'NONE',  ( 32.33143948541893309, 1.358872982500733961, 11.55979286843934695 ) ) ;
#21473 = CARTESIAN_POINT ( 'NONE',  ( 10.97317656914242967, 17.31587133052951089, -29.34811157007365523 ) ) ;
#21474 = ORIENTED_EDGE ( 'NONE', *, *, #2099, .T. ) ;
#21475 = CARTESIAN_POINT ( 'NONE',  ( -2.525645716490710679, 8.212903943950959018, 9.000000000000001776 ) ) ;
#21476 = CARTESIAN_POINT ( 'NONE',  ( -14.53998467467461353, -25.44454797919701505, -10.65503318047344194 ) ) ;
#21477 = CARTESIAN_POINT ( 'NONE',  ( -24.32690616642468839, -27.49953951067762148, 15.13084544680243049 ) ) ;
#21478 = CARTESIAN_POINT ( 'NONE',  ( -16.88793822083986740, -14.03095869258871531, -24.29931205907291769 ) ) ;
#21479 = CARTESIAN_POINT ( 'NONE',  ( 1.255466122108702232, -20.65231545638951616, -27.17923991438529185 ) ) ;
#21480 = CARTESIAN_POINT ( 'NONE',  ( 14.97130663709144294, 24.72598064263621609, -10.66823142197542928 ) ) ;
#21481 = CARTESIAN_POINT ( 'NONE',  ( 18.10664311642079483, 11.05995638511404167, -23.33310058690642919 ) ) ;
#21482 = DIRECTION ( 'NONE',  ( 0.8660254037844363761, -0.5000000000000039968, 0.000000000000000000 ) ) ;
#21483 = AXIS2_PLACEMENT_3D ( 'NONE', #36552, #8114, #5272 ) ;
#21484 = CARTESIAN_POINT ( 'NONE',  ( -3.705086238427029777, 21.62874139591992773, -24.30186519092085362 ) ) ;
#21485 = ORIENTED_EDGE ( 'NONE', *, *, #16613, .F. ) ;
#21486 = CARTESIAN_POINT ( 'NONE',  ( -34.30668518109128939, -6.458525508014972161, -7.647112954010694352 ) ) ;
#21487 = EDGE_CURVE ( 'NONE', #20155, #26406, #5869, .T. ) ;
#21488 = CARTESIAN_POINT ( 'NONE',  ( -17.15083734909836011, 27.26712758904658784, 12.73282698324853257 ) ) ;
#21489 = ORIENTED_EDGE ( 'NONE', *, *, #9769, .T. ) ;
#21490 = PLANE ( 'NONE',  #1874 ) ;
#21491 = CARTESIAN_POINT ( 'NONE',  ( 18.76532695907111403, -16.22790357942847805, 22.99999999999999289 ) ) ;
#21492 = CARTESIAN_POINT ( 'NONE',  ( -20.66892949074973984, 1.176045066688247598, -27.46922783559482895 ) ) ;
#21493 = CARTESIAN_POINT ( 'NONE',  ( 33.95993763334963234, -12.46657790436312752, -9.313543929707535085 ) ) ;
#21494 = AXIS2_PLACEMENT_3D ( 'NONE', #25205, #37603, #9770 ) ;
#21495 = VECTOR ( 'NONE', #16507, 1000.000000000000227 ) ;
#21496 = ORIENTED_EDGE ( 'NONE', *, *, #35310, .F. ) ;
#21497 = DIRECTION ( 'NONE',  ( -1.000000000000000000, 0.000000000000000000, 0.000000000000000000 ) ) ;
#21498 = VERTEX_POINT ( 'NONE', #12285 ) ;
#21499 = DIRECTION ( 'NONE',  ( 0.000000000000000000, 0.000000000000000000, 1.000000000000000000 ) ) ;
#21500 = FACE_OUTER_BOUND ( 'NONE', #23953, .T. ) ;
#21501 = CYLINDRICAL_SURFACE ( 'NONE', #13618, 0.4999999999999997780 ) ;
#21502 = ORIENTED_EDGE ( 'NONE', *, *, #38386, .F. ) ;
#21503 = CARTESIAN_POINT ( 'NONE',  ( -2.962397377419403899, 36.59740967881665341, -9.288886632304988566 ) ) ;
#21504 = FACE_OUTER_BOUND ( 'NONE', #10744, .T. ) ;
#21505 = DIRECTION ( 'NONE',  ( -1.000000000000000000, 0.000000000000000000, 0.000000000000000000 ) ) ;
#21506 = CIRCLE ( 'NONE', #24752, 1.000000000000000222 ) ;
#21507 = EDGE_CURVE ( 'NONE', #21421, #14341, #14740, .T. ) ;
#21508 = PLANE ( 'NONE',  #37689 ) ;
#21509 = CARTESIAN_POINT ( 'NONE',  ( 27.03181137051826255, -20.83723433176508166, -11.99698614993629064 ) ) ;
#21510 = EDGE_CURVE ( 'NONE', #13434, #3501, #37402, .T. ) ;
#21511 = CARTESIAN_POINT ( 'NONE',  ( 16.48441032495264835, 12.78878735330096994, -25.47995477096423755 ) ) ;
#21512 = CARTESIAN_POINT ( 'NONE',  ( 8.265145098949810532, 19.28472743380562804, -26.57823981897835708 ) ) ;
#21513 = ORIENTED_EDGE ( 'NONE', *, *, #18911, .F. ) ;
#21514 = CARTESIAN_POINT ( 'NONE',  ( -21.33856562183509098, 11.52826686442322845, -10.38518463479564957 ) ) ;
#21515 = CARTESIAN_POINT ( 'NONE',  ( 1.082972213713614407, 27.41125570341915818, 23.00000000000000000 ) ) ;
#21516 = CARTESIAN_POINT ( 'NONE',  ( 12.00181538804464232, -21.47850077996891471, -18.44043584019166104 ) ) ;
#21517 = DIRECTION ( 'NONE',  ( 0.9135454576426059736, 0.4067366430757888285, 0.000000000000000000 ) ) ;
#21518 = CARTESIAN_POINT ( 'NONE',  ( 19.54664213359407654, -11.28525909758385914, -19.69475445967423610 ) ) ;
#21519 = CARTESIAN_POINT ( 'NONE',  ( -12.11165721293594544, 19.94706872364197281, -20.53702604530188935 ) ) ;
#21520 = VECTOR ( 'NONE', #6652, 1000.000000000000000 ) ;
#21521 = APPLICATION_CONTEXT ( 'automotive_design' ) ;
#21522 = CARTESIAN_POINT ( 'NONE',  ( -14.83625493676444052, -17.72904731969334691, -22.21157065729462232 ) ) ;
#21523 = CARTESIAN_POINT ( 'NONE',  ( 12.69900848833330187, -25.52681193209280153, -9.268119605047994369 ) ) ;
#21524 = DIRECTION ( 'NONE',  ( -0.000000000000000000, -0.000000000000000000, -1.000000000000000000 ) ) ;
#21525 = ORIENTED_EDGE ( 'NONE', *, *, #23711, .F. ) ;
#21526 = CARTESIAN_POINT ( 'NONE',  ( -8.291105163447188175, 27.72608485885197638, -15.86983220121024729 ) ) ;
#21527 = CARTESIAN_POINT ( 'NONE',  ( 0.5000000000000000000, 37.50000000000000711, 10.49999999999999822 ) ) ;
#21528 = ADVANCED_FACE ( 'NONE', ( #39908 ), #33643, .F. ) ;
#21529 = DIRECTION ( 'NONE',  ( -1.000000000000000000, 0.000000000000000000, 0.000000000000000000 ) ) ;
#21530 = CARTESIAN_POINT ( 'NONE',  ( 13.63581098909226874, 27.45627467658428955, 7.000000000000000000 ) ) ;
#21531 = VERTEX_POINT ( 'NONE', #24475 ) ;
#21532 = CARTESIAN_POINT ( 'NONE',  ( 23.30637526650272662, 0.5818651227441539175, -20.54567832033172792 ) ) ;
#21533 = EDGE_CURVE ( 'NONE', #13142, #32713, #36872, .T. ) ;
#21534 = DIRECTION ( 'NONE',  ( 0.000000000000000000, 0.000000000000000000, 1.000000000000000000 ) ) ;
#21535 = AXIS2_PLACEMENT_3D ( 'NONE', #8460, #24296, #12104 ) ;
#21536 = CARTESIAN_POINT ( 'NONE',  ( 15.02235689379175732, 21.92659494635341844, 11.00000000000000000 ) ) ;
#21537 = ORIENTED_EDGE ( 'NONE', *, *, #23296, .F. ) ;
#21538 = CARTESIAN_POINT ( 'NONE',  ( -22.21240959074407684, 0.6992048922518714349, -22.73936558975926658 ) ) ;
#21539 = CARTESIAN_POINT ( 'NONE',  ( 9.677076426724161351, 26.69573495723207301, 10.50000000000000355 ) ) ;
#21540 = VERTEX_POINT ( 'NONE', #5982 ) ;
#21541 = CARTESIAN_POINT ( 'NONE',  ( 22.77169554655636219, -3.983247555766573189, -22.21157357009845512 ) ) ;
#21542 = EDGE_CURVE ( 'NONE', #39554, #2993, #24675, .T. ) ;
#21543 = ORIENTED_EDGE ( 'NONE', *, *, #30399, .F. ) ;
#21544 = CARTESIAN_POINT ( 'NONE',  ( -15.81288461013852498, 30.89878388227737105, 12.73282698324828743 ) ) ;
#21545 = CARTESIAN_POINT ( 'NONE',  ( 6.077490221915134327, -14.56650175400723946, 20.99999999999999645 ) ) ;
#21546 = CARTESIAN_POINT ( 'NONE',  ( -1.281338032051963616, 37.44565299484865051, 7.102637441331450141 ) ) ;
#21547 = CARTESIAN_POINT ( 'NONE',  ( 7.604809270644918406, 28.95580224300140770, 20.25080042701566541 ) ) ;
#21548 = CARTESIAN_POINT ( 'NONE',  ( -11.81630298851966288, 31.79381426990562787, 7.000000000000000000 ) ) ;
#21549 = ORIENTED_EDGE ( 'NONE', *, *, #38895, .F. ) ;
#21550 = CIRCLE ( 'NONE', #9227, 16.00000000000000000 ) ;
#21551 = DIRECTION ( 'NONE',  ( 0.000000000000000000, 0.000000000000000000, 1.000000000000000000 ) ) ;
#21552 = CARTESIAN_POINT ( 'NONE',  ( -10.32951289851619592, 32.69782367585516170, 10.83333333333333037 ) ) ;
#21553 = LINE ( 'NONE', #17924, #2025 ) ;
#21554 = EDGE_CURVE ( 'NONE', #39380, #19863, #30181, .T. ) ;
#21555 = EDGE_CURVE ( 'NONE', #11050, #39108, #37068, .T. ) ;
#21556 = DIRECTION ( 'NONE',  ( 0.5000000000000039968, 0.8660254037844363761, 0.000000000000000000 ) ) ;
#21557 = EDGE_CURVE ( 'NONE', #26271, #37740, #25707, .T. ) ;
#21558 = CARTESIAN_POINT ( 'NONE',  ( 4.496862015843431593, 20.00989232716073118, -29.23636761809433082 ) ) ;
#21559 = CARTESIAN_POINT ( 'NONE',  ( 8.401171878996485987, 21.11424711454080594, 7.000000000000000000 ) ) ;
#21560 = VECTOR ( 'NONE', #12795, 1000.000000000000114 ) ;
#21561 = CARTESIAN_POINT ( 'NONE',  ( 15.53547054105565373, -24.29315558060116231, -13.36240988604506263 ) ) ;
#21562 = FACE_OUTER_BOUND ( 'NONE', #28702, .T. ) ;
#21563 = CARTESIAN_POINT ( 'NONE',  ( -8.505700342264141511, 22.10876900990917804, 9.000000000000001776 ) ) ;
#21564 = PLANE ( 'NONE',  #29135 ) ;
#21565 = ORIENTED_EDGE ( 'NONE', *, *, #12037, .T. ) ;
#21566 = CARTESIAN_POINT ( 'NONE',  ( -15.03387384203356270, 25.91884056606313536, -9.238937710698264638 ) ) ;
#21567 = CIRCLE ( 'NONE', #5997, 0.5000000000000004441 ) ;
#21568 = CARTESIAN_POINT ( 'NONE',  ( -32.94198380406523796, -19.01906321691725310, 16.87380292611441845 ) ) ;
#21569 = CARTESIAN_POINT ( 'NONE',  ( 10.44557952003627221, -19.60207686399620286, -22.74606572134008431 ) ) ;
#21570 = CARTESIAN_POINT ( 'NONE',  ( -14.36910708881314669, 26.64307479831630587, 10.76099332938163577 ) ) ;
#21571 = VERTEX_POINT ( 'NONE', #34616 ) ;
#21572 = ORIENTED_EDGE ( 'NONE', *, *, #28354, .T. ) ;
#21573 = CARTESIAN_POINT ( 'NONE',  ( -10.38118103384230828, 18.73610608265249766, -24.88814054586562818 ) ) ;
#21574 = CARTESIAN_POINT ( 'NONE',  ( -14.44439269762431977, -21.86739633494050139, -17.20223798650874869 ) ) ;
#21575 = EDGE_CURVE ( 'NONE', #5290, #5502, #31172, .T. ) ;
#21576 = DIRECTION ( 'NONE',  ( 1.000000000000000000, 0.000000000000000000, 0.000000000000000000 ) ) ;
#21577 = ORIENTED_EDGE ( 'NONE', *, *, #26621, .F. ) ;
#21578 = CARTESIAN_POINT ( 'NONE',  ( -19.82898810763364494, -5.533127045182635761, -28.50453774944905661 ) ) ;
#21579 = CARTESIAN_POINT ( 'NONE',  ( -15.28548941152575402, -26.69066991962944257, -5.000000000000000888 ) ) ;
#21580 = CARTESIAN_POINT ( 'NONE',  ( 0.5000000000000000000, 37.50000000000000711, 10.63089969389957190 ) ) ;
#21581 = EDGE_LOOP ( 'NONE', ( #1282, #5941, #39309, #28731 ) ) ;
#21582 = CARTESIAN_POINT ( 'NONE',  ( 30.64962079249725946, 0.2186612821100236970, -5.000000000000000000 ) ) ;
#21583 = ADVANCED_FACE ( 'NONE', ( #37665 ), #19170, .F. ) ;
#21584 = CARTESIAN_POINT ( 'NONE',  ( 8.927394655428267711, 11.06314620770944757, 11.00000000000000000 ) ) ;
#21585 = ORIENTED_EDGE ( 'NONE', *, *, #37178, .T. ) ;
#21586 = CARTESIAN_POINT ( 'NONE',  ( -30.50745882448537927, -0.03539364285743687444, -7.826725409455514537 ) ) ;
#21587 = ORIENTED_EDGE ( 'NONE', *, *, #16116, .T. ) ;
#21588 = CARTESIAN_POINT ( 'NONE',  ( 32.12760839428420212, -2.228125769087125896, -8.203263732686945531 ) ) ;
#21589 = CIRCLE ( 'NONE', #26781, 17.00000000000000000 ) ;
#21590 = CARTESIAN_POINT ( 'NONE',  ( 6.128519550197534471, -19.61146684927020090, -30.00000000000000711 ) ) ;
#21591 = CARTESIAN_POINT ( 'NONE',  ( 30.60828605274730663, -21.42068866017963913, 17.42190598798431012 ) ) ;
#21592 = EDGE_LOOP ( 'NONE', ( #1301, #12991, #15993 ) ) ;
#21593 = AXIS2_PLACEMENT_3D ( 'NONE', #19568, #13672, #6960 ) ;
#21594 = CARTESIAN_POINT ( 'NONE',  ( -23.09610976977102936, 3.527081606721067075, -18.74855405513135409 ) ) ;
#21595 = CARTESIAN_POINT ( 'NONE',  ( -11.08846162081388975, 2.083081287325696529, 10.00000000000000000 ) ) ;
#21596 = CYLINDRICAL_SURFACE ( 'NONE', #27784, 1.000000000000000000 ) ;
#21597 = CIRCLE ( 'NONE', #37804, 0.5000000000000004441 ) ;
#21598 = CARTESIAN_POINT ( 'NONE',  ( 0.000000000000000000, 22.50000000000000355, 13.00000000000000178 ) ) ;
#21599 = DIRECTION ( 'NONE',  ( 1.000000000000000000, 0.000000000000000000, 0.000000000000000000 ) ) ;
#21600 = VECTOR ( 'NONE', #15762, 1000.000000000000000 ) ;
#21601 = FACE_BOUND ( 'NONE', #19845, .T. ) ;
#21602 = CARTESIAN_POINT ( 'NONE',  ( 22.71454497019403362, 13.11424865306083731, 13.92931973827808889 ) ) ;
#21603 = ORIENTED_EDGE ( 'NONE', *, *, #31342, .F. ) ;
#21604 = CARTESIAN_POINT ( 'NONE',  ( -20.11046056464997633, 6.477547240074802204, -24.32480941670467089 ) ) ;
#21605 = DIRECTION ( 'NONE',  ( 0.1045284632676570929, 0.9945218953682730678, 0.000000000000000000 ) ) ;
#21606 = DIRECTION ( 'NONE',  ( 0.000000000000000000, 0.000000000000000000, 1.000000000000000000 ) ) ;
#21607 = CARTESIAN_POINT ( 'NONE',  ( 20.57510288040941049, -22.72408697488640783, -13.98806764414992898 ) ) ;
#21608 = CARTESIAN_POINT ( 'NONE',  ( -13.28401428800407658, 15.85743772853297884, 10.49999999999999822 ) ) ;
#21609 = CARTESIAN_POINT ( 'NONE',  ( 15.02598156427579568, 26.38482746277715307, -8.756742615304116129 ) ) ;
#21610 = VECTOR ( 'NONE', #13155, 999.9999999999998863 ) ;
#21611 = VERTEX_POINT ( 'NONE', #6377 ) ;
#21612 = CARTESIAN_POINT ( 'NONE',  ( -12.90072778892209904, 17.70939849946352851, -22.91841346334786422 ) ) ;
#21613 = CARTESIAN_POINT ( 'NONE',  ( -17.21213525677265821, -20.06193531423681620, 20.50957957746029692 ) ) ;
#21614 = VECTOR ( 'NONE', #36867, 1000.000000000000000 ) ;
#21615 = CARTESIAN_POINT ( 'NONE',  ( 17.34253826607186255, 27.32041144404028543, -5.000000000000000000 ) ) ;
#21616 = CARTESIAN_POINT ( 'NONE',  ( 11.06077487293502593, 17.41132527382090700, -28.07864658204483277 ) ) ;
#21617 = VERTEX_POINT ( 'NONE', #12479 ) ;
#21618 = DIRECTION ( 'NONE',  ( 1.000000000000000000, 0.000000000000000000, 0.000000000000000000 ) ) ;
#21619 = VERTEX_POINT ( 'NONE', #22212 ) ;
#21621 = CARTESIAN_POINT ( 'NONE',  ( 9.625795778761983001, 10.95253033666821274, 11.00000000000000000 ) ) ;
#21620 = CARTESIAN_POINT ( 'NONE',  ( -14.73753967824242572, 25.92079578855301847, -10.16159616314446268 ) ) ;
#21622 = CARTESIAN_POINT ( 'NONE',  ( -9.570498547032590508, -18.18000853095062297, -28.70499904869090102 ) ) ;
#21623 = CARTESIAN_POINT ( 'NONE',  ( -14.06524961900331760, 27.71236540882611621, 7.499999999999993783 ) ) ;
#21624 = AXIS2_PLACEMENT_3D ( 'NONE', #35856, #2338, #14116 ) ;
#21625 = ORIENTED_EDGE ( 'NONE', *, *, #17618, .F. ) ;
#21626 = CARTESIAN_POINT ( 'NONE',  ( -18.37356219290808568, -9.636757534816835502, -27.70765190437884939 ) ) ;
#21627 = CARTESIAN_POINT ( 'NONE',  ( -8.733449382607537004, -18.59056498759259313, -28.73589422697259366 ) ) ;
#21628 = LINE ( 'NONE', #15540, #20275 ) ;
#21629 = CARTESIAN_POINT ( 'NONE',  ( 14.40945247603743340, 22.05875077139578266, -14.55621836163558847 ) ) ;
#21630 = ORIENTED_EDGE ( 'NONE', *, *, #30691, .T. ) ;
#21631 = CARTESIAN_POINT ( 'NONE',  ( 23.77809889112756991, 5.422375568838193161, -14.77688470156370038 ) ) ;
#21632 = CARTESIAN_POINT ( 'NONE',  ( -2.211402178667006169, 32.38366924255629442, 13.00000000000000178 ) ) ;
#21633 = DIRECTION ( 'NONE',  ( -1.000000000000000000, 0.000000000000000000, 0.000000000000000000 ) ) ;
#21634 = CARTESIAN_POINT ( 'NONE',  ( -0.5000000000000005551, 32.50000000000000000, 10.49999999999999645 ) ) ;
#21635 = ORIENTED_EDGE ( 'NONE', *, *, #37430, .T. ) ;
#21636 = CARTESIAN_POINT ( 'NONE',  ( -31.00339467208933542, -1.147717236077904213, -9.169194955842794315 ) ) ;
#21637 = AXIS2_PLACEMENT_3D ( 'NONE', #14117, #11678, #29354 ) ;
#21638 = CARTESIAN_POINT ( 'NONE',  ( 31.15015558338321711, -0.2976252405140638047, -5.472529613951848226 ) ) ;
#21639 = CARTESIAN_POINT ( 'NONE',  ( -5.632984386902246676, 36.38118674759818560, 10.68306085400122996 ) ) ;
#21640 = CIRCLE ( 'NONE', #26189, 1.000000000000000222 ) ;
#21641 = CARTESIAN_POINT ( 'NONE',  ( 25.38348611796611110, -5.460896781497905472, 20.69868183039781329 ) ) ;
#21642 = EDGE_LOOP ( 'NONE', ( #18627, #23500, #22186, #29471 ) ) ;
#21643 = CARTESIAN_POINT ( 'NONE',  ( 20.90924525106828114, -8.502318254486461058, -19.80438750953544513 ) ) ;
#21644 = VECTOR ( 'NONE', #5621, 1000.000000000000000 ) ;
#21645 = CARTESIAN_POINT ( 'NONE',  ( -1.693998953219649772, 12.12549434688617822, 10.00000000000000000 ) ) ;
#21646 = VERTEX_POINT ( 'NONE', #96 ) ;
#21647 = CARTESIAN_POINT ( 'NONE',  ( 5.237540274239914417, 35.49300472853430222, 7.000000000000000000 ) ) ;
#21648 = CARTESIAN_POINT ( 'NONE',  ( 11.14717238216093520, 32.53695909538286202, 7.000000000000000000 ) ) ;
#21649 = PLANE ( 'NONE',  #24218 ) ;
#21650 = CARTESIAN_POINT ( 'NONE',  ( 2.482818899334112928, 24.48995573783189528, -20.72365887979838206 ) ) ;
#21651 = CARTESIAN_POINT ( 'NONE',  ( -14.52509594610762456, 21.97885917798744870, 11.00000000000000000 ) ) ;
#21652 = EDGE_CURVE ( 'NONE', #18499, #31487, #28323, .T. ) ;
#21653 = DIRECTION ( 'NONE',  ( 0.8090169943749426773, -0.5877852522924797984, 0.000000000000000000 ) ) ;
#21654 = CARTESIAN_POINT ( 'NONE',  ( 7.530592408760855783, 11.28437794979193498, 10.00000000000000000 ) ) ;
#21655 = CARTESIAN_POINT ( 'NONE',  ( 4.481940917958135095, 8.628727325586426744, 7.000000000000000000 ) ) ;
#21656 = LINE ( 'NONE', #34059, #39127 ) ;
#21657 = PRESENTATION_STYLE_ASSIGNMENT (( #16166 ) ) ;
#21658 = CARTESIAN_POINT ( 'NONE',  ( 15.01573743325078070, 27.63731046468882724, -6.866476842728680197 ) ) ;
#21659 = DIRECTION ( 'NONE',  ( 0.000000000000000000, 0.000000000000000000, 1.000000000000000000 ) ) ;
#21660 = ORIENTED_EDGE ( 'NONE', *, *, #4916, .T. ) ;
#21662 = CARTESIAN_POINT ( 'NONE',  ( 12.05736835487432579, 14.38397459621550567, 10.49999999999999822 ) ) ;
#21661 = CARTESIAN_POINT ( 'NONE',  ( -18.09191307318060993, 16.86591247271400107, -11.82766105011013380 ) ) ;
#21663 = VECTOR ( 'NONE', #11073, 1000.000000000000000 ) ;
#21664 = EDGE_CURVE ( 'NONE', #18489, #30503, #10230, .T. ) ;
#21665 = CARTESIAN_POINT ( 'NONE',  ( 1.623731701744046241, 25.43444280220171194, 6.000000000000000000 ) ) ;
#21666 = CARTESIAN_POINT ( 'NONE',  ( 9.571804183446699810, -18.27277504971789668, -28.07733812879041935 ) ) ;
#21667 = EDGE_CURVE ( 'NONE', #3856, #2749, #348, .T. ) ;
#21668 = CARTESIAN_POINT ( 'NONE',  ( -21.33353929772287216, -26.74474634351298974, -7.673098688866929251 ) ) ;
#21669 = CYLINDRICAL_SURFACE ( 'NONE', #32112, 21.00000000000001776 ) ;
#21670 = CARTESIAN_POINT ( 'NONE',  ( 12.64671789796098444, 21.06331887642912548, -18.45078820372820871 ) ) ;
#21671 = B_SPLINE_SURFACE_WITH_KNOTS ( 'NONE', 1, 3, ( 
 ( #33339, #30075, #8740, #39809, #5683, #37168, #30280, #8942, #3041, #5288 ),
 ( #24577, #12184, #9342, #36972, #2248, #33927, #9139, #6082, #21331, #20932 ) ),
 .UNSPECIFIED., .F., .F., .F.,
 ( 2, 2 ),
 ( 4, 2, 2, 2, 4 ),
 ( 0.000000000000000000, 1.000000000000000000 ),
 ( 1.003840680322689360, 1.396539762021415498, 1.789238843720141414, 2.181937925418867330, 2.574637007117593246 ),
 .UNSPECIFIED. ) ;
#21672 = ORIENTED_EDGE ( 'NONE', *, *, #23020, .F. ) ;
#21673 = CARTESIAN_POINT ( 'NONE',  ( 0.5000000000000005551, 33.00000000000000000, 10.00000000000000000 ) ) ;
#21674 = CARTESIAN_POINT ( 'NONE',  ( -14.96192385577551853, -26.11888079852932876, -8.768824939043708966 ) ) ;
#21675 = CARTESIAN_POINT ( 'NONE',  ( -36.22115687806137174, -16.54570019420447835, 13.92931973827825409 ) ) ;
#21676 = VECTOR ( 'NONE', #22447, 1000.000000000000000 ) ;
#21677 = CARTESIAN_POINT ( 'NONE',  ( -29.86115101714491260, -23.36578077687985200, -5.861277548232656898 ) ) ;
#21678 = CARTESIAN_POINT ( 'NONE',  ( -2.597410653098545907, -24.79173595445318767, -5.482757586617159618 ) ) ;
#21680 = AXIS2_PLACEMENT_3D ( 'NONE', #3122, #18369, #34010 ) ;
#21679 = CARTESIAN_POINT ( 'NONE',  ( 11.95174086388698953, 18.65537474512603922, -22.77781173593105279 ) ) ;
#21681 = CARTESIAN_POINT ( 'NONE',  ( 22.68038563371576899, 10.11994014617707727, -7.424820902145242485 ) ) ;
#21682 = DIRECTION ( 'NONE',  ( -0.6293203910498342823, 0.7771459614569734553, 0.000000000000000000 ) ) ;
#21683 = CARTESIAN_POINT ( 'NONE',  ( -3.169894294691394165, 22.54309369389885020, -23.04265340177524735 ) ) ;
#21684 = ORIENTED_EDGE ( 'NONE', *, *, #9116, .F. ) ;
#21685 = CARTESIAN_POINT ( 'NONE',  ( -24.35958059579095902, -4.502232839367173334, -19.97906599432332087 ) ) ;
#21686 = AXIS2_PLACEMENT_3D ( 'NONE', #1571, #4817, #32041 ) ;
#21687 = CARTESIAN_POINT ( 'NONE',  ( -31.51573171626090897, 0.5582143012903738599, 15.13084544680213561 ) ) ;
#21688 = ORIENTED_EDGE ( 'NONE', *, *, #17692, .T. ) ;
#21689 = CARTESIAN_POINT ( 'NONE',  ( -3.610593701936585465, 31.83882289796395426, 10.00000000000000000 ) ) ;
#21690 = EDGE_CURVE ( 'NONE', #31599, #2452, #4226, .T. ) ;
#21691 = DIRECTION ( 'NONE',  ( 1.000000000000000000, 0.000000000000000000, 0.000000000000000000 ) ) ;
#21692 = ADVANCED_FACE ( 'NONE', ( #18783 ), #893, .F. ) ;
#21693 = CARTESIAN_POINT ( 'NONE',  ( -29.66265100694612045, 0.8681446443984893735, -7.834569626181125734 ) ) ;
#21694 = CARTESIAN_POINT ( 'NONE',  ( 35.42505292462669786, -13.05524145712385042, -5.438507544938067539 ) ) ;
#21695 = AXIS2_PLACEMENT_3D ( 'NONE', #2483, #34506, #37946 ) ;
#21696 = EDGE_LOOP ( 'NONE', ( #39862, #31122, #36071, #22516 ) ) ;
#21697 = DIRECTION ( 'NONE',  ( 1.000000000000000000, 0.000000000000000000, 0.000000000000000000 ) ) ;
#21698 = ORIENTED_EDGE ( 'NONE', *, *, #13303, .T. ) ;
#21699 = DIRECTION ( 'NONE',  ( -1.224646799147351235E-16, 1.000000000000000000, 0.000000000000000000 ) ) ;
#21700 = PLANE ( 'NONE',  #25319 ) ;
#21701 = AXIS2_PLACEMENT_3D ( 'NONE', #14831, #27218, #39804 ) ;
#21702 = FACE_OUTER_BOUND ( 'NONE', #13792, .T. ) ;
#21703 = ORIENTED_EDGE ( 'NONE', *, *, #21664, .F. ) ;
#21704 = CARTESIAN_POINT ( 'NONE',  ( -3.065405920905819759, 38.15199578371129263, -5.857520754517073769 ) ) ;
#21705 = DIRECTION ( 'NONE',  ( 0.9510565162951541973, 0.3090169943749456194, 0.000000000000000000 ) ) ;
#21706 = LINE ( 'NONE', #22105, #18901 ) ;
#21707 = EDGE_CURVE ( 'NONE', #7, #12173, #3534, .T. ) ;
#21708 = CARTESIAN_POINT ( 'NONE',  ( 25.46576935384675622, -20.87028045292102263, -12.93180561768287617 ) ) ;
#21709 = CARTESIAN_POINT ( 'NONE',  ( 15.86706096491193385, 13.22493649639811508, -27.13960584726105196 ) ) ;
#21710 = CARTESIAN_POINT ( 'NONE',  ( 12.57008845403963804, 30.17714168556475229, -9.943509663025896117 ) ) ;
#21711 = VECTOR ( 'NONE', #8564, 1000.000000000000114 ) ;
#21712 = EDGE_LOOP ( 'NONE', ( #19134, #21816, #225, #10830 ) ) ;
#21713 = CARTESIAN_POINT ( 'NONE',  ( -17.79840780512438769, 10.58908824627457257, -26.62318974669575056 ) ) ;
#21714 = CARTESIAN_POINT ( 'NONE',  ( 2.109373541296217347, 27.06550157850341876, 23.00000000000000000 ) ) ;
#21715 = CARTESIAN_POINT ( 'NONE',  ( 9.643767478264347659, -18.09000205506835712, -29.34533616503313525 ) ) ;
#21716 = DIRECTION ( 'NONE',  ( -0.000000000000000000, -0.000000000000000000, -1.000000000000000000 ) ) ;
#21717 = CARTESIAN_POINT ( 'NONE',  ( 37.49625565938770677, -14.69322820095495530, -14.45070082761205832 ) ) ;
#21718 = CARTESIAN_POINT ( 'NONE',  ( -3.784955426773657816, 9.502919080911416572, 10.00000000000000000 ) ) ;
#21719 = CARTESIAN_POINT ( 'NONE',  ( -15.27656269013936985, 26.57811910751880191, -7.356432126642811653 ) ) ;
#21720 = CARTESIAN_POINT ( 'NONE',  ( -23.88751137688053561, -26.63245304365073807, -5.447315017795344438 ) ) ;
#21721 = CARTESIAN_POINT ( 'NONE',  ( 8.584620562788320086, -18.61902014996657684, -29.36583904130536027 ) ) ;
#21722 = PLANE ( 'NONE',  #6250 ) ;
#21723 = ORIENTED_EDGE ( 'NONE', *, *, #37893, .T. ) ;
#21724 = CARTESIAN_POINT ( 'NONE',  ( -10.38219465376270101, 31.39154972851433101, -11.21545975099760817 ) ) ;
#21725 = CARTESIAN_POINT ( 'NONE',  ( 0.5000000000000000000, 37.09261900150649893, 10.99387790580546032 ) ) ;
#21726 = DIRECTION ( 'NONE',  ( 0.000000000000000000, 0.000000000000000000, 1.000000000000000000 ) ) ;
#21727 = CARTESIAN_POINT ( 'NONE',  ( -9.204968164644803608, 10.68109904802236798, 10.68306085400111449 ) ) ;
#21728 = EDGE_LOOP ( 'NONE', ( #34868, #14851, #1012, #20097 ) ) ;
#21729 = CARTESIAN_POINT ( 'NONE',  ( 20.48156205581511458, 0.8692611811187750392, -29.34855215404837381 ) ) ;
#21730 = DIRECTION ( 'NONE',  ( -0.5877852522924699175, 0.8090169943749498938, 0.000000000000000000 ) ) ;
#21731 = CARTESIAN_POINT ( 'NONE',  ( -10.44103466624267362, 32.57396620494226624, 9.500000000000000000 ) ) ;
#21732 = EDGE_CURVE ( 'NONE', #12299, #12248, #34162, .T. ) ;
#21733 = ORIENTED_EDGE ( 'NONE', *, *, #14080, .T. ) ;
#21734 = CARTESIAN_POINT ( 'NONE',  ( -20.52601294777450036, 0.8771626251181813272, -28.70764666120362918 ) ) ;
#21735 = CARTESIAN_POINT ( 'NONE',  ( 6.651296319737278750, 27.81603774131160023, 9.000000000000001776 ) ) ;
#21736 = ORIENTED_EDGE ( 'NONE', *, *, #24916, .T. ) ;
#21737 = CARTESIAN_POINT ( 'NONE',  ( 25.28008582448413222, -5.224672493644258786, -18.90502067835477717 ) ) ;
#21738 = AXIS2_PLACEMENT_3D ( 'NONE', #23507, #22895, #28998 ) ;
#21739 = VECTOR ( 'NONE', #21428, 1000.000000000000114 ) ;
#21740 = ORIENTED_EDGE ( 'NONE', *, *, #4565, .T. ) ;
#21741 = CARTESIAN_POINT ( 'NONE',  ( -13.65031603318048070, 34.08687889766149226, 12.73282698324877238 ) ) ;
#21742 = LINE ( 'NONE', #18708, #30073 ) ;
#21743 = DIRECTION ( 'NONE',  ( 1.000000000000000000, 0.000000000000000000, 0.000000000000000000 ) ) ;
#21744 = CARTESIAN_POINT ( 'NONE',  ( 9.535948996435982039, 27.56441102001909016, 19.99202127657104100 ) ) ;
#21745 = FACE_OUTER_BOUND ( 'NONE', #377, .T. ) ;
#21746 = VERTEX_POINT ( 'NONE', #34422 ) ;
#21747 = DIRECTION ( 'NONE',  ( 0.000000000000000000, 0.000000000000000000, 1.000000000000000000 ) ) ;
#21748 = CARTESIAN_POINT ( 'NONE',  ( -14.43694901005348719, 26.51279404187317468, 17.42190598798392642 ) ) ;
#21749 = CARTESIAN_POINT ( 'NONE',  ( -7.468455364333119739, 29.89744377950679421, 10.00000000000000000 ) ) ;
#21750 = CARTESIAN_POINT ( 'NONE',  ( 11.03640989728592281, 29.14264673470096767, 6.000000000000000000 ) ) ;
#21751 = ADVANCED_FACE ( 'NONE', ( #3729 ), #16132, .F. ) ;
#21752 = CARTESIAN_POINT ( 'NONE',  ( 5.158612383331919737, 20.07816763940033411, -27.79035459442517109 ) ) ;
#21753 = EDGE_CURVE ( 'NONE', #38096, #26836, #21829, .T. ) ;
#21754 = ADVANCED_FACE ( 'NONE', ( #18978 ), #29173, .T. ) ;
#21755 = CARTESIAN_POINT ( 'NONE',  ( 18.18730782112094246, -26.61009966856806130, -8.649289542032247979 ) ) ;
#21756 = DIRECTION ( 'NONE',  ( -0.3090169943749574988, -0.9510565162951503115, 0.000000000000000000 ) ) ;
#21757 = VECTOR ( 'NONE', #25503, 1000.000000000000000 ) ;
#21758 = CARTESIAN_POINT ( 'NONE',  ( 0.9685993473471133930, 37.46883198857096886, 7.338691926023209966 ) ) ;
#21759 = ORIENTED_EDGE ( 'NONE', *, *, #34725, .T. ) ;
#21760 = AXIS2_PLACEMENT_3D ( 'NONE', #20215, #38491, #26305 ) ;
#21761 = CARTESIAN_POINT ( 'NONE',  ( -14.64327399112337780, 24.66794574669921047, -11.60795671540694940 ) ) ;
#21762 = EDGE_CURVE ( 'NONE', #36822, #36487, #38266, .T. ) ;
#21763 = CIRCLE ( 'NONE', #8139, 0.5000000000000004441 ) ;
#21764 = CARTESIAN_POINT ( 'NONE',  ( -17.40362039086605250, -25.54020003774204639, 17.92354375535249034 ) ) ;
#21765 = CARTESIAN_POINT ( 'NONE',  ( 9.421039322076820710, -18.20697522973744498, -29.34992098691236251 ) ) ;
#21766 = CARTESIAN_POINT ( 'NONE',  ( -3.601976756503266763, 7.958898870085802990, 10.68306085400113048 ) ) ;
#21767 = ORIENTED_EDGE ( 'NONE', *, *, #29948, .F. ) ;
#21768 = EDGE_LOOP ( 'NONE', ( #11361, #11191, #27997, #15854 ) ) ;
#21769 = CARTESIAN_POINT ( 'NONE',  ( -13.74168852163965582, 30.17666712228406922, -7.268198090464257355 ) ) ;
#21770 = CARTESIAN_POINT ( 'NONE',  ( -19.54254085204202696, -25.96847084744576151, -9.956545142502918111 ) ) ;
#21771 = CARTESIAN_POINT ( 'NONE',  ( 10.09822582592851425, -27.41751403068707660, 11.00000000000204992 ) ) ;
#21772 = ORIENTED_EDGE ( 'NONE', *, *, #17641, .T. ) ;
#21773 = CARTESIAN_POINT ( 'NONE',  ( -35.11119181084233531, -9.814895828461905225, -7.164001942392926203 ) ) ;
#21774 = CARTESIAN_POINT ( 'NONE',  ( -9.700341350330687007, -18.60197822309132576, -26.23289683583976384 ) ) ;
#21775 = CARTESIAN_POINT ( 'NONE',  ( 13.93732035918235113, 28.04574148721571092, 7.339470489435498735 ) ) ;
#21776 = ORIENTED_EDGE ( 'NONE', *, *, #11156, .T. ) ;
#21777 = CARTESIAN_POINT ( 'NONE',  ( 20.47266963615838264, 1.058032431983775723, -29.35195464549815014 ) ) ;
#21778 = CARTESIAN_POINT ( 'NONE',  ( 4.817371740575539185, 23.83900317890011422, 20.99999999999999645 ) ) ;
#21779 = CARTESIAN_POINT ( 'NONE',  ( 19.48557158514982746, -11.25000000000009415, 2.999999999999999112 ) ) ;
#21780 = VERTEX_POINT ( 'NONE', #7375 ) ;
#21781 = ADVANCED_FACE ( 'NONE', ( #7785 ), #37321, .T. ) ;
#21782 = CARTESIAN_POINT ( 'NONE',  ( -28.93253131167843151, 0.05243184118532782240, -11.59459516453416583 ) ) ;
#21784 = EDGE_CURVE ( 'NONE', #21382, #17580, #14286, .T. ) ;
#21783 = ORIENTED_EDGE ( 'NONE', *, *, #11385, .F. ) ;
#21785 = CARTESIAN_POINT ( 'NONE',  ( 26.55368438709993129, -0.9046161187539608628, -16.29675340907314407 ) ) ;
#21786 = CARTESIAN_POINT ( 'NONE',  ( 24.37759566069541961, -10.08322588119077423, 21.00000000000001776 ) ) ;
#21787 = CARTESIAN_POINT ( 'NONE',  ( 33.27313359469018650, -17.33775975077022480, 17.42190598798393353 ) ) ;
#21788 = EDGE_LOOP ( 'NONE', ( #11198, #37021 ) ) ;
#21789 = CARTESIAN_POINT ( 'NONE',  ( -24.43781183141654623, 4.343050687655961362, -14.72646766136039176 ) ) ;
#21790 = VECTOR ( 'NONE', #5137, 1000.000000000000000 ) ;
#21791 = CARTESIAN_POINT ( 'NONE',  ( 24.58993327517434224, 16.11278406388105111, 7.000000000000000000 ) ) ;
#21792 = CYLINDRICAL_SURFACE ( 'NONE', #12840, 0.5000000000000001110 ) ;
#21793 = VECTOR ( 'NONE', #7060, 1000.000000000000000 ) ;
#21794 = CARTESIAN_POINT ( 'NONE',  ( 1.278175571583998194, 14.08178954835375940, 7.000000000000000000 ) ) ;
#21795 = VECTOR ( 'NONE', #35917, 1000.000000000000000 ) ;
#21796 = DIRECTION ( 'NONE',  ( -1.000000000000000000, 0.000000000000000000, 0.000000000000000000 ) ) ;
#21797 = EDGE_CURVE ( 'NONE', #2755, #19049, #26678, .T. ) ;
#21798 = EDGE_CURVE ( 'NONE', #3986, #14430, #23774, .T. ) ;
#21799 = DIRECTION ( 'NONE',  ( 0.000000000000000000, 0.000000000000000000, 1.000000000000000000 ) ) ;
#21800 = EDGE_CURVE ( 'NONE', #11758, #31065, #27657, .T. ) ;
#21801 = CARTESIAN_POINT ( 'NONE',  ( 15.48853125999101898, -26.74269726803731828, -5.000000000000000000 ) ) ;
#21802 = CARTESIAN_POINT ( 'NONE',  ( -19.65651305555018169, 6.423002548754848995, -27.12312071538742231 ) ) ;
#21803 = CARTESIAN_POINT ( 'NONE',  ( 2.672146553953307802, 12.33340603770389876, 11.00000000000000000 ) ) ;
#21804 = LINE ( 'NONE', #28100, #27887 ) ;
#21805 = CARTESIAN_POINT ( 'NONE',  ( 18.65140588264522137, -20.59310479824253548, -16.86763276178779591 ) ) ;
#21806 = DIRECTION ( 'NONE',  ( -0.3706816908110125985, -0.7275037805840900429, 0.5773502691896360561 ) ) ;
#21807 = CARTESIAN_POINT ( 'NONE',  ( 10.86259508579260746, 17.64226652144433771, -27.43142463228216599 ) ) ;
#21808 = ORIENTED_EDGE ( 'NONE', *, *, #13218, .T. ) ;
#21809 = CARTESIAN_POINT ( 'NONE',  ( -14.99023650920256756, 21.79341618737742792, -13.61763280836055934 ) ) ;
#21810 = EDGE_CURVE ( 'NONE', #19243, #6388, #24993, .T. ) ;
#21811 = CARTESIAN_POINT ( 'NONE',  ( -20.97603028425659843, -19.42790760331400790, 20.69868183039763565 ) ) ;
#21812 = DIRECTION ( 'NONE',  ( 1.000000000000000000, 0.000000000000000000, 0.000000000000000000 ) ) ;
#21813 = CARTESIAN_POINT ( 'NONE',  ( 14.75519950962563698, 25.34459079533402104, -10.65436177232459869 ) ) ;
#21814 = ORIENTED_EDGE ( 'NONE', *, *, #12137, .T. ) ;
#21815 = DIRECTION ( 'NONE',  ( 0.000000000000000000, 0.000000000000000000, 1.000000000000000000 ) ) ;
#21816 = ORIENTED_EDGE ( 'NONE', *, *, #16122, .F. ) ;
#21818 = DIRECTION ( 'NONE',  ( -0.3090169943749572767, -0.9510565162951503115, 0.000000000000000000 ) ) ;
#21817 = CARTESIAN_POINT ( 'NONE',  ( -13.91244456763262249, 24.21709252099823928, -13.48676834890144249 ) ) ;
#21819 = CARTESIAN_POINT ( 'NONE',  ( -15.12295902014546733, -26.02312468727843253, -9.231359056296803089 ) ) ;
#21820 = CARTESIAN_POINT ( 'NONE',  ( 12.51373512357659123, 14.69784138864569911, 10.94387467463329955 ) ) ;
#21821 = AXIS2_PLACEMENT_3D ( 'NONE', #24871, #37265, #31170 ) ;
#21822 = VERTEX_POINT ( 'NONE', #4335 ) ;
#21823 = CARTESIAN_POINT ( 'NONE',  ( -34.77349899548257639, -15.60207130184392987, -6.280198675005461695 ) ) ;
#21824 = CARTESIAN_POINT ( 'NONE',  ( -11.07034157884144854, -24.96936304302928988, -10.24950191894629370 ) ) ;
#21825 = DIRECTION ( 'NONE',  ( -0.000000000000000000, -0.000000000000000000, -1.000000000000000000 ) ) ;
#21826 = CARTESIAN_POINT ( 'NONE',  ( 12.38972167065434782, 16.33584955698245977, -29.37623187657347401 ) ) ;
#21827 = ORIENTED_EDGE ( 'NONE', *, *, #1889, .T. ) ;
#21828 = CARTESIAN_POINT ( 'NONE',  ( 19.85421419770838014, 5.208915335517238177, -28.81948969002354488 ) ) ;
#21829 = CIRCLE ( 'NONE', #17963, 0.4999999999999995559 ) ;
#21830 = DIRECTION ( 'NONE',  ( -1.000000000000000000, 0.000000000000000000, 0.000000000000000000 ) ) ;
#21831 = FACE_OUTER_BOUND ( 'NONE', #12647, .T. ) ;
#21832 = DIRECTION ( 'NONE',  ( 1.000000000000000000, 0.000000000000000000, 0.000000000000000000 ) ) ;
#21833 = VERTEX_POINT ( 'NONE', #35825 ) ;
#21834 = CARTESIAN_POINT ( 'NONE',  ( -23.55945276895399232, -0.1373144991472548537, -20.44794942058729603 ) ) ;
#21835 = ADVANCED_FACE ( 'NONE', ( #20189 ), #4540, .F. ) ;
#21836 = CARTESIAN_POINT ( 'NONE',  ( 26.00273584551220196, 0.08967249519437395233, -16.41428873911882746 ) ) ;
#21837 = CARTESIAN_POINT ( 'NONE',  ( -39.48557158816404211, -12.76940457902596471, 10.99999999999999645 ) ) ;
#21838 = CARTESIAN_POINT ( 'NONE',  ( 26.77583779507883222, -12.71777209950087340, 20.82122704794080903 ) ) ;
#21839 = ORIENTED_EDGE ( 'NONE', *, *, #1523, .T. ) ;
#21840 = CARTESIAN_POINT ( 'NONE',  ( -37.62663912510979003, -8.659558992827880886, -5.000000000000002665 ) ) ;
#21841 = CARTESIAN_POINT ( 'NONE',  ( 22.37674264578617667, 24.85189042352198641, 11.00000000000000000 ) ) ;
#21842 = ORIENTED_EDGE ( 'NONE', *, *, #29360, .F. ) ;
#21843 = DIRECTION ( 'NONE',  ( -0.5877852522924797984, -0.8090169943749425663, 0.000000000000000000 ) ) ;
#21844 = AXIS2_PLACEMENT_3D ( 'NONE', #12885, #33844, #22222 ) ;
#21845 = AXIS2_PLACEMENT_3D ( 'NONE', #28822, #29625, #35321 ) ;
#21846 = DIRECTION ( 'NONE',  ( -0.000000000000000000, -0.000000000000000000, 1.000000000000000000 ) ) ;
#21847 = DIRECTION ( 'NONE',  ( 1.000000000000000000, 0.000000000000000000, 0.000000000000000000 ) ) ;
#21848 = CARTESIAN_POINT ( 'NONE',  ( 1.512454924012853974, 21.38568066047234950, -25.58676729699224239 ) ) ;
#21849 = EDGE_CURVE ( 'NONE', #19377, #38413, #13475, .T. ) ;
#21850 = CARTESIAN_POINT ( 'NONE',  ( 14.97009266215792778, 21.42933399866929634, 10.63089969389956480 ) ) ;
#21851 = DIRECTION ( 'NONE',  ( 0.9781476007338072431, 0.2079116908177516265, 0.000000000000000000 ) ) ;
#21852 = CARTESIAN_POINT ( 'NONE',  ( 8.577540944421576441, 33.15743037285414374, 13.00000000000000178 ) ) ;
#21853 = B_SPLINE_CURVE_WITH_KNOTS ( 'NONE', 3,
 ( #4672, #22746, #19504, #38800, #29052, #23364 ),
 .UNSPECIFIED., .F., .F.,
 ( 4, 2, 4 ),
 ( 0.000000000000000000, 0.5000000000000000000, 1.000000000000000000 ),
 .UNSPECIFIED. ) ;
#21854 = LINE ( 'NONE', #18818, #24476 ) ;
#21855 = CARTESIAN_POINT ( 'NONE',  ( -7.470035553104361625, 44.81454624109330354, 7.000000000000000000 ) ) ;
#21856 = DIRECTION ( 'NONE',  ( 0.000000000000000000, 0.000000000000000000, 1.000000000000000000 ) ) ;
#21857 = CARTESIAN_POINT ( 'NONE',  ( 12.69411822000453327, 23.12755374673593423, -16.33488331723920339 ) ) ;
#21858 = DIRECTION ( 'NONE',  ( 0.000000000000000000, 0.000000000000000000, 1.000000000000000000 ) ) ;
#21859 = VERTEX_POINT ( 'NONE', #11244 ) ;
#21861 = DIRECTION ( 'NONE',  ( -0.2588190451025293437, -0.9659258262890660918, 0.000000000000000000 ) ) ;
#21860 = CARTESIAN_POINT ( 'NONE',  ( -18.70298414372253148, 17.62570364501429410, -6.443206386152125376 ) ) ;
#21862 = CARTESIAN_POINT ( 'NONE',  ( -13.33727129354594609, 15.63559704646376147, 7.470097061328788257 ) ) ;
#21863 = CARTESIAN_POINT ( 'NONE',  ( 15.17726020569047130, -26.28321538289182513, -8.297710205149746443 ) ) ;
#21864 = CARTESIAN_POINT ( 'NONE',  ( -14.51034690954441153, -19.54383024884274533, -20.13759940615653221 ) ) ;
#21865 = CARTESIAN_POINT ( 'NONE',  ( 10.98647152928294979, 17.30743895948372568, -30.00000000000000711 ) ) ;
#21866 = CARTESIAN_POINT ( 'NONE',  ( 11.05510453204928289, 17.51453838611892522, -27.44640421723807222 ) ) ;
#21867 = ORIENTED_EDGE ( 'NONE', *, *, #36950, .T. ) ;
#21868 = DIRECTION ( 'NONE',  ( -0.000000000000000000, -0.000000000000000000, -1.000000000000000000 ) ) ;
#21869 = CARTESIAN_POINT ( 'NONE',  ( -12.58328644382519990, -22.55677566891993280, -16.44928081634269645 ) ) ;
#21870 = CARTESIAN_POINT ( 'NONE',  ( -16.99774364072496979, -28.32416636927843001, 14.53008259253979517 ) ) ;
#21871 = CARTESIAN_POINT ( 'NONE',  ( -23.88592270937412110, -16.48473916716029919, -16.63925841098920699 ) ) ;
#21872 = CARTESIAN_POINT ( 'NONE',  ( -0.3897205959626180993, -24.77793770357540737, -5.482964004482600906 ) ) ;
#21873 = CARTESIAN_POINT ( 'NONE',  ( 15.56814849921199695, 26.15651636719908879, -5.946228235075683877 ) ) ;
#21874 = CARTESIAN_POINT ( 'NONE',  ( 21.01520796838052618, 9.533611945060952664, -15.93287469514982924 ) ) ;
#21875 = LINE ( 'NONE', #30835, #17353 ) ;
#21876 = ORIENTED_EDGE ( 'NONE', *, *, #26893, .T. ) ;
#21877 = CARTESIAN_POINT ( 'NONE',  ( -20.82306015624319073, -2.481982540487905897, -26.57961284343121733 ) ) ;
#21878 = VECTOR ( 'NONE', #31327, 1000.000000000000000 ) ;
#21879 = AXIS2_PLACEMENT_3D ( 'NONE', #5246, #18050, #2208 ) ;
#21880 = CARTESIAN_POINT ( 'NONE',  ( -22.19651343352304806, 6.568638172588403989, 18.42518152272124965 ) ) ;
#21881 = EDGE_LOOP ( 'NONE', ( #10165, #33282, #23360, #39455, #24824 ) ) ;
#21882 = CARTESIAN_POINT ( 'NONE',  ( 2.164762040630750395, 7.656889776559952843, 7.338691926023207301 ) ) ;
#21883 = EDGE_CURVE ( 'NONE', #19145, #30411, #35215, .T. ) ;
#21884 = FACE_OUTER_BOUND ( 'NONE', #29935, .T. ) ;
#21885 = EDGE_CURVE ( 'NONE', #25935, #5003, #35379, .T. ) ;
#21886 = AXIS2_PLACEMENT_3D ( 'NONE', #31581, #10454, #10053 ) ;
#21887 = CARTESIAN_POINT ( 'NONE',  ( -29.86441318786370047, 0.6479988441763335771, -7.832743955948457071 ) ) ;
#21888 = CARTESIAN_POINT ( 'NONE',  ( 33.65435358744935712, -12.34966631407584003, -9.758582659885652433 ) ) ;
#21889 = CARTESIAN_POINT ( 'NONE',  ( 16.95459465864674442, -28.62006465032575164, 13.92931973827687919 ) ) ;
#21890 = ORIENTED_EDGE ( 'NONE', *, *, #32615, .T. ) ;
#21891 = DIRECTION ( 'NONE',  ( -0.9945218953682742891, -0.1045284632676437425, 0.000000000000000000 ) ) ;
#21892 = ORIENTED_EDGE ( 'NONE', *, *, #13164, .F. ) ;
#21893 = ADVANCED_FACE ( 'NONE', ( #32789, #32994 ), #17351, .F. ) ;
#21894 = CARTESIAN_POINT ( 'NONE',  ( 8.412270287199559604, 10.07085245822950981, 10.49999999999999822 ) ) ;
#21895 = LINE ( 'NONE', #25340, #18288 ) ;
#21896 = CARTESIAN_POINT ( 'NONE',  ( 3.494936919103933448, 34.23777120880591696, 12.00000000000000000 ) ) ;
#21897 = ORIENTED_EDGE ( 'NONE', *, *, #33979, .F. ) ;
#21898 = CARTESIAN_POINT ( 'NONE',  ( -3.054091535875387731, 37.95567441806279163, -6.700395517222553998 ) ) ;
#21899 = CARTESIAN_POINT ( 'NONE',  ( 8.380596568873530217, 10.11444759148754535, 10.76099332938164288 ) ) ;
#21900 = DIRECTION ( 'NONE',  ( 0.3090169943749450643, -0.9510565162951544194, 0.000000000000000000 ) ) ;
#21901 = FACE_OUTER_BOUND ( 'NONE', #14348, .T. ) ;
#21902 = DIRECTION ( 'NONE',  ( 0.000000000000000000, 0.000000000000000000, 1.000000000000000000 ) ) ;
#21903 = LINE ( 'NONE', #12960, #28139 ) ;
#21904 = CARTESIAN_POINT ( 'NONE',  ( 13.55441085756498154, 30.31521231272209604, -7.712462757402486879 ) ) ;
#21905 = VECTOR ( 'NONE', #27928, 1000.000000000000000 ) ;
#21906 = ORIENTED_EDGE ( 'NONE', *, *, #19798, .T. ) ;
#21907 = CARTESIAN_POINT ( 'NONE',  ( -20.65769276629826479, 11.18138066491571614, -13.90382682998711417 ) ) ;
#21908 = CARTESIAN_POINT ( 'NONE',  ( 19.26948696230205016, 27.85601271560038228, 11.00000000000000000 ) ) ;
#21909 = EDGE_CURVE ( 'NONE', #32296, #29828, #38669, .T. ) ;
#21910 = CARTESIAN_POINT ( 'NONE',  ( 15.51551714807790994, -26.62543040642743364, -6.885114030514080774 ) ) ;
#21911 = CARTESIAN_POINT ( 'NONE',  ( -14.81329996725647469, 19.93755115561707569, 7.000000000000000000 ) ) ;
#21912 = CARTESIAN_POINT ( 'NONE',  ( 15.34541588040626792, 26.76641394790292239, -6.415693964850016862 ) ) ;
#21913 = VECTOR ( 'NONE', #17870, 1000.000000000000000 ) ;
#21914 = CARTESIAN_POINT ( 'NONE',  ( 26.31271763591406909, -28.25584584496056451, -14.26382729546506667 ) ) ;
#21915 = DIRECTION ( 'NONE',  ( 1.000000000000000000, 0.000000000000000000, 0.000000000000000000 ) ) ;
#21916 = CIRCLE ( 'NONE', #4410, 1.000000000000002665 ) ;
#21917 = CARTESIAN_POINT ( 'NONE',  ( -14.82594730225876312, 25.65344611243898498, -10.17754751450732265 ) ) ;
#21918 = CARTESIAN_POINT ( 'NONE',  ( -26.03722647915365584, -25.89241862741840094, -5.000000000000004441 ) ) ;
#21919 = CARTESIAN_POINT ( 'NONE',  ( 8.275334808801511954, -21.38839901459642334, -19.81352468994020910 ) ) ;
#21920 = CARTESIAN_POINT ( 'NONE',  ( 14.33783055764683745, 24.35298217862673198, -12.55492370899574972 ) ) ;
#21921 = CARTESIAN_POINT ( 'NONE',  ( 24.02681206829297977, -16.26566910256974552, -16.63819982037562184 ) ) ;
#21922 = FACE_OUTER_BOUND ( 'NONE', #12279, .T. ) ;
#21923 = ORIENTED_EDGE ( 'NONE', *, *, #35923, .F. ) ;
#21924 = CARTESIAN_POINT ( 'NONE',  ( -10.27371142776379820, 34.65346829918823346, -6.313534688996303323 ) ) ;
#21925 = CARTESIAN_POINT ( 'NONE',  ( -14.58123527826107590, 20.01612550765336707, 10.49999999999999822 ) ) ;
#21926 = DIRECTION ( 'NONE',  ( -0.000000000000000000, -0.000000000000000000, -1.000000000000000000 ) ) ;
#21927 = CARTESIAN_POINT ( 'NONE',  ( 14.81329996725643738, 19.93755115561686964, 10.50000000000000533 ) ) ;
#21928 = ORIENTED_EDGE ( 'NONE', *, *, #21510, .T. ) ;
#21929 = CARTESIAN_POINT ( 'NONE',  ( 30.75739384342617555, 0.004716038886164508614, -6.417043594193787115 ) ) ;
#21930 = CARTESIAN_POINT ( 'NONE',  ( 14.47283171447379502, 21.48159823030311344, 7.500000000000010658 ) ) ;
#21931 = EDGE_CURVE ( 'NONE', #31871, #13187, #29527, .T. ) ;
#21932 = DIRECTION ( 'NONE',  ( 0.000000000000000000, -0.000000000000000000, -1.000000000000000000 ) ) ;
#21933 = ORIENTED_EDGE ( 'NONE', *, *, #28970, .T. ) ;
#21934 = CARTESIAN_POINT ( 'NONE',  ( -20.52549850993021607, 0.8876484853251380702, -28.70801360605462094 ) ) ;
#21935 = EDGE_CURVE ( 'NONE', #25837, #39356, #9807, .T. ) ;
#21936 = LINE ( 'NONE', #6098, #6643 ) ;
#21937 = ORIENTED_EDGE ( 'NONE', *, *, #6314, .T. ) ;
#21938 = CARTESIAN_POINT ( 'NONE',  ( 20.21125490546006276, -3.489748019849370220, -29.99999999999998579 ) ) ;
#21939 = AXIS2_PLACEMENT_3D ( 'NONE', #27791, #30648, #24735 ) ;
#21940 = AXIS2_PLACEMENT_3D ( 'NONE', #33002, #14699, #20996 ) ;
#21941 = EDGE_CURVE ( 'NONE', #9948, #20919, #6254, .T. ) ;
#21942 = EDGE_LOOP ( 'NONE', ( #18254, #23102, #5216, #729, #33359, #32733, #31482, #7829 ) ) ;
#21943 = CARTESIAN_POINT ( 'NONE',  ( 13.75541765477348655, 34.17602237659296094, 12.14047268033109184 ) ) ;
#21944 = ADVANCED_FACE ( 'NONE', ( #12235 ), #11446, .F. ) ;
#21945 = CIRCLE ( 'NONE', #30407, 15.00000000000000000 ) ;
#21946 = FACE_OUTER_BOUND ( 'NONE', #29108, .T. ) ;
#21947 = LINE ( 'NONE', #34349, #6580 ) ;
#21948 = CARTESIAN_POINT ( 'NONE',  ( -9.417362331747755277, 30.49429905890304937, 19.27171037444153612 ) ) ;
#21949 = AXIS2_PLACEMENT_3D ( 'NONE', #38779, #13387, #16651 ) ;
#21950 = FACE_OUTER_BOUND ( 'NONE', #1382, .T. ) ;
#21951 = ORIENTED_EDGE ( 'NONE', *, *, #28700, .F. ) ;
#21952 = CARTESIAN_POINT ( 'NONE',  ( 3.607749162633208329, 7.931741834401768720, 10.59344459855565468 ) ) ;
#21953 = CARTESIAN_POINT ( 'NONE',  ( -19.08133911595188437, 7.519478901772812307, -29.99999999999999645 ) ) ;
#21954 = DIRECTION ( 'NONE',  ( -0.000000000000000000, -0.000000000000000000, -1.000000000000000000 ) ) ;
#21955 = CARTESIAN_POINT ( 'NONE',  ( 12.17073081513896327, 14.31852474926571972, 10.49999999999999822 ) ) ;
#21956 = CARTESIAN_POINT ( 'NONE',  ( 18.04900360418865546, 18.86275876442724453, -7.401912832897363792 ) ) ;
#21957 = CARTESIAN_POINT ( 'NONE',  ( 9.059065324806985231, 35.31177540401563419, -7.163937956742758573 ) ) ;
#21958 = EDGE_CURVE ( 'NONE', #19274, #35202, #20988, .T. ) ;
#21959 = EDGE_CURVE ( 'NONE', #16687, #31932, #7558, .T. ) ;
#21960 = CARTESIAN_POINT ( 'NONE',  ( 17.41134420666527660, -26.92035120749303445, -7.305176101613050754 ) ) ;
#21961 = DIRECTION ( 'NONE',  ( 0.000000000000000000, 0.000000000000000000, 1.000000000000000000 ) ) ;
#21962 = DIRECTION ( 'NONE',  ( 0.000000000000000000, 0.000000000000000000, 1.000000000000000000 ) ) ;
#21963 = B_SPLINE_CURVE_WITH_KNOTS ( 'NONE', 3,
 ( #37643, #21998, #12454, #3511 ),
 .UNSPECIFIED., .F., .F.,
 ( 4, 4 ),
 ( 0.000000000000000000, 0.1234515740337736034 ),
 .UNSPECIFIED. ) ;
#21964 = CIRCLE ( 'NONE', #24583, 6.000000000000000888 ) ;
#21965 = ORIENTED_EDGE ( 'NONE', *, *, #24369, .F. ) ;
#21967 = AXIS2_PLACEMENT_3D ( 'NONE', #6859, #778, #25953 ) ;
#21966 = CARTESIAN_POINT ( 'NONE',  ( -11.23742582611742513, 17.39156283123631752, -27.46051757209724897 ) ) ;
#21968 = CARTESIAN_POINT ( 'NONE',  ( -23.60877407455476984, -25.08990816560874038, 17.92354375535287403 ) ) ;
#21969 = CARTESIAN_POINT ( 'NONE',  ( 11.80044851807104678, -21.49314593586473876, -18.46258872189030242 ) ) ;
#21970 = CARTESIAN_POINT ( 'NONE',  ( 6.354454053420411697, 35.54304081427980577, 9.000000000000001776 ) ) ;
#21971 = VERTEX_POINT ( 'NONE', #5936 ) ;
#21972 = ORIENTED_EDGE ( 'NONE', *, *, #18736, .F. ) ;
#21973 = CARTESIAN_POINT ( 'NONE',  ( -13.92122689940795510, 28.37753238768550190, -9.577933452506133705 ) ) ;
#21974 = CARTESIAN_POINT ( 'NONE',  ( -11.08653240243507554, -17.32279251903801409, -28.64327423991444377 ) ) ;
#21975 = FACE_BOUND ( 'NONE', #5498, .T. ) ;
#21976 = EDGE_LOOP ( 'NONE', ( #11602, #18458, #39876, #13723 ) ) ;
#21977 = CARTESIAN_POINT ( 'NONE',  ( -26.20239787803879850, -7.299429199793270762, -17.76499887194331961 ) ) ;
#21978 = CARTESIAN_POINT ( 'NONE',  ( -9.394881763177457046, -18.22048488343288142, -29.35045134641008957 ) ) ;
#21979 = DIRECTION ( 'NONE',  ( -0.000000000000000000, -0.000000000000000000, 1.000000000000000000 ) ) ;
#21980 = ORIENTED_EDGE ( 'NONE', *, *, #37446, .F. ) ;
#21981 = CARTESIAN_POINT ( 'NONE',  ( 20.67958368883273224, 1.036419229453801050, -27.46041608859013650 ) ) ;
#21982 = DIRECTION ( 'NONE',  ( -0.000000000000000000, -0.000000000000000000, 1.000000000000000000 ) ) ;
#21983 = DIRECTION ( 'NONE',  ( -1.000000000000000000, 0.000000000000000000, 0.000000000000000000 ) ) ;
#21984 = ORIENTED_EDGE ( 'NONE', *, *, #17735, .F. ) ;
#21985 = CARTESIAN_POINT ( 'NONE',  ( -20.52899626704462932, 0.8142514703770860063, -28.70543900254816805 ) ) ;
#21986 = EDGE_CURVE ( 'NONE', #29585, #35629, #17551, .T. ) ;
#21987 = ORIENTED_EDGE ( 'NONE', *, *, #37902, .F. ) ;
#21988 = CARTESIAN_POINT ( 'NONE',  ( 20.88948691698688265, -0.6490584520769514532, -26.71535767925633564 ) ) ;
#21989 = CARTESIAN_POINT ( 'NONE',  ( 15.27779781845867468, -13.73655938454271030, -29.99999999999999645 ) ) ;
#21990 = CARTESIAN_POINT ( 'NONE',  ( 31.36686156446545581, -22.11446460981255058, 16.30093088680227709 ) ) ;
#21991 = ORIENTED_EDGE ( 'NONE', *, *, #31621, .T. ) ;
#21992 = CARTESIAN_POINT ( 'NONE',  ( -26.64229111171870912, 4.405581445021985232, -7.868447511081861911 ) ) ;
#21993 = EDGE_CURVE ( 'NONE', #12248, #19728, #2106, .T. ) ;
#21994 = CARTESIAN_POINT ( 'NONE',  ( -14.54089481611321055, 26.18321485943229376, 7.323837789871779691 ) ) ;
#21995 = DIRECTION ( 'NONE',  ( 0.000000000000000000, 0.000000000000000000, 1.000000000000000000 ) ) ;
#21996 = VECTOR ( 'NONE', #39451, 1000.000000000000000 ) ;
#21997 = VECTOR ( 'NONE', #36312, 1000.000000000000000 ) ;
#21998 = CARTESIAN_POINT ( 'NONE',  ( -17.14571668001621418, -27.17024302301528849, -4.999999999999999112 ) ) ;
#21999 = FACE_OUTER_BOUND ( 'NONE', #4245, .T. ) ;
#22000 = VECTOR ( 'NONE', #35954, 1000.000000000000000 ) ;
#22001 = PRODUCT_DEFINITION_SHAPE ( 'NONE', 'NONE',  #27397 ) ;
#22002 = FACE_BOUND ( 'NONE', #29245, .T. ) ;
#22003 = CARTESIAN_POINT ( 'NONE',  ( 25.43795106045698518, 8.821996438889113890, 13.32518128616659148 ) ) ;
#22004 = CARTESIAN_POINT ( 'NONE',  ( -19.80772954507643391, 5.710854581715417488, -27.67139024716352225 ) ) ;
#22005 = LINE ( 'NONE', #25054, #35216 ) ;
#22006 = DIRECTION ( 'NONE',  ( 0.000000000000000000, 0.000000000000000000, 1.000000000000000000 ) ) ;
#22007 = CARTESIAN_POINT ( 'NONE',  ( 19.29622809070872691, -21.30767804701306289, -15.90023521376778604 ) ) ;
#22008 = CARTESIAN_POINT ( 'NONE',  ( -5.458872323573595864, 26.51478363815348160, 13.00000000000000178 ) ) ;
#22009 = EDGE_CURVE ( 'NONE', #4170, #18302, #12028, .T. ) ;
#22010 = CARTESIAN_POINT ( 'NONE',  ( 15.27493397812733988, 27.00603829493833175, -6.411867504281748786 ) ) ;
#22011 = ORIENTED_EDGE ( 'NONE', *, *, #3954, .F. ) ;
#22012 = CARTESIAN_POINT ( 'NONE',  ( -12.27438659830399104, 16.41897796854597047, -30.00000000000000000 ) ) ;
#22013 = CARTESIAN_POINT ( 'NONE',  ( -27.85940672053882849, -14.94704994757599081, 20.50957957746051719 ) ) ;
#22014 = CARTESIAN_POINT ( 'NONE',  ( -19.48557158514998022, -11.24999999999982414, 2.999999999999999112 ) ) ;
#22015 = CARTESIAN_POINT ( 'NONE',  ( 11.72000814234884025, 18.87896920474838680, -22.74070836927191053 ) ) ;
#22016 = EDGE_LOOP ( 'NONE', ( #22550, #21698, #12033, #30091 ) ) ;
#22017 = CARTESIAN_POINT ( 'NONE',  ( -14.23945615837876311, -31.58416516429889853, 0.000000000000000000 ) ) ;
#22018 = ORIENTED_EDGE ( 'NONE', *, *, #23183, .F. ) ;
#22020 = DIRECTION ( 'NONE',  ( 0.000000000000000000, 0.000000000000000000, 1.000000000000000000 ) ) ;
#22019 = CARTESIAN_POINT ( 'NONE',  ( -14.17779301840820239, 24.76684511783872011, -12.52556781375514738 ) ) ;
#22021 = CARTESIAN_POINT ( 'NONE',  ( -15.29280108727264853, -26.19529837291199215, -8.758642717996806937 ) ) ;
#22022 = CARTESIAN_POINT ( 'NONE',  ( 12.14063985594365924, 14.34296697341676641, 10.49999999999999822 ) ) ;
#22023 = AXIS2_PLACEMENT_3D ( 'NONE', #17180, #38088, #32204 ) ;
#22024 = ORIENTED_EDGE ( 'NONE', *, *, #18311, .T. ) ;
#22025 = CARTESIAN_POINT ( 'NONE',  ( -33.98065044953765579, -15.22623518443444901, -8.413853775630943943 ) ) ;
#22026 = CARTESIAN_POINT ( 'NONE',  ( -13.97107818215439146, -25.64569743057662166, -9.722743490932185040 ) ) ;
#22027 = DIRECTION ( 'NONE',  ( -1.000000000000000000, 0.000000000000000000, 0.000000000000000000 ) ) ;
#22028 = CARTESIAN_POINT ( 'NONE',  ( 16.38359496941714966, 23.11600525820518115, -7.374208509789634824 ) ) ;
#22029 = VERTEX_POINT ( 'NONE', #21185 ) ;
#22030 = CARTESIAN_POINT ( 'NONE',  ( 25.86526715380574259, 4.645913844102615542, -10.29163244528595200 ) ) ;
#22031 = DIRECTION ( 'NONE',  ( -1.000000000000000000, 0.000000000000000000, 0.000000000000000000 ) ) ;
#22032 = CARTESIAN_POINT ( 'NONE',  ( -11.16521142134453726, 24.66068167190384841, 13.00000000000000178 ) ) ;
#22033 = CARTESIAN_POINT ( 'NONE',  ( -0.5000000000000004441, 37.00000000000000711, 7.000000000000000000 ) ) ;
#22034 = VECTOR ( 'NONE', #3613, 1000.000000000000114 ) ;
#22035 = ORIENTED_EDGE ( 'NONE', *, *, #3242, .F. ) ;
#22036 = CARTESIAN_POINT ( 'NONE',  ( -30.84242166733599788, -0.3958891573209706860, -7.811368989421731079 ) ) ;
#22037 = EDGE_CURVE ( 'NONE', #31380, #8749, #17039, .T. ) ;
#22038 = CARTESIAN_POINT ( 'NONE',  ( 20.61837044269047681, 0.7085719058875546983, -28.07041881223954860 ) ) ;
#22039 = EDGE_CURVE ( 'NONE', #5579, #28502, #39289, .T. ) ;
#22040 = CARTESIAN_POINT ( 'NONE',  ( 27.57147631791876918, -9.321847555861369372, 20.69868183039781329 ) ) ;
#22041 = VERTEX_POINT ( 'NONE', #39470 ) ;
#22042 = CARTESIAN_POINT ( 'NONE',  ( 12.33616729053617966, -27.99489201236593416, -5.000000000000000000 ) ) ;
#22043 = CARTESIAN_POINT ( 'NONE',  ( 4.577399223880713741, 35.23960032125091146, 9.500000000000000000 ) ) ;
#22044 = EDGE_CURVE ( 'NONE', #24787, #24416, #4255, .T. ) ;
#22045 = VERTEX_POINT ( 'NONE', #27473 ) ;
#22046 = DIRECTION ( 'NONE',  ( 0.8090169943749421222, -0.5877852522924804646, 0.000000000000000000 ) ) ;
#22047 = CARTESIAN_POINT ( 'NONE',  ( -0.5000000000000004441, 37.00000000000000711, 7.000000000000000000 ) ) ;
#22048 = CARTESIAN_POINT ( 'NONE',  ( -14.86556419889029534, 20.43481210330121556, 7.000000000000000000 ) ) ;
#22049 = CARTESIAN_POINT ( 'NONE',  ( 3.810525450730533947, 37.24451434163790253, -7.981115972861925201 ) ) ;
#22050 = DIRECTION ( 'NONE',  ( 0.6459741880212479526, 0.2876062384759398016, 0.7071067811865549002 ) ) ;
#22051 = DIRECTION ( 'NONE',  ( 0.4067366430758010409, 0.9135454576426005335, -0.000000000000000000 ) ) ;
#22052 = CARTESIAN_POINT ( 'NONE',  ( -14.01838097023000707, 23.73363068877903359, 13.00000000000000178 ) ) ;
#22053 = AXIS2_PLACEMENT_3D ( 'NONE', #171, #24951, #34500 ) ;
#22054 = EDGE_CURVE ( 'NONE', #15741, #10198, #11399, .T. ) ;
#22055 = PLANE ( 'NONE',  #2417 ) ;
#22056 = DIRECTION ( 'NONE',  ( 0.7431448254773953543, 0.6691306063588570163, 0.000000000000000000 ) ) ;
#22057 = DIRECTION ( 'NONE',  ( -0.000000000000000000, -0.000000000000000000, -1.000000000000000000 ) ) ;
#22058 = EDGE_CURVE ( 'NONE', #6246, #16446, #2505, .T. ) ;
#22059 = CARTESIAN_POINT ( 'NONE',  ( 15.00330998323748055, 28.06465100738194351, -4.999999999999998224 ) ) ;
#22060 = CARTESIAN_POINT ( 'NONE',  ( -2.036571916123810055, 8.108948098542073879, 10.50000000000000355 ) ) ;
#22061 = ORIENTED_EDGE ( 'NONE', *, *, #14052, .T. ) ;
#22063 = FACE_OUTER_BOUND ( 'NONE', #33639, .T. ) ;
#22062 = CARTESIAN_POINT ( 'NONE',  ( -18.09385140116044965, 18.44421545049425504, -8.373696076410258371 ) ) ;
#22064 = CARTESIAN_POINT ( 'NONE',  ( -13.28503138821885798, 15.53523575316151195, 7.499999999999993783 ) ) ;
#22065 = CARTESIAN_POINT ( 'NONE',  ( 9.486164890912217373, -18.17313361576023212, -29.34858962865161303 ) ) ;
#22066 = CARTESIAN_POINT ( 'NONE',  ( -20.92342021452639855, -26.27463686021861378, -9.014949617875791077 ) ) ;
#22067 = CARTESIAN_POINT ( 'NONE',  ( 15.17557291600564362, 26.27770503188184037, -8.298014751482952533 ) ) ;
#22068 = CARTESIAN_POINT ( 'NONE',  ( 12.38369262076488475, 20.50029293666852226, -19.49479296581450427 ) ) ;
#22069 = ORIENTED_EDGE ( 'NONE', *, *, #4519, .F. ) ;
#22070 = CARTESIAN_POINT ( 'NONE',  ( -33.75875814100331951, 2.759858869446532470, 23.00000000000000000 ) ) ;
#22071 = CARTESIAN_POINT ( 'NONE',  ( -9.648264831776160122, -18.46096267954140657, -26.83400085027493986 ) ) ;
#22072 = CARTESIAN_POINT ( 'NONE',  ( -18.85754271145797034, -29.00601859117224990, 13.32518128616650799 ) ) ;
#22073 = CIRCLE ( 'NONE', #2622, 1.000000000000000000 ) ;
#22074 = CARTESIAN_POINT ( 'NONE',  ( -19.84140702193834827, -14.57578147485350506, -20.72667381623678651 ) ) ;
#22075 = CARTESIAN_POINT ( 'NONE',  ( -2.250492809306957387, -22.96836341133687753, -15.94180792882460018 ) ) ;
#22076 = CARTESIAN_POINT ( 'NONE',  ( 14.19245098026133967, 22.50397599124407932, -14.52977076431803560 ) ) ;
#22077 = ORIENTED_EDGE ( 'NONE', *, *, #24968, .F. ) ;
#22078 = CARTESIAN_POINT ( 'NONE',  ( 18.70205627895097678, 9.558498540185201620, -24.40894002729765688 ) ) ;
#22079 = DIRECTION ( 'NONE',  ( 0.5877852522924689183, -0.8090169943749505599, -0.000000000000000000 ) ) ;
#22080 = CARTESIAN_POINT ( 'NONE',  ( -6.055828121133336239, 35.60995051739008943, 17.92354375535250810 ) ) ;
#22081 = B_SPLINE_CURVE_WITH_KNOTS ( 'NONE', 3,
 ( #39959, #12135, #24523, #34074 ),
 .UNSPECIFIED., .F., .F.,
 ( 4, 4 ),
 ( 0.8666666404939821211, 1.000000000000000000 ),
 .UNSPECIFIED. ) ;
#22082 = ORIENTED_EDGE ( 'NONE', *, *, #35406, .T. ) ;
#22083 = CARTESIAN_POINT ( 'NONE',  ( -22.73893131577041871, -2.785302627231514006, -22.32846206850632598 ) ) ;
#22084 = EDGE_CURVE ( 'NONE', #17936, #1570, #17756, .T. ) ;
#22085 = CARTESIAN_POINT ( 'NONE',  ( -13.83280510892634929, 26.34487040056601970, 17.92354375535250810 ) ) ;
#22086 = VERTEX_POINT ( 'NONE', #11649 ) ;
#22087 = EDGE_CURVE ( 'NONE', #32396, #39920, #36236, .T. ) ;
#22088 = CARTESIAN_POINT ( 'NONE',  ( 8.368303251206119953, 20.48707633493483371, 9.000000000000001776 ) ) ;
#22089 = FACE_OUTER_BOUND ( 'NONE', #444, .T. ) ;
#22090 = AXIS2_PLACEMENT_3D ( 'NONE', #30608, #18616, #39738 ) ;
#22091 = CARTESIAN_POINT ( 'NONE',  ( -21.60728915618764390, 1.248469937430795262, -23.91367510233994764 ) ) ;
#22092 = CARTESIAN_POINT ( 'NONE',  ( 19.81193986357125425, -7.322314881371388751, -26.31558243123959073 ) ) ;
#22093 = CARTESIAN_POINT ( 'NONE',  ( 26.32119069355270113, -27.53777429989680670, 13.32518128616608521 ) ) ;
#22094 = ORIENTED_EDGE ( 'NONE', *, *, #24508, .F. ) ;
#22095 = CARTESIAN_POINT ( 'NONE',  ( -12.23327497914565853, 13.81973598992469121, 7.000000000000000000 ) ) ;
#22096 = VERTEX_POINT ( 'NONE', #8398 ) ;
#22097 = DIRECTION ( 'NONE',  ( -0.5877852522924797984, -0.8090169943749426773, 0.000000000000000000 ) ) ;
#22098 = CARTESIAN_POINT ( 'NONE',  ( 15.00309677617812554, 1.567672476142359050, 23.00000000000000000 ) ) ;
#22099 = CARTESIAN_POINT ( 'NONE',  ( -19.48557158514982390, 33.75000000000009948, 7.000000000000000000 ) ) ;
#22100 = EDGE_LOOP ( 'NONE', ( #27869, #33789, #33267, #4713 ) ) ;
#22101 = CARTESIAN_POINT ( 'NONE',  ( -3.032905758677766794, 37.61468665050777105, -7.549769678190211941 ) ) ;
#22102 = AXIS2_PLACEMENT_3D ( 'NONE', #23106, #1175, #19451 ) ;
#22103 = DIRECTION ( 'NONE',  ( -0.6691306063588678965, -0.7431448254773855844, 0.000000000000000000 ) ) ;
#22104 = CARTESIAN_POINT ( 'NONE',  ( -0.5000000000000026645, 32.50000000000000000, 10.50000000000000000 ) ) ;
#22105 = CARTESIAN_POINT ( 'NONE',  ( -7.096882951594427169, 29.56287847632736288, 10.00000000000000000 ) ) ;
#22106 = FACE_OUTER_BOUND ( 'NONE', #29488, .T. ) ;
#22107 = CARTESIAN_POINT ( 'NONE',  ( -10.81260707898136531, 32.90853150812170469, 10.63089969389957901 ) ) ;
#22108 = CARTESIAN_POINT ( 'NONE',  ( 8.094548601407081989, 18.84590462288236878, -29.28895203708815487 ) ) ;
#22109 = ORIENTED_EDGE ( 'NONE', *, *, #37398, .F. ) ;
#22110 = CARTESIAN_POINT ( 'NONE',  ( -20.71964873649640282, 12.39161998634679840, -10.88618712900710150 ) ) ;
#22111 = CARTESIAN_POINT ( 'NONE',  ( -13.82587226055958851, 37.11292026377127229, 23.00000000000187583 ) ) ;
#22112 = CARTESIAN_POINT ( 'NONE',  ( 11.22784262000083899, -20.46096934038583015, -20.53583499620931363 ) ) ;
#22113 = LINE ( 'NONE', #25758, #6155 ) ;
#22114 = EDGE_CURVE ( 'NONE', #6485, #24101, #20794, .T. ) ;
#22115 = VECTOR ( 'NONE', #32716, 1000.000000000000000 ) ;
#22116 = CARTESIAN_POINT ( 'NONE',  ( 14.70889546940418136, 25.48292030289299959, -10.64750965446335762 ) ) ;
#22117 = CARTESIAN_POINT ( 'NONE',  ( 8.937590682902566641, -20.71651963383554218, -21.24786896499729494 ) ) ;
#22118 = DIRECTION ( 'NONE',  ( -0.000000000000000000, -0.000000000000000000, -1.000000000000000000 ) ) ;
#22119 = CARTESIAN_POINT ( 'NONE',  ( -26.93779216284742972, -25.25507388614077797, -6.299698065591226026 ) ) ;
#22120 = CARTESIAN_POINT ( 'NONE',  ( 8.427633117194249124, -18.99098521131534412, -26.92671562467327107 ) ) ;
#22121 = CARTESIAN_POINT ( 'NONE',  ( 11.09252425524408459, 17.23965631597926418, -29.99999999999999289 ) ) ;
#22122 = CARTESIAN_POINT ( 'NONE',  ( 17.32296204507781212, -11.70303779259323917, -26.97532818047861269 ) ) ;
#22123 = CARTESIAN_POINT ( 'NONE',  ( 13.63581098909226519, 27.45627467658428600, 10.99999999999999289 ) ) ;
#22124 = CARTESIAN_POINT ( 'NONE',  ( 5.644276917315718123, 36.40655018617690786, 10.49999999999999822 ) ) ;
#22125 = EDGE_LOOP ( 'NONE', ( #7732, #4033, #22398, #21198 ) ) ;
#22126 = CARTESIAN_POINT ( 'NONE',  ( -8.013417946183661655, 33.96338083945676800, -10.23839836295345229 ) ) ;
#22127 = DIRECTION ( 'NONE',  ( 0.7032331762534027586, -0.07391278520357077997, -0.7071067811865484609 ) ) ;
#22128 = CIRCLE ( 'NONE', #37042, 15.00000000000000000 ) ;
#22129 = DIRECTION ( 'NONE',  ( 0.9945218953682730678, -0.1045284632676569819, 0.000000000000000000 ) ) ;
#22130 = ORIENTED_EDGE ( 'NONE', *, *, #23363, .T. ) ;
#22131 = CARTESIAN_POINT ( 'NONE',  ( 30.47427288445410554, -0.0007432638058615850113, -7.827850035976748444 ) ) ;
#22132 = LINE ( 'NONE', #25376, #38802 ) ;
#22133 = PLANE ( 'NONE',  #17416 ) ;
#22134 = B_SPLINE_CURVE_WITH_KNOTS ( 'NONE', 3,
 ( #14770, #34451, #9268, #40139 ),
 .UNSPECIFIED., .F., .F.,
 ( 4, 4 ),
 ( 0.000000000000000000, 1.000000000000000000 ),
 .UNSPECIFIED. ) ;
#22135 = ORIENTED_EDGE ( 'NONE', *, *, #8143, .T. ) ;
#22136 = CARTESIAN_POINT ( 'NONE',  ( -20.81434011470259193, 0.8451126377779130117, -26.83172302409398924 ) ) ;
#22137 = DIRECTION ( 'NONE',  ( 0.000000000000000000, 0.000000000000000000, 1.000000000000000000 ) ) ;
#22138 = EDGE_LOOP ( 'NONE', ( #33255, #22623, #38414, #36629 ) ) ;
#22139 = CARTESIAN_POINT ( 'NONE',  ( 34.03611443232053091, -6.103416065348592490, -8.094509381288824912 ) ) ;
#22140 = ORIENTED_EDGE ( 'NONE', *, *, #38040, .T. ) ;
#22141 = CARTESIAN_POINT ( 'NONE',  ( 7.508063977623086416, 38.75471409550124235, 12.73282698324837803 ) ) ;
#22142 = PLANE ( 'NONE',  #35258 ) ;
#22143 = CARTESIAN_POINT ( 'NONE',  ( -8.842909878189049167, 12.23753042740625752, 23.00000000000000355 ) ) ;
#22144 = CARTESIAN_POINT ( 'NONE',  ( 8.843001881758423721, 30.00677403926963294, 19.66345542862529783 ) ) ;
#22145 = CARTESIAN_POINT ( 'NONE',  ( -13.28503138821885798, 15.53523575316151195, 7.499999999999993783 ) ) ;
#22146 = ORIENTED_EDGE ( 'NONE', *, *, #5916, .F. ) ;
#22147 = CARTESIAN_POINT ( 'NONE',  ( -10.72918489117944674, 32.98258515686310943, 7.500000000000004441 ) ) ;
#22148 = CARTESIAN_POINT ( 'NONE',  ( 1.419287350250943325, 20.45362594422159219, -30.00000000000000711 ) ) ;
#22149 = CARTESIAN_POINT ( 'NONE',  ( -14.36830325120615903, 20.48707633493503621, 7.500000000000004441 ) ) ;
#22150 = CARTESIAN_POINT ( 'NONE',  ( -13.05736835487441994, 16.11602540378456183, 9.500000000000000000 ) ) ;
#22151 = CARTESIAN_POINT ( 'NONE',  ( 16.28467717620302579, 16.38496874790540758, -17.87567372210706296 ) ) ;
#22152 = CARTESIAN_POINT ( 'NONE',  ( 5.103355680224397339, 19.86390335519187289, -29.24334217793310842 ) ) ;
#22153 = CIRCLE ( 'NONE', #28624, 0.5000000000000004441 ) ;
#22154 = VECTOR ( 'NONE', #37597, 1000.000000000000000 ) ;
#22155 = EDGE_CURVE ( 'NONE', #24567, #747, #24761, .T. ) ;
#22156 = CARTESIAN_POINT ( 'NONE',  ( 14.72827463056593444, -23.14637955489208565, -15.28270852680887693 ) ) ;
#22157 = CARTESIAN_POINT ( 'NONE',  ( -4.817371740575545402, 23.83900317890010001, 20.99999999999999645 ) ) ;
#22158 = CARTESIAN_POINT ( 'NONE',  ( -2.605702774688126500, 27.44183462127829642, 12.00000000000000000 ) ) ;
#22159 = ORIENTED_EDGE ( 'NONE', *, *, #17587, .F. ) ;
#22160 = CARTESIAN_POINT ( 'NONE',  ( -14.54212453546162465, 24.94396834142040120, -11.59977209224463479 ) ) ;
#22161 = CARTESIAN_POINT ( 'NONE',  ( -26.77946264071690052, -24.43926981373589058, 17.42190598798356049 ) ) ;
#22162 = CARTESIAN_POINT ( 'NONE',  ( 9.346475367005044887, -18.24555389153483631, -30.00000000000000000 ) ) ;
#22163 = EDGE_CURVE ( 'NONE', #3967, #27076, #8295, .T. ) ;
#22164 = CONICAL_SURFACE ( 'NONE', #11135, 1.000000000000000888, 0.7853981633974548293 ) ;
#22165 = DIRECTION ( 'NONE',  ( 1.000000000000000000, 0.000000000000000000, 0.000000000000000000 ) ) ;
#22166 = ADVANCED_FACE ( 'NONE', ( #19129, #37417, #12829, #6526, #28069, #6921, #22567, #22365, #9391, #3885, #19325, #9591, #37623, #34176, #30928, #3091, #3686, #25225, #3488, #6132, #28669, #27873, #28469, #31721, #247, #844, #12431, #25023, #34570, #3289, #12634, #15681, #18537, #16081, #34772, #21975, #13223, #9791, #6720, #34376, #18931, #25615, #38015, #15487, #37814, #24823, #37221, #6326, #18737, #644, #31126, #31319, #15885, #31523, #13025, #25416, #35780, #11194, #11000, #38221, #32737, #7933, #32540, #31917, #1857, #16690, #4694, #7737, #13632, #23384, #16487, #22768, #28873, #17099, #20344, #14236, #29072, #29474, #20140, #26019, #4893, #7127, #25821, #14034, #38618, #39017 ), #1651, .T. ) ;
#22167 = EDGE_LOOP ( 'NONE', ( #34587, #23151, #11750 ) ) ;
#22168 = EDGE_LOOP ( 'NONE', ( #5525, #11168 ) ) ;
#22169 = CARTESIAN_POINT ( 'NONE',  ( -14.36450198187400318, 29.42115241676423310, -6.376794364350948818 ) ) ;
#22170 = CARTESIAN_POINT ( 'NONE',  ( -6.460609604078108248, 35.78147008481153080, 10.94611345180489970 ) ) ;
#22171 = CARTESIAN_POINT ( 'NONE',  ( 14.98890121934609532, -28.67928442654220333, 11.00000000000000000 ) ) ;
#22172 = CARTESIAN_POINT ( 'NONE',  ( -33.71982540184990995, -9.379966980860906745, -9.801996931721211226 ) ) ;
#22173 = CARTESIAN_POINT ( 'NONE',  ( -15.12720010012756156, -26.36448638230414687, -7.828442106200601991 ) ) ;
#22174 = DIRECTION ( 'NONE',  ( 1.000000000000000000, 0.000000000000000000, 0.000000000000000000 ) ) ;
#22175 = ORIENTED_EDGE ( 'NONE', *, *, #22710, .F. ) ;
#22176 = CARTESIAN_POINT ( 'NONE',  ( 25.72413230257677341, 0.5541670876175327498, -16.46445719556119514 ) ) ;
#22177 = DIRECTION ( 'NONE',  ( 1.000000000000000000, 0.000000000000000000, 0.000000000000000000 ) ) ;
#22178 = LINE ( 'NONE', #31134, #15394 ) ;
#22179 = VERTEX_POINT ( 'NONE', #17303 ) ;
#22180 = CARTESIAN_POINT ( 'NONE',  ( -30.92750986253986767, -0.06599190286722655951, -5.000000000000000000 ) ) ;
#22181 = VERTEX_POINT ( 'NONE', #13427 ) ;
#22182 = CARTESIAN_POINT ( 'NONE',  ( 32.75437695154221274, -2.309567439508531272, -5.462365998068315243 ) ) ;
#22183 = CARTESIAN_POINT ( 'NONE',  ( -7.326526595265096198, -19.15832871326084330, -30.00000000000001066 ) ) ;
#22184 = CARTESIAN_POINT ( 'NONE',  ( 27.27686897040210212, -25.33890797347431700, 16.30093088680153102 ) ) ;
#22185 = EDGE_CURVE ( 'NONE', #2515, #9387, #26425, .T. ) ;
#22186 = ORIENTED_EDGE ( 'NONE', *, *, #31257, .T. ) ;
#22187 = EDGE_CURVE ( 'NONE', #23393, #30574, #15276, .T. ) ;
#22188 = DIRECTION ( 'NONE',  ( 0.000000000000000000, 0.000000000000000000, 1.000000000000000000 ) ) ;
#22189 = CARTESIAN_POINT ( 'NONE',  ( -0.5415361484147104276, 27.50000000000004263, 20.99999999999998934 ) ) ;
#22190 = CARTESIAN_POINT ( 'NONE',  ( 10.44103466624280685, 32.57396620494213124, 9.000000000000001776 ) ) ;
#22191 = DIRECTION ( 'NONE',  ( 0.000000000000000000, 0.000000000000000000, 1.000000000000000000 ) ) ;
#22192 = AXIS2_PLACEMENT_3D ( 'NONE', #30590, #15936, #18393 ) ;
#22193 = LINE ( 'NONE', #18957, #6088 ) ;
#22194 = CARTESIAN_POINT ( 'NONE',  ( 17.34253826607094240, 27.32041144404343314, 11.55979286843934872 ) ) ;
#22195 = CARTESIAN_POINT ( 'NONE',  ( -22.97007816870513608, 9.885904127924739271, -5.482133400955172320 ) ) ;
#22196 = CARTESIAN_POINT ( 'NONE',  ( 22.46963405367063160, -26.15767612554902399, -8.532870437220990922 ) ) ;
#22197 = CARTESIAN_POINT ( 'NONE',  ( -10.16521142134453548, 24.66068167190384841, 12.00000000000000000 ) ) ;
#22198 = EDGE_CURVE ( 'NONE', #22676, #11758, #10086, .T. ) ;
#22199 = CARTESIAN_POINT ( 'NONE',  ( 12.82845314113447444, 21.81843741845949580, -17.41504233143949776 ) ) ;
#22200 = ORIENTED_EDGE ( 'NONE', *, *, #24420, .F. ) ;
#22201 = CARTESIAN_POINT ( 'NONE',  ( -13.77473007477936306, 20.30411881401572316, -17.57123835615476892 ) ) ;
#22202 = AXIS2_PLACEMENT_3D ( 'NONE', #13456, #16520, #19357 ) ;
#22203 = CARTESIAN_POINT ( 'NONE',  ( -25.23650320482248333, -19.40090744331417127, 20.25080042701566185 ) ) ;
#22204 = DIRECTION ( 'NONE',  ( 0.2926062055178220711, -0.7622652262560022374, 0.5773502691896384986 ) ) ;
#22205 = CARTESIAN_POINT ( 'NONE',  ( 15.19494511612774090, 26.21339590839900069, -8.298239470938288065 ) ) ;
#22206 = VERTEX_POINT ( 'NONE', #38820 ) ;
#22207 = CARTESIAN_POINT ( 'NONE',  ( 11.39463915635820612, 18.33192650902018883, 13.00000000000000178 ) ) ;
#22208 = ORIENTED_EDGE ( 'NONE', *, *, #29999, .T. ) ;
#22210 = DIRECTION ( 'NONE',  ( -1.000000000000000000, 0.000000000000000000, 0.000000000000000000 ) ) ;
#22209 = CARTESIAN_POINT ( 'NONE',  ( -10.88757786208257805, 17.52439729938563318, -28.06831848310639899 ) ) ;
#22211 = CARTESIAN_POINT ( 'NONE',  ( -9.580852559982135475, -18.12344168749379492, -30.00000000000000000 ) ) ;
#22212 = CARTESIAN_POINT ( 'NONE',  ( 18.00000000000000000, 22.50000000000000711, 6.000000000000000000 ) ) ;
#22213 = ORIENTED_EDGE ( 'NONE', *, *, #12994, .T. ) ;
#22214 = CARTESIAN_POINT ( 'NONE',  ( -22.78420442030176929, -11.94118074355967352, -19.63367908279295548 ) ) ;
#22215 = CARTESIAN_POINT ( 'NONE',  ( -12.34945208490760216, -23.53982313883594202, -14.53211625936720885 ) ) ;
#22216 = LINE ( 'NONE', #22824, #19624 ) ;
#22217 = CARTESIAN_POINT ( 'NONE',  ( 14.60279944388903495, 20.71121289329725457, -15.60062821346018325 ) ) ;
#22218 = ORIENTED_EDGE ( 'NONE', *, *, #5820, .T. ) ;
#22219 = CARTESIAN_POINT ( 'NONE',  ( 21.81847007083357326, 4.523505414233293109, -20.94089222306983089 ) ) ;
#22220 = CYLINDRICAL_SURFACE ( 'NONE', #38148, 0.5000000000000004441 ) ;
#22221 = CIRCLE ( 'NONE', #23543, 0.5000000000000004441 ) ;
#22222 = DIRECTION ( 'NONE',  ( 0.9510565162951543083, 0.3090169943749450088, 0.000000000000000000 ) ) ;
#22223 = CARTESIAN_POINT ( 'NONE',  ( -13.22516817658055288, 40.70288237343638826, 7.000000000000000000 ) ) ;
#22224 = ORIENTED_EDGE ( 'NONE', *, *, #34171, .T. ) ;
#22225 = CARTESIAN_POINT ( 'NONE',  ( -20.84162644709726209, 0.4883270344463671031, -26.80397353251239423 ) ) ;
#22226 = CARTESIAN_POINT ( 'NONE',  ( 31.20266475843156329, -0.3930892854634324141, -5.941229959064580513 ) ) ;
#22227 = AXIS2_PLACEMENT_3D ( 'NONE', #27034, #1655, #38622 ) ;
#22228 = CARTESIAN_POINT ( 'NONE',  ( 25.23650320482206055, -19.40090744331450878, 20.25080042701540961 ) ) ;
#22229 = ORIENTED_EDGE ( 'NONE', *, *, #5019, .F. ) ;
#22230 = EDGE_CURVE ( 'NONE', #15233, #5452, #27600, .T. ) ;
#22231 = CARTESIAN_POINT ( 'NONE',  ( -31.47283671532259675, -25.12609584734821411, -5.000000000000010658 ) ) ;
#22232 = PLANE ( 'NONE',  #5048 ) ;
#22233 = AXIS2_PLACEMENT_3D ( 'NONE', #5521, #17934, #2880 ) ;
#22234 = ORIENTED_EDGE ( 'NONE', *, *, #11141, .F. ) ;
#22235 = LINE ( 'NONE', #21647, #26206 ) ;
#22236 = AXIS2_PLACEMENT_3D ( 'NONE', #14017, #26407, #32722 ) ;
#22237 = LINE ( 'NONE', #16561, #33769 ) ;
#22238 = DIRECTION ( 'NONE',  ( -1.000000000000000000, 0.000000000000000000, 0.000000000000000000 ) ) ;
#22239 = CARTESIAN_POINT ( 'NONE',  ( 2.971324280269732387, 22.57991813769753264, -23.03519204931057374 ) ) ;
#22240 = CARTESIAN_POINT ( 'NONE',  ( 14.97009266215792778, 21.42933399866928568, 10.49999999999999822 ) ) ;
#22241 = CARTESIAN_POINT ( 'NONE',  ( -3.610593701936590794, 31.83882289796395426, 10.50000000000000533 ) ) ;
#22242 = AXIS2_PLACEMENT_3D ( 'NONE', #10027, #35418, #38461 ) ;
#22243 = CARTESIAN_POINT ( 'NONE',  ( -1.693998953219646664, 12.12549434688617644, 10.50000000000000000 ) ) ;
#22244 = FACE_OUTER_BOUND ( 'NONE', #4293, .T. ) ;
#22245 = DIRECTION ( 'NONE',  ( 1.000000000000000000, 0.000000000000000000, 0.000000000000000000 ) ) ;
#22246 = EDGE_CURVE ( 'NONE', #36663, #15234, #34977, .T. ) ;
#22247 = CARTESIAN_POINT ( 'NONE',  ( 10.56422568374752480, 17.99037428788165371, -26.77787062081501190 ) ) ;
#22248 = DIRECTION ( 'NONE',  ( -0.4156269377774519658, 0.5720614028176885801, 0.7071067811865450192 ) ) ;
#22249 = ORIENTED_EDGE ( 'NONE', *, *, #15295, .F. ) ;
#22250 = CIRCLE ( 'NONE', #33308, 0.4999999999999997780 ) ;
#22252 = CARTESIAN_POINT ( 'NONE',  ( 14.98890121934609532, -28.67928442654221044, -5.000000000000000000 ) ) ;
#22251 = CARTESIAN_POINT ( 'NONE',  ( -18.26045280058711739, 18.67344520970426913, -5.958434712537178157 ) ) ;
#22253 = LINE ( 'NONE', #34463, #39953 ) ;
#22254 = ADVANCED_FACE ( 'NONE', ( #4494 ), #24921, .T. ) ;
#22255 = CARTESIAN_POINT ( 'NONE',  ( 15.45091137245021429, -26.73300375246232008, -5.000000000000000000 ) ) ;
#22256 = DIRECTION ( 'NONE',  ( 0.9510565162951541973, 0.3090169943749456194, 1.040834085586083783E-14 ) ) ;
#22257 = CARTESIAN_POINT ( 'NONE',  ( 14.29112916160344859, 24.47062756151937180, -12.55066837350503839 ) ) ;
#22258 = ORIENTED_EDGE ( 'NONE', *, *, #34421, .T. ) ;
#22259 = CARTESIAN_POINT ( 'NONE',  ( 15.28428319961222570, 26.55126983923268114, -7.357174194785967458 ) ) ;
#22260 = VERTEX_POINT ( 'NONE', #26829 ) ;
#22261 = DIRECTION ( 'NONE',  ( 1.000000000000000000, 0.000000000000000000, 0.000000000000000000 ) ) ;
#22262 = CARTESIAN_POINT ( 'NONE',  ( -15.39818770356525945, -26.71945962344603487, -5.000000000000000888 ) ) ;
#22263 = CARTESIAN_POINT ( 'NONE',  ( -20.77381726376759019, -29.00435581194061641, 12.73282698324853257 ) ) ;
#22264 = EDGE_CURVE ( 'NONE', #445, #8575, #20544, .T. ) ;
#22265 = CARTESIAN_POINT ( 'NONE',  ( -25.96013749710196450, -19.13211056138908361, -13.82494223876936346 ) ) ;
#22266 = CARTESIAN_POINT ( 'NONE',  ( -1.948798780195311275, -21.39903356808110146, -22.24353699554251662 ) ) ;
#22267 = CARTESIAN_POINT ( 'NONE',  ( 12.51562164745455874, 19.46842532610077825, -20.60745837019819859 ) ) ;
#22268 = EDGE_LOOP ( 'NONE', ( #39053, #25479, #2956, #11091 ) ) ;
#22269 = CARTESIAN_POINT ( 'NONE',  ( 23.39763224849028234, 9.229310415396369649, -4.999999999999999112 ) ) ;
#22270 = FACE_OUTER_BOUND ( 'NONE', #24733, .T. ) ;
#22271 = CARTESIAN_POINT ( 'NONE',  ( -13.41665185498830937, 27.84207739517983171, 17.92354375535208888 ) ) ;
#22272 = VECTOR ( 'NONE', #18166, 1000.000000000000000 ) ;
#22273 = ORIENTED_EDGE ( 'NONE', *, *, #32223, .T. ) ;
#22274 = CARTESIAN_POINT ( 'NONE',  ( -33.86638135467044464, -4.484472903435158919, -6.349560011803310644 ) ) ;
#22275 = VECTOR ( 'NONE', #24314, 1000.000000000000000 ) ;
#22276 = CARTESIAN_POINT ( 'NONE',  ( -28.25018339770460685, -2.647087534799629438, 19.27171037444156809 ) ) ;
#22277 = ORIENTED_EDGE ( 'NONE', *, *, #23307, .T. ) ;
#22278 = CARTESIAN_POINT ( 'NONE',  ( -11.41268156625113406, 18.79179606750104981, 6.000000000000000000 ) ) ;
#22279 = AXIS2_PLACEMENT_3D ( 'NONE', #32297, #13798, #19903 ) ;
#22280 = CARTESIAN_POINT ( 'NONE',  ( 24.49503443140846315, -11.70166252807803176, 23.00000000000000000 ) ) ;
#22281 = EDGE_CURVE ( 'NONE', #26114, #12596, #2326, .T. ) ;
#22282 = CARTESIAN_POINT ( 'NONE',  ( -24.79870091042203484, 1.154735779887344771, -17.51345790379463807 ) ) ;
#22283 = ADVANCED_FACE ( 'NONE', ( #8746 ), #15911, .T. ) ;
#22284 = CARTESIAN_POINT ( 'NONE',  ( 19.60579457783088841, -8.618293326532800336, -25.60564762322205823 ) ) ;
#22285 = EDGE_CURVE ( 'NONE', #13694, #18489, #5488, .T. ) ;
#22286 = CARTESIAN_POINT ( 'NONE',  ( 24.59814121633610640, -28.40949844211205644, 12.73282698324863738 ) ) ;
#22287 = CIRCLE ( 'NONE', #8669, 1.000000000000000000 ) ;
#22288 = EDGE_LOOP ( 'NONE', ( #10310, #1409 ) ) ;
#22289 = ORIENTED_EDGE ( 'NONE', *, *, #9993, .F. ) ;
#22290 = LINE ( 'NONE', #13145, #261 ) ;
#22291 = CARTESIAN_POINT ( 'NONE',  ( 33.75875814100320582, 2.759858869446452534, 22.99999999999999645 ) ) ;
#22292 = DIRECTION ( 'NONE',  ( 1.000000000000000000, 0.000000000000000000, 0.000000000000000000 ) ) ;
#22293 = VERTEX_POINT ( 'NONE', #17902 ) ;
#22294 = AXIS2_PLACEMENT_3D ( 'NONE', #39292, #1933, #29347 ) ;
#22295 = CARTESIAN_POINT ( 'NONE',  ( -0.4054287150579977683, 20.91504830566051254, -26.96527958665584634 ) ) ;
#22296 = FACE_OUTER_BOUND ( 'NONE', #4050, .T. ) ;
#22297 = CARTESIAN_POINT ( 'NONE',  ( 5.644276917315719899, 36.40655018617690786, 10.49999999999999822 ) ) ;
#22298 = FACE_OUTER_BOUND ( 'NONE', #1484, .T. ) ;
#22299 = CARTESIAN_POINT ( 'NONE',  ( 6.706335727061685681, 24.35410196624994583, 12.00000000000000000 ) ) ;
#22300 = EDGE_CURVE ( 'NONE', #36787, #4871, #31490, .T. ) ;
#22301 = CARTESIAN_POINT ( 'NONE',  ( -4.082607396026893376, 23.58034083595207875, 6.000000000000000000 ) ) ;
#22302 = CIRCLE ( 'NONE', #21013, 1.000000000000000000 ) ;
#22303 = CARTESIAN_POINT ( 'NONE',  ( 11.02804646868720617, 24.24809588149700090, -17.10494504817883055 ) ) ;
#22304 = CARTESIAN_POINT ( 'NONE',  ( 2.501562340374731352, 7.696614566897833853, 10.50000000000000000 ) ) ;
#22305 = ORIENTED_EDGE ( 'NONE', *, *, #25010, .T. ) ;
#22307 = DIRECTION ( 'NONE',  ( 1.000000000000000000, 0.000000000000000000, 0.000000000000000000 ) ) ;
#22306 = CARTESIAN_POINT ( 'NONE',  ( -20.55655765742755747, 12.29105890200828455, -11.88403847902282529 ) ) ;
#22308 = LINE ( 'NONE', #779, #3648 ) ;
#22309 = EDGE_CURVE ( 'NONE', #10247, #22086, #30286, .T. ) ;
#22310 = CARTESIAN_POINT ( 'NONE',  ( 12.70345522867710741, -22.55901976966053368, -16.43839307279606032 ) ) ;
#22311 = DIRECTION ( 'NONE',  ( 0.000000000000000000, 0.000000000000000000, 1.000000000000000000 ) ) ;
#22312 = CARTESIAN_POINT ( 'NONE',  ( 10.93327523444657778, 17.34109439532409525, -29.34725070414031478 ) ) ;
#22313 = CARTESIAN_POINT ( 'NONE',  ( 7.289639608743135213, -27.06962010326278190, -5.000000000000004441 ) ) ;
#22314 = CARTESIAN_POINT ( 'NONE',  ( 9.331903152615748098, 11.35703883385568780, 10.49999999999999645 ) ) ;
#22315 = VECTOR ( 'NONE', #2177, 999.9999999999998863 ) ;
#22316 = CARTESIAN_POINT ( 'NONE',  ( -17.85134198839684316, -18.89656077001060552, -18.85215370857916639 ) ) ;
#22317 = CARTESIAN_POINT ( 'NONE',  ( 6.120099083145483121, -24.74703752395057421, -8.867573918171460789 ) ) ;
#22318 = CARTESIAN_POINT ( 'NONE',  ( 14.60292836218529544, 24.77861828538451050, -11.60468508207308069 ) ) ;
#22319 = CARTESIAN_POINT ( 'NONE',  ( 17.38935910474636160, -12.52520610644180366, -25.59909104371132216 ) ) ;
#22320 = CARTESIAN_POINT ( 'NONE',  ( 14.11133924723984201, 27.61078317377173619, 10.59344459855563514 ) ) ;
#22321 = DIRECTION ( 'NONE',  ( -0.4999999999999919509, 0.8660254037844432595, 0.000000000000000000 ) ) ;
#22322 = ORIENTED_EDGE ( 'NONE', *, *, #12742, .T. ) ;
#22323 = CARTESIAN_POINT ( 'NONE',  ( -8.044889785369548463, 30.10955582739369163, -13.93146741096502872 ) ) ;
#22324 = CARTESIAN_POINT ( 'NONE',  ( 14.86131180699620735, 21.44076732726258072, 10.82238861112335471 ) ) ;
#22325 = ORIENTED_EDGE ( 'NONE', *, *, #25141, .T. ) ;
#22326 = CARTESIAN_POINT ( 'NONE',  ( 25.87031140294526921, 0.3067695561049477715, -16.44274321582222953 ) ) ;
#22327 = DIRECTION ( 'NONE',  ( 1.000000000000000000, 0.000000000000000000, 0.000000000000000000 ) ) ;
#22328 = DIRECTION ( 'NONE',  ( 0.3090169943749450643, -0.9510565162951544194, 0.000000000000000000 ) ) ;
#22329 = VERTEX_POINT ( 'NONE', #24179 ) ;
#22330 = CARTESIAN_POINT ( 'NONE',  ( -27.11474883183905504, 0.2720220986060000734, -14.47902593302377738 ) ) ;
#22331 = DIRECTION ( 'NONE',  ( 0.000000000000000000, 0.000000000000000000, 1.000000000000000000 ) ) ;
#22332 = ORIENTED_EDGE ( 'NONE', *, *, #36476, .F. ) ;
#22333 = CARTESIAN_POINT ( 'NONE',  ( 20.16346151983087509, -4.126571039269510521, -28.54077426291244990 ) ) ;
#22334 = AXIS2_PLACEMENT_3D ( 'NONE', #26257, #37504, #18624 ) ;
#22335 = VERTEX_POINT ( 'NONE', #32938 ) ;
#22336 = CARTESIAN_POINT ( 'NONE',  ( 16.82090372984188065, 29.19711159930560740, 10.99999999999877609 ) ) ;
#22337 = DIRECTION ( 'NONE',  ( -0.6691306063588653430, -0.7431448254773878048, 0.000000000000000000 ) ) ;
#22338 = CARTESIAN_POINT ( 'NONE',  ( 6.774334011770120512, 35.84443018111158352, 10.49999999999999822 ) ) ;
#22339 = CARTESIAN_POINT ( 'NONE',  ( -2.823200210931145815, 35.29864485453418865, 18.87996532025786323 ) ) ;
#22340 = VECTOR ( 'NONE', #25687, 1000.000000000000114 ) ;
#22341 = DIRECTION ( 'NONE',  ( 1.000000000000000000, 0.000000000000000000, 0.000000000000000000 ) ) ;
#22342 = ORIENTED_EDGE ( 'NONE', *, *, #29798, .F. ) ;
#22343 = CARTESIAN_POINT ( 'NONE',  ( 3.607749162633205220, 7.931741834401766944, 10.50000000000000178 ) ) ;
#22344 = CARTESIAN_POINT ( 'NONE',  ( -18.10143317280823894, -9.644849403491171813, -30.00000000000001421 ) ) ;
#22345 = CARTESIAN_POINT ( 'NONE',  ( 0.000000000000000000, 22.50000000000000355, 7.000000000000000000 ) ) ;
#22346 = CARTESIAN_POINT ( 'NONE',  ( -8.806982162272252168, 13.84996144622306247, 13.00000000000000178 ) ) ;
#22347 = CARTESIAN_POINT ( 'NONE',  ( 17.84657098941836040, 18.57841126220657557, -9.344939892030197370 ) ) ;
#22348 = CARTESIAN_POINT ( 'NONE',  ( 5.797474147347187134, 25.70591046706581295, -18.75075227247661758 ) ) ;
#22349 = VERTEX_POINT ( 'NONE', #2456 ) ;
#22350 = CARTESIAN_POINT ( 'NONE',  ( 16.16426081259751513, -26.77215978000938890, -6.871636933944165193 ) ) ;
#22351 = CARTESIAN_POINT ( 'NONE',  ( -0.5415361484146622439, 27.50000000000005329, 21.00000000000000355 ) ) ;
#22352 = DIRECTION ( 'NONE',  ( -0.000000000000000000, -0.000000000000000000, 1.000000000000000000 ) ) ;
#22353 = VECTOR ( 'NONE', #38001, 1000.000000000000114 ) ;
#22354 = ORIENTED_EDGE ( 'NONE', *, *, #28655, .T. ) ;
#22355 = CARTESIAN_POINT ( 'NONE',  ( -15.39831948222068192, 26.75390157443277772, -5.946046044839542688 ) ) ;
#22356 = CARTESIAN_POINT ( 'NONE',  ( -34.68832217153530451, -7.625465254389222736, 16.87380292611359778 ) ) ;
#22357 = CARTESIAN_POINT ( 'NONE',  ( 12.19254079021881587, -22.55338299999295870, -16.47865374781240888 ) ) ;
#22358 = LINE ( 'NONE', #16481, #18555 ) ;
#22359 = ORIENTED_EDGE ( 'NONE', *, *, #15873, .F. ) ;
#22360 = ORIENTED_EDGE ( 'NONE', *, *, #6509, .F. ) ;
#22361 = CARTESIAN_POINT ( 'NONE',  ( -8.916636640703819339, 18.64685610723298836, -27.95511672575932494 ) ) ;
#22362 = AXIS2_PLACEMENT_3D ( 'NONE', #34858, #19406, #3966 ) ;
#22363 = CARTESIAN_POINT ( 'NONE',  ( -12.11431924477676425, -16.53859993892360336, -30.00000000000000711 ) ) ;
#22364 =( BOUNDED_CURVE ( )  B_SPLINE_CURVE ( 2, ( #12531, #22070, #15582 ),
 .UNSPECIFIED., .F., .F. ) 
 B_SPLINE_CURVE_WITH_KNOTS ( ( 3, 3 ),
 ( 0.000000000000000000, 1.000000000000000000 ),
 .UNSPECIFIED. ) 
 CURVE ( )  GEOMETRIC_REPRESENTATION_ITEM ( )  RATIONAL_B_SPLINE_CURVE ( ( 1.000000000000000000, 0.7071067811865475727, 1.000000000000000000 ) ) 
 REPRESENTATION_ITEM ( '' )  );
#22365 = FACE_BOUND ( 'NONE', #13329, .T. ) ;
#22366 = CIRCLE ( 'NONE', #15910, 18.00000000000000355 ) ;
#22367 = CARTESIAN_POINT ( 'NONE',  ( -24.28665842282865839, -6.776736144980733734, -19.81828135623066345 ) ) ;
#22368 = DIRECTION ( 'NONE',  ( -0.000000000000000000, 0.000000000000000000, -1.000000000000000000 ) ) ;
#22369 = ORIENTED_EDGE ( 'NONE', *, *, #30723, .T. ) ;
#22370 = CARTESIAN_POINT ( 'NONE',  ( 29.18931739517128676, 0.2643966938976765602, -10.65876322853514502 ) ) ;
#22371 = CARTESIAN_POINT ( 'NONE',  ( 13.94482798346721175, 26.50521816028912525, 11.00000000000000000 ) ) ;
#22372 = LINE ( 'NONE', #34778, #35548 ) ;
#22373 = VERTEX_POINT ( 'NONE', #39218 ) ;
#22374 = CARTESIAN_POINT ( 'NONE',  ( -25.87499874312591785, 0.2997861449386328148, -16.44121720947547871 ) ) ;
#22375 = ORIENTED_EDGE ( 'NONE', *, *, #21667, .T. ) ;
#22376 = CARTESIAN_POINT ( 'NONE',  ( 29.56918532523465259, -1.550794330668424648, -12.39820313618830205 ) ) ;
#22377 = CARTESIAN_POINT ( 'NONE',  ( 22.38472516250418209, -15.35952186208521120, 20.99999999999999645 ) ) ;
#22378 = CARTESIAN_POINT ( 'NONE',  ( 34.83511892542234278, -16.10726664690938392, 16.30093088680188984 ) ) ;
#22379 = ADVANCED_FACE ( 'NONE', ( #23781 ), #32154, .T. ) ;
#22380 = ORIENTED_EDGE ( 'NONE', *, *, #9518, .F. ) ;
#22381 = CARTESIAN_POINT ( 'NONE',  ( -12.63297681466540467, 33.22352044042957431, 15.72805884748945005 ) ) ;
#22382 = CARTESIAN_POINT ( 'NONE',  ( -1.693998953219642223, 12.12549434688618888, 11.00000000000000000 ) ) ;
#22383 = AXIS2_PLACEMENT_3D ( 'NONE', #33085, #20487, #23327 ) ;
#22384 = CARTESIAN_POINT ( 'NONE',  ( -5.400187688428998334E-14, 29.10878045366048639, 20.94377226548378346 ) ) ;
#22385 = DIRECTION ( 'NONE',  ( 0.3090169943749574988, 0.9510565162951503115, 0.000000000000000000 ) ) ;
#22386 = EDGE_CURVE ( 'NONE', #37263, #1779, #27231, .T. ) ;
#22387 = DIRECTION ( 'NONE',  ( 0.000000000000000000, 0.000000000000000000, 1.000000000000000000 ) ) ;
#22388 = EDGE_CURVE ( 'NONE', #39356, #14996, #6201, .T. ) ;
#22389 = VECTOR ( 'NONE', #33826, 1000.000000000000000 ) ;
#22390 = VECTOR ( 'NONE', #12510, 1000.000000000000000 ) ;
#22391 = VECTOR ( 'NONE', #1251, 1000.000000000000000 ) ;
#22392 = FACE_BOUND ( 'NONE', #23978, .T. ) ;
#22393 = CYLINDRICAL_SURFACE ( 'NONE', #28931, 1.000000000000000000 ) ;
#22394 = CARTESIAN_POINT ( 'NONE',  ( -22.85284608940409257, 9.847895807180515604, -7.423717738255721343 ) ) ;
#22395 = CARTESIAN_POINT ( 'NONE',  ( 13.47898897988460121, -15.87835076097369580, -27.16664839183066249 ) ) ;
#22396 = DIRECTION ( 'NONE',  ( 1.000000000000000000, 0.000000000000000000, 0.000000000000000000 ) ) ;
#22397 = CARTESIAN_POINT ( 'NONE',  ( 11.38208074324289854, 18.52518290154176483, -23.83773640263114046 ) ) ;
#22398 = ORIENTED_EDGE ( 'NONE', *, *, #3274, .T. ) ;
#22399 = CARTESIAN_POINT ( 'NONE',  ( -15.38402806139854384, 25.23968687678138068, -8.776766146092349175 ) ) ;
#22400 = CARTESIAN_POINT ( 'NONE',  ( -28.38958307348538668, -9.126824876481562043, 20.50957957745985283 ) ) ;
#22401 = EDGE_CURVE ( 'NONE', #30063, #28113, #2649, .T. ) ;
#22402 = DIRECTION ( 'NONE',  ( 0.000000000000000000, 0.000000000000000000, 1.000000000000000000 ) ) ;
#22403 = CARTESIAN_POINT ( 'NONE',  ( 13.51484764804600935, 22.76996113590243453, -15.45381432112062825 ) ) ;
#22404 = VERTEX_POINT ( 'NONE', #14433 ) ;
#22405 = CARTESIAN_POINT ( 'NONE',  ( 33.70372332681250782, -18.58847439657466083, -5.435464265174550391 ) ) ;
#22406 = CYLINDRICAL_SURFACE ( 'NONE', #38476, 0.5000000000000007772 ) ;
#22407 = ORIENTED_EDGE ( 'NONE', *, *, #37188, .T. ) ;
#22409 = CARTESIAN_POINT ( 'NONE',  ( -12.80736835487442349, 15.68301270189233954, 11.00000000000000000 ) ) ;
#22408 = CARTESIAN_POINT ( 'NONE',  ( -11.92048302216191047, 20.17252841636972960, -20.49873944758164868 ) ) ;
#22410 = CARTESIAN_POINT ( 'NONE',  ( -9.994354138142316657, -18.05759666164655286, -28.05362611333584866 ) ) ;
#22411 = CARTESIAN_POINT ( 'NONE',  ( 12.23768179954923419, 14.31935546172391760, 10.49999999999999822 ) ) ;
#22412 = ORIENTED_EDGE ( 'NONE', *, *, #34397, .T. ) ;
#22413 = CARTESIAN_POINT ( 'NONE',  ( -18.43967439804336550, -8.978407292334221523, -30.00000000000000711 ) ) ;
#22414 = CARTESIAN_POINT ( 'NONE',  ( -9.792301971375101388, -19.78694043973939287, -22.82254168301635033 ) ) ;
#22415 = DIRECTION ( 'NONE',  ( 1.000000000000000000, 0.000000000000000000, 0.000000000000000000 ) ) ;
#22416 = CARTESIAN_POINT ( 'NONE',  ( 15.52145767144611099, 22.42669402248078470, -11.67624505304624094 ) ) ;
#22417 = EDGE_LOOP ( 'NONE', ( #21171, #11549, #1307, #38047 ) ) ;
#22418 = CARTESIAN_POINT ( 'NONE',  ( 25.41189056253793410, 4.628821310671148659, -11.75822289690720268 ) ) ;
#22419 = FACE_OUTER_BOUND ( 'NONE', #22609, .T. ) ;
#22420 = CARTESIAN_POINT ( 'NONE',  ( 3.485571585149872753, -11.24999999999998224, 6.000000000000000000 ) ) ;
#22421 = DIRECTION ( 'NONE',  ( 1.000000000000000000, 0.000000000000000000, 0.000000000000000000 ) ) ;
#22422 = ORIENTED_EDGE ( 'NONE', *, *, #37609, .T. ) ;
#22423 = CARTESIAN_POINT ( 'NONE',  ( -28.02036111935687757, -0.1831946594191615485, -13.47373158784090563 ) ) ;
#22424 = CARTESIAN_POINT ( 'NONE',  ( 23.40003965484141446, 0.3230641209998412200, -20.51045967696057559 ) ) ;
#22425 = VECTOR ( 'NONE', #39355, 1000.000000000000000 ) ;
#22426 = VECTOR ( 'NONE', #27372, 1000.000000000000000 ) ;
#22427 = CARTESIAN_POINT ( 'NONE',  ( 29.32420241873593625, -10.00128497722831611, 20.25080042701565830 ) ) ;
#22428 = VECTOR ( 'NONE', #39359, 1000.000000000000000 ) ;
#22429 = ORIENTED_EDGE ( 'NONE', *, *, #2844, .F. ) ;
#22430 = ADVANCED_FACE ( 'NONE', ( #39814 ), #23585, .F. ) ;
#22431 = CARTESIAN_POINT ( 'NONE',  ( -21.88499642459564853, -5.528038495964381127, -30.00000000000000355 ) ) ;
#22432 = FACE_OUTER_BOUND ( 'NONE', #32501, .T. ) ;
#22433 = ORIENTED_EDGE ( 'NONE', *, *, #17566, .F. ) ;
#22434 = EDGE_CURVE ( 'NONE', #14560, #23343, #3588, .T. ) ;
#22435 = CARTESIAN_POINT ( 'NONE',  ( -11.44473057578096942, 31.45924896672619298, 11.00000000000000000 ) ) ;
#22436 = CARTESIAN_POINT ( 'NONE',  ( -11.17899463792456771, 31.89279561836819710, 10.99387789255783687 ) ) ;
#22437 = CARTESIAN_POINT ( 'NONE',  ( 15.41558956984165363, 26.78481017248027740, -5.000000000000000000 ) ) ;
#22438 = CARTESIAN_POINT ( 'NONE',  ( 3.093609891035674853, 23.47637780903313853, -21.88905062759406306 ) ) ;
#22439 = CARTESIAN_POINT ( 'NONE',  ( -6.506711629694017063, 35.47525137376727855, 10.83333333333333215 ) ) ;
#22440 = EDGE_LOOP ( 'NONE', ( #5852, #1965, #29037, #680 ) ) ;
#22441 = DIRECTION ( 'NONE',  ( 0.000000000000000000, 0.000000000000000000, 1.000000000000000000 ) ) ;
#22442 = CARTESIAN_POINT ( 'NONE',  ( 33.75875814100317029, 2.759858869446390361, 23.00000000000000000 ) ) ;
#22443 = CARTESIAN_POINT ( 'NONE',  ( 28.46220377038417126, -23.29623700624878779, -8.431205218395554368 ) ) ;
#22444 = AXIS2_PLACEMENT_3D ( 'NONE', #22967, #20135, #26620 ) ;
#22445 = DIRECTION ( 'NONE',  ( 0.000000000000000000, 0.000000000000000000, 1.000000000000000000 ) ) ;
#22446 = DIRECTION ( 'NONE',  ( -0.2079116908177655043, -0.9781476007338044676, -0.000000000000000000 ) ) ;
#22447 = DIRECTION ( 'NONE',  ( -0.000000000000000000, -0.000000000000000000, 1.000000000000000000 ) ) ;
#22448 = CARTESIAN_POINT ( 'NONE',  ( 10.76979477178801936, 18.04852582976164044, -26.18016545178095100 ) ) ;
#22449 = DIRECTION ( 'NONE',  ( 0.9781476007338069101, 0.2079116908177532363, 0.000000000000000000 ) ) ;
#22450 = VERTEX_POINT ( 'NONE', #8947 ) ;
#22453 = CARTESIAN_POINT ( 'NONE',  ( -8.910254037844428154, 17.93301270189230223, 10.00000000000000000 ) ) ;
#22452 = CIRCLE ( 'NONE', #432, 1.000000000000000888 ) ;
#22451 = CARTESIAN_POINT ( 'NONE',  ( -17.59337500131034915, 19.37719024453491201, -8.848041657323321374 ) ) ;
#22454 = CARTESIAN_POINT ( 'NONE',  ( 32.84658669524289110, -23.46788009898384075, 10.99999999999997691 ) ) ;
#22455 = AXIS2_PLACEMENT_3D ( 'NONE', #19780, #1495, #20596 ) ;
#22456 = EDGE_CURVE ( 'NONE', #16724, #4132, #19836, .T. ) ;
#22457 = CARTESIAN_POINT ( 'NONE',  ( 11.87964959439185897, -21.48688383848312000, -18.45485520218330677 ) ) ;
#22458 = EDGE_CURVE ( 'NONE', #4444, #32326, #17238, .T. ) ;
#22459 = CARTESIAN_POINT ( 'NONE',  ( 10.14060191828658120, 25.26915018278934255, 10.00000000000000000 ) ) ;
#22460 = CARTESIAN_POINT ( 'NONE',  ( 10.98647152928295156, 17.30743895948372568, -29.34839841643596614 ) ) ;
#22461 = ORIENTED_EDGE ( 'NONE', *, *, #32237, .F. ) ;
#22462 = CARTESIAN_POINT ( 'NONE',  ( 11.00058940542414554, 17.35166013633943649, -28.70672724212847271 ) ) ;
#22463 = ORIENTED_EDGE ( 'NONE', *, *, #6911, .T. ) ;
#22464 = CARTESIAN_POINT ( 'NONE',  ( 21.24426311945340373, 15.07158936841587860, 11.00000000000000000 ) ) ;
#22465 = CARTESIAN_POINT ( 'NONE',  ( -11.17406680738855584, -20.47027838762622665, -20.54295404136550118 ) ) ;
#22466 = CARTESIAN_POINT ( 'NONE',  ( -24.55877074691219164, -28.27742302307168742, 13.32518128616625930 ) ) ;
#22467 = CARTESIAN_POINT ( 'NONE',  ( -29.65485267539152048, -20.48675704930219155, -10.17941642897329224 ) ) ;
#22468 = CARTESIAN_POINT ( 'NONE',  ( -3.392224512981891316, -20.63403223353535410, -25.47406074567986778 ) ) ;
#22469 = CARTESIAN_POINT ( 'NONE',  ( 15.65441761974471113, 25.86232774665390366, -5.946368842702213442 ) ) ;
#22470 = ORIENTED_EDGE ( 'NONE', *, *, #35598, .F. ) ;
#22471 = CARTESIAN_POINT ( 'NONE',  ( 22.11137694095066308, 11.05602416922195630, -7.426733222396916467 ) ) ;
#22472 = LINE ( 'NONE', #7433, #23222 ) ;
#22473 = CARTESIAN_POINT ( 'NONE',  ( -13.80284393768010531, 29.83092525299177566, 16.87380292611440069 ) ) ;
#22474 = ORIENTED_EDGE ( 'NONE', *, *, #32151, .F. ) ;
#22475 = CARTESIAN_POINT ( 'NONE',  ( -32.89022462939520608, -4.305485280278338323, -9.038522573761735401 ) ) ;
#22476 = CARTESIAN_POINT ( 'NONE',  ( -27.25314217027208841, 3.686469637083872541, 16.30093088680831315 ) ) ;
#22477 = ORIENTED_EDGE ( 'NONE', *, *, #35131, .T. ) ;
#22478 = FACE_OUTER_BOUND ( 'NONE', #37464, .T. ) ;
#22479 = CARTESIAN_POINT ( 'NONE',  ( -3.295881626406750087, 9.398963235502531433, 9.500000000000000000 ) ) ;
#22480 = EDGE_CURVE ( 'NONE', #15244, #31324, #35402, .T. ) ;
#22481 = CARTESIAN_POINT ( 'NONE',  ( 20.12997315792683395, -8.847206737175625335, -24.25336459654654320 ) ) ;
#22482 = CARTESIAN_POINT ( 'NONE',  ( 24.65531199400567886, -28.60128534115905552, 11.55979286843931675 ) ) ;
#22483 = AXIS2_PLACEMENT_3D ( 'NONE', #27230, #24178, #21134 ) ;
#22484 = CIRCLE ( 'NONE', #27685, 1.000000000000000000 ) ;
#22485 = ORIENTED_EDGE ( 'NONE', *, *, #2715, .T. ) ;
#22486 = ORIENTED_EDGE ( 'NONE', *, *, #821, .T. ) ;
#22487 = LINE ( 'NONE', #37741, #30101 ) ;
#22488 = CARTESIAN_POINT ( 'NONE',  ( -15.45712587483427924, 26.63597398780867564, -5.000000000000002665 ) ) ;
#22489 = DIRECTION ( 'NONE',  ( -0.000000000000000000, -0.000000000000000000, -1.000000000000000000 ) ) ;
#22490 = EDGE_LOOP ( 'NONE', ( #39972, #34088, #19024, #25400 ) ) ;
#22491 = CARTESIAN_POINT ( 'NONE',  ( -0.7539017812582486933, 38.52547057370831141, -5.435359319770989295 ) ) ;
#22492 = CARTESIAN_POINT ( 'NONE',  ( -7.935776944912362296, 22.65328985282726393, 6.000000000000000000 ) ) ;
#22493 = CARTESIAN_POINT ( 'NONE',  ( -10.03245514394471627, 31.53326318584470656, 7.000000000000000000 ) ) ;
#22494 = DIRECTION ( 'NONE',  ( 1.000000000000000000, 0.000000000000000000, 0.000000000000000000 ) ) ;
#22495 = DIRECTION ( 'NONE',  ( 0.000000000000000000, 0.000000000000000000, 1.000000000000000000 ) ) ;
#22496 = CARTESIAN_POINT ( 'NONE',  ( 2.629601561899394202, 7.723830143584017094, 10.63089969389957545 ) ) ;
#22497 = CARTESIAN_POINT ( 'NONE',  ( 13.78612880735749791, 27.70518701290404451, -10.51413500146422564 ) ) ;
#22498 = DIRECTION ( 'NONE',  ( -0.000000000000000000, -0.000000000000000000, -1.000000000000000000 ) ) ;
#22499 = ORIENTED_EDGE ( 'NONE', *, *, #7760, .T. ) ;
#22501 = CARTESIAN_POINT ( 'NONE',  ( 0.000000000000000000, 22.50000000000000355, 6.000000000000000000 ) ) ;
#22500 = CARTESIAN_POINT ( 'NONE',  ( -18.80902559120175255, 10.24077132063193041, -22.24714609963263001 ) ) ;
#22502 = CARTESIAN_POINT ( 'NONE',  ( 2.166144593658585915, 42.50000000000004974, 22.99999999999999289 ) ) ;
#22503 = CARTESIAN_POINT ( 'NONE',  ( 15.47542781151556213, -26.66463022141588368, -6.416210468062471861 ) ) ;
#22504 = DIRECTION ( 'NONE',  ( 0.8660254037844363761, -0.5000000000000039968, -0.000000000000000000 ) ) ;
#22505 = CARTESIAN_POINT ( 'NONE',  ( 15.20930106813657368, 26.48505469187728423, -7.825161417022220789 ) ) ;
#22506 = CARTESIAN_POINT ( 'NONE',  ( -18.07620401364299667, 24.68088026512193167, -13.58461195433497082 ) ) ;
#22507 = DIRECTION ( 'NONE',  ( 0.9945218953682727347, -0.1045284632676597436, 6.938893903907217334E-15 ) ) ;
#22508 = EDGE_CURVE ( 'NONE', #35497, #13010, #12784, .T. ) ;
#22509 = AXIS2_PLACEMENT_3D ( 'NONE', #18546, #18347, #3101 ) ;
#22510 = CARTESIAN_POINT ( 'NONE',  ( -14.62643312820280528, -15.49996111506702512, -25.77096336785993103 ) ) ;
#22511 = CARTESIAN_POINT ( 'NONE',  ( 5.856590299683157141, -20.17846598857110507, -25.37062753232054746 ) ) ;
#22512 = CARTESIAN_POINT ( 'NONE',  ( 15.10734495844927849, 25.68721481206937085, -9.241857395831049260 ) ) ;
#22513 = CARTESIAN_POINT ( 'NONE',  ( 23.08576052398056078, -15.62326469692720110, -17.60933158146236366 ) ) ;
#22514 = CARTESIAN_POINT ( 'NONE',  ( 13.72527515842283741, 27.95206079998155957, 10.49999999999999822 ) ) ;
#22515 = FACE_OUTER_BOUND ( 'NONE', #1703, .T. ) ;
#22516 = ORIENTED_EDGE ( 'NONE', *, *, #3158, .T. ) ;
#22517 = CARTESIAN_POINT ( 'NONE',  ( -6.983932559990830846, 26.21054456205356331, -17.77984188425750389 ) ) ;
#22518 = CONICAL_SURFACE ( 'NONE', #12785, 1.000000000000013101, 0.7853981633974582710 ) ;
#22519 = DIRECTION ( 'NONE',  ( 0.6691306063588569053, -0.7431448254773954654, 0.000000000000000000 ) ) ;
#22520 = ORIENTED_EDGE ( 'NONE', *, *, #17791, .F. ) ;
#22521 = CARTESIAN_POINT ( 'NONE',  ( 30.22229184125601265, -0.02826660990534823545, -8.765447815367933160 ) ) ;
#22522 = DIRECTION ( 'NONE',  ( -0.000000000000000000, -0.000000000000000000, -1.000000000000000000 ) ) ;
#22523 = DIRECTION ( 'NONE',  ( -0.000000000000000000, -0.000000000000000000, -1.000000000000000000 ) ) ;
#22524 = ORIENTED_EDGE ( 'NONE', *, *, #15585, .T. ) ;
#22525 = CARTESIAN_POINT ( 'NONE',  ( -26.41186682634353389, 0.4197715753672409678, -15.46164128583599329 ) ) ;
#22526 = CARTESIAN_POINT ( 'NONE',  ( -11.41268156625113406, 18.79179606750104981, 13.00000000000000178 ) ) ;
#22527 = EDGE_CURVE ( 'NONE', #30503, #4287, #34329, .T. ) ;
#22528 = EDGE_LOOP ( 'NONE', ( #23919, #24175, #14542, #35755 ) ) ;
#22529 = CARTESIAN_POINT ( 'NONE',  ( 33.51572963880570910, -7.992457164366485678, -9.832202616107817761 ) ) ;
#22530 = EDGE_CURVE ( 'NONE', #10650, #1084, #27217, .T. ) ;
#22531 = ORIENTED_EDGE ( 'NONE', *, *, #38206, .F. ) ;
#22532 = CARTESIAN_POINT ( 'NONE',  ( 0.000000000000000000, 0.000000000000000000, 0.000000000000000000 ) ) ;
#22533 = CARTESIAN_POINT ( 'NONE',  ( -13.80290580123972966, 34.21636679304910444, 11.55979286843966314 ) ) ;
#22534 = DIRECTION ( 'NONE',  ( -1.000000000000000000, 0.000000000000000000, 0.000000000000000000 ) ) ;
#22535 = LINE ( 'NONE', #10562, #4650 ) ;
#22536 = CARTESIAN_POINT ( 'NONE',  ( 2.498547013092441649, 33.82729453933308150, 19.66345542862528006 ) ) ;
#22537 = AXIS2_PLACEMENT_3D ( 'NONE', #38425, #7744, #7542 ) ;
#22538 = AXIS2_PLACEMENT_3D ( 'NONE', #9450, #25280, #34430 ) ;
#22539 = ADVANCED_FACE ( 'NONE', ( #25370 ), #37984, .T. ) ;
#22540 = DIRECTION ( 'NONE',  ( -0.000000000000000000, 0.000000000000000000, 1.000000000000000000 ) ) ;
#22541 = ORIENTED_EDGE ( 'NONE', *, *, #16104, .F. ) ;
#22542 = SURFACE_SIDE_STYLE ('',( #20116 ) ) ;
#22543 = CARTESIAN_POINT ( 'NONE',  ( 3.992867117591230919, 8.524771480177550487, 7.499999999999990230 ) ) ;
#22544 = CYLINDRICAL_SURFACE ( 'NONE', #68, 0.4999999999999997780 ) ;
#22545 = AXIS2_PLACEMENT_3D ( 'NONE', #24695, #37092, #9259 ) ;
#22546 = DIRECTION ( 'NONE',  ( -0.000000000000000000, -0.000000000000000000, -1.000000000000000000 ) ) ;
#22547 = CARTESIAN_POINT ( 'NONE',  ( 17.71135169000040932, 20.05059954136391553, -5.477262195481070073 ) ) ;
#22548 = AXIS2_PLACEMENT_3D ( 'NONE', #15943, #19381, #31780 ) ;
#22549 = CARTESIAN_POINT ( 'NONE',  ( 11.56236212135367047, 32.93568925309087803, -7.647066273184269569 ) ) ;
#22550 = ORIENTED_EDGE ( 'NONE', *, *, #1768, .F. ) ;
#22551 = CARTESIAN_POINT ( 'NONE',  ( 10.21873439408511253, -18.03641402610821842, -27.40419155213225721 ) ) ;
#22552 = DIRECTION ( 'NONE',  ( -0.000000000000000000, -0.000000000000000000, -1.000000000000000000 ) ) ;
#22553 = B_SPLINE_CURVE_WITH_KNOTS ( 'NONE', 3,
 ( #36166, #38808, #23372, #10984, #7922, #29663, #39006, #20736, #11182 ),
 .UNSPECIFIED., .F., .F.,
 ( 4, 1, 1, 1, 1, 1, 4 ),
 ( 0.3034822677883343145, 0.3750000000143087764, 0.4999999999999940048, 0.6249999999856795663, 0.7499999999713649057, 0.8749999999570503562, 1.000000000000000000 ),
 .UNSPECIFIED. ) ;
#22554 = EDGE_CURVE ( 'NONE', #29633, #27849, #6285, .T. ) ;
#22555 = DIRECTION ( 'NONE',  ( -0.7431448254773863615, 0.6691306063588670083, 0.000000000000000000 ) ) ;
#22556 = EDGE_CURVE ( 'NONE', #4057, #36810, #37850, .T. ) ;
#22557 = ORIENTED_EDGE ( 'NONE', *, *, #28240, .F. ) ;
#22558 = CARTESIAN_POINT ( 'NONE',  ( -15.02206552268004458, 25.95591568151323969, -9.238934606167955366 ) ) ;
#22559 = CARTESIAN_POINT ( 'NONE',  ( -35.63595018118445523, -14.50160624002370469, 15.72805884748939143 ) ) ;
#22560 = CARTESIAN_POINT ( 'NONE',  ( 9.296951271124752836, -18.31947431080797628, -28.71563296508281482 ) ) ;
#22561 = DIRECTION ( 'NONE',  ( 1.000000000000000000, 0.000000000000000000, 0.000000000000000000 ) ) ;
#22562 = EDGE_LOOP ( 'NONE', ( #16707, #27030, #11116, #32142 ) ) ;
#22563 = VERTEX_POINT ( 'NONE', #12189 ) ;
#22564 = AXIS2_PLACEMENT_3D ( 'NONE', #25211, #18723, #19313 ) ;
#22565 = CARTESIAN_POINT ( 'NONE',  ( -13.55309326636294109, 29.69719733569533915, -8.626781295736174471 ) ) ;
#22566 = DIRECTION ( 'NONE',  ( -0.9510565162951503115, 0.3090169943749572767, 0.000000000000000000 ) ) ;
#22567 = FACE_BOUND ( 'NONE', #21225, .T. ) ;
#22568 = AXIS2_PLACEMENT_3D ( 'NONE', #2260, #29483, #14650 ) ;
#22569 = AXIS2_PLACEMENT_3D ( 'NONE', #4345, #13279, #19379 ) ;
#22570 = CARTESIAN_POINT ( 'NONE',  ( -35.11052852875971553, -8.727991070938342588, -6.744352222248348738 ) ) ;
#22571 = LINE ( 'NONE', #35173, #36513 ) ;
#22572 = ORIENTED_EDGE ( 'NONE', *, *, #8280, .F. ) ;
#22573 = CARTESIAN_POINT ( 'NONE',  ( 20.80244950058357034, 0.9809649937616239379, -26.84207219552697410 ) ) ;
#22574 = CARTESIAN_POINT ( 'NONE',  ( 14.42035624161478857, 26.65972665747660386, 10.63089969389957190 ) ) ;
#22575 = CARTESIAN_POINT ( 'NONE',  ( 1.358225888363031819, 11.68927977431952137, 13.00000000000000178 ) ) ;
#22576 = CIRCLE ( 'NONE', #20010, 0.5000000000000004441 ) ;
#22577 = ORIENTED_EDGE ( 'NONE', *, *, #27197, .T. ) ;
#22578 = CARTESIAN_POINT ( 'NONE',  ( -29.59593009434644983, 0.04982597378002901617, -10.18041819265831549 ) ) ;
#22579 = CARTESIAN_POINT ( 'NONE',  ( -39.31168172498703939, -14.28874104167793035, 11.00000000000000000 ) ) ;
#22580 = EDGE_CURVE ( 'NONE', #1489, #4691, #27828, .T. ) ;
#22581 = ORIENTED_EDGE ( 'NONE', *, *, #32395, .F. ) ;
#22582 = CARTESIAN_POINT ( 'NONE',  ( 33.36633864933632054, -3.217268494394103673, -5.000000000000000000 ) ) ;
#22583 = VECTOR ( 'NONE', #22725, 1000.000000000000000 ) ;
#22584 = DIRECTION ( 'NONE',  ( 0.9135454576426059736, 0.4067366430757888285, -0.000000000000000000 ) ) ;
#22585 = CARTESIAN_POINT ( 'NONE',  ( 34.55475982899568521, -10.97206003969012755, 17.42190598798391932 ) ) ;
#22586 = EDGE_CURVE ( 'NONE', #14121, #4988, #32811, .T. ) ;
#22587 = ORIENTED_EDGE ( 'NONE', *, *, #5658, .T. ) ;
#22588 = CARTESIAN_POINT ( 'NONE',  ( -6.751265526281039264, 37.11581529111845867, 16.30093088680186142 ) ) ;
#22589 = CARTESIAN_POINT ( 'NONE',  ( 2.494936919103933448, 34.23777120880591696, 6.000000000000000000 ) ) ;
#22590 = CARTESIAN_POINT ( 'NONE',  ( 2.442402655125668787, 27.78651631404541789, 21.00000000000000355 ) ) ;
#22591 = DIRECTION ( 'NONE',  ( -0.4999999999999921729, 0.8660254037844432595, 0.000000000000000000 ) ) ;
#22592 = DIRECTION ( 'NONE',  ( 0.000000000000000000, 0.000000000000000000, 1.000000000000000000 ) ) ;
#22593 = AXIS2_PLACEMENT_3D ( 'NONE', #15399, #11754, #18256 ) ;
#22594 = AXIS2_PLACEMENT_3D ( 'NONE', #17510, #17106, #14439 ) ;
#22595 = FACE_BOUND ( 'NONE', #1612, .T. ) ;
#22596 = CARTESIAN_POINT ( 'NONE',  ( 16.78686424248630615, 15.93842542257170258, 18.42518152272128518 ) ) ;
#22597 = CARTESIAN_POINT ( 'NONE',  ( -23.58808727774059832, 8.960771098271621327, -5.481298557163171381 ) ) ;
#22598 = CARTESIAN_POINT ( 'NONE',  ( 18.77937622075242530, -23.29516096719056861, -14.07484684245071982 ) ) ;
#22599 = CIRCLE ( 'NONE', #5104, 0.5000000000000004441 ) ;
#22600 = CARTESIAN_POINT ( 'NONE',  ( 4.348106467989403257, 35.16482219193073178, 13.00000000000000178 ) ) ;
#22601 = ORIENTED_EDGE ( 'NONE', *, *, #26999, .F. ) ;
#22602 = CARTESIAN_POINT ( 'NONE',  ( 15.32234214663592375, 26.84634284219205824, -6.414409059685876713 ) ) ;
#22603 = AXIS2_PLACEMENT_3D ( 'NONE', #22278, #34683, #26133 ) ;
#22604 = ORIENTED_EDGE ( 'NONE', *, *, #7069, .T. ) ;
#22605 = CARTESIAN_POINT ( 'NONE',  ( -13.03496280190833723, 19.64411286304471815, -19.60530794096396434 ) ) ;
#22606 = CARTESIAN_POINT ( 'NONE',  ( -29.47277113412615179, -17.01611234805157480, 19.66345542862529072 ) ) ;
#22607 = FACE_OUTER_BOUND ( 'NONE', #34580, .T. ) ;
#22608 = CARTESIAN_POINT ( 'NONE',  ( 11.92636920872155670, 19.34590550356041305, -21.62300054144612460 ) ) ;
#22609 = EDGE_LOOP ( 'NONE', ( #8342, #10431, #21358 ) ) ;
#22610 = CARTESIAN_POINT ( 'NONE',  ( 18.81768709236329329, -9.658926806160746281, -26.25942549260763670 ) ) ;
#22611 = ADVANCED_FACE ( 'NONE', ( #24582 ), #18492, .F. ) ;
#22612 = DIRECTION ( 'NONE',  ( -0.8660254037844432595, -0.4999999999999920064, 0.000000000000000000 ) ) ;
#22613 = ORIENTED_EDGE ( 'NONE', *, *, #15719, .T. ) ;
#22615 = FACE_OUTER_BOUND ( 'NONE', #9435, .T. ) ;
#22614 = CARTESIAN_POINT ( 'NONE',  ( -11.24118742064583998, 18.64458347442174713, -23.81550990468068107 ) ) ;
#22616 = CARTESIAN_POINT ( 'NONE',  ( -16.68682434244347590, -26.92965747703111390, -6.397897022492878172 ) ) ;
#22617 = DIRECTION ( 'NONE',  ( 0.9510565162951507556, -0.3090169943749560000, -2.144236138472114690E-15 ) ) ;
#22618 = ORIENTED_EDGE ( 'NONE', *, *, #28935, .T. ) ;
#22619 = CARTESIAN_POINT ( 'NONE',  ( -22.46715076204040429, -10.09974697177796088, -20.72078323234527630 ) ) ;
#22620 = CARTESIAN_POINT ( 'NONE',  ( -9.971190107407892356, -19.73728639792070538, -22.80224159634297720 ) ) ;
#22621 = DIRECTION ( 'NONE',  ( 1.000000000000000000, 0.000000000000000000, 0.000000000000000000 ) ) ;
#22622 = CARTESIAN_POINT ( 'NONE',  ( 13.88678101316755864, 18.51693486955983659, -19.73415532929779914 ) ) ;
#22623 = ORIENTED_EDGE ( 'NONE', *, *, #15575, .T. ) ;
#22624 = CARTESIAN_POINT ( 'NONE',  ( 23.90103726830303899, 3.753447309722855785, -16.71722843108891965 ) ) ;
#22625 = DIRECTION ( 'NONE',  ( 1.000000000000000000, 0.000000000000000000, 0.000000000000000000 ) ) ;
#22626 = DIRECTION ( 'NONE',  ( 0.000000000000000000, 0.000000000000000000, 1.000000000000000000 ) ) ;
#22627 = VERTEX_POINT ( 'NONE', #25181 ) ;
#22628 = CARTESIAN_POINT ( 'NONE',  ( -20.73211841591003690, 0.1678577862357426842, -27.40417673715113978 ) ) ;
#22629 = CARTESIAN_POINT ( 'NONE',  ( 29.33018326755770744, -0.4255386876862592427, -11.55134619685823516 ) ) ;
#22630 = AXIS2_PLACEMENT_3D ( 'NONE', #40151, #33681, #12325 ) ;
#22631 = CARTESIAN_POINT ( 'NONE',  ( 29.36302367423321869, -15.61102309902083185, 19.99202127657103389 ) ) ;
#22632 = ORIENTED_EDGE ( 'NONE', *, *, #11715, .F. ) ;
#22633 = VECTOR ( 'NONE', #25245, 999.9999999999998863 ) ;
#22634 = CARTESIAN_POINT ( 'NONE',  ( -13.28992586503615669, -18.25382200079944539, -20.55760979252988463 ) ) ;
#22635 = DIRECTION ( 'NONE',  ( 0.000000000000000000, 0.000000000000000000, 1.000000000000000000 ) ) ;
#22636 = EDGE_CURVE ( 'NONE', #37407, #2419, #25641, .T. ) ;
#22637 = LINE ( 'NONE', #19393, #35349 ) ;
#22638 = DIRECTION ( 'NONE',  ( -1.224646799147351235E-16, 1.000000000000000000, 0.000000000000000000 ) ) ;
#22639 = LINE ( 'NONE', #19808, #29438 ) ;
#22640 = CARTESIAN_POINT ( 'NONE',  ( 14.52509594610761923, 21.97885917798724975, 11.00000000000000000 ) ) ;
#22641 = ORIENTED_EDGE ( 'NONE', *, *, #26286, .T. ) ;
#22642 = DIRECTION ( 'NONE',  ( 1.000000000000000000, 0.000000000000000000, 0.000000000000000000 ) ) ;
#22643 = CARTESIAN_POINT ( 'NONE',  ( 3.503793317224320969, 8.420815634768672453, 11.00000000000000000 ) ) ;
#22644 = CARTESIAN_POINT ( 'NONE',  ( 15.88542612224667927, -12.95767258840383107, -29.22532221307605838 ) ) ;
#22645 = FACE_OUTER_BOUND ( 'NONE', #31629, .T. ) ;
#22646 = DIRECTION ( 'NONE',  ( -0.000000000000000000, -0.000000000000000000, -1.000000000000000000 ) ) ;
#22647 = CARTESIAN_POINT ( 'NONE',  ( 13.80587148021421484, 24.46212733322120414, -13.46414252330034778 ) ) ;
#22648 = CARTESIAN_POINT ( 'NONE',  ( -6.064571727552472424, 31.45661825943146894, 13.00000000000000178 ) ) ;
#22649 = AXIS2_PLACEMENT_3D ( 'NONE', #28548, #31796, #18816 ) ;
#22650 = ORIENTED_EDGE ( 'NONE', *, *, #36353, .F. ) ;
#22651 = CARTESIAN_POINT ( 'NONE',  ( -14.63038540974646828, 16.30325065141676077, -22.01182681179342637 ) ) ;
#22652 = DIRECTION ( 'NONE',  ( 0.000000000000000000, -0.000000000000000000, 1.000000000000000000 ) ) ;
#22653 = EDGE_CURVE ( 'NONE', #38699, #3260, #21763, .T. ) ;
#22654 = CARTESIAN_POINT ( 'NONE',  ( 15.29084952668607933, -26.49705136638473846, -7.357960102425458615 ) ) ;
#22655 = CARTESIAN_POINT ( 'NONE',  ( 12.68475447279711510, 27.14725768220934654, 9.500000000000000000 ) ) ;
#22656 = CARTESIAN_POINT ( 'NONE',  ( 11.12160456634172512, 17.61533166272547035, -26.83009323505500987 ) ) ;
#22657 = VERTEX_POINT ( 'NONE', #28422 ) ;
#22658 = CARTESIAN_POINT ( 'NONE',  ( 13.76332498804387861, 23.40953749546633134, -14.47517996330730305 ) ) ;
#22659 = AXIS2_PLACEMENT_3D ( 'NONE', #24199, #20770, #33164 ) ;
#22660 = PRODUCT_DEFINITION_SHAPE ( 'NONE', 'NONE',  #40203 ) ;
#22661 = EDGE_LOOP ( 'NONE', ( #2224, #20094, #8277, #35591 ) ) ;
#22663 = CARTESIAN_POINT ( 'NONE',  ( 14.12406941186438125, 26.56345723075634524, 10.96580508970281009 ) ) ;
#22662 = CARTESIAN_POINT ( 'NONE',  ( -12.08249424194362120, 19.98192381863790956, -20.53110637240889602 ) ) ;
#22664 = CARTESIAN_POINT ( 'NONE',  ( -9.594949128275974459, -18.35353841803804542, -27.44967104049570850 ) ) ;
#22665 = CARTESIAN_POINT ( 'NONE',  ( -18.86506720475286514, -28.79250143785268534, 13.92931973827851522 ) ) ;
#22666 = CARTESIAN_POINT ( 'NONE',  ( -18.49734238951277732, -11.93560065676270021, -24.22553531776692992 ) ) ;
#22667 = CARTESIAN_POINT ( 'NONE',  ( -3.697151520580219231, -21.53368035006806380, -21.12883000117165366 ) ) ;
#22668 = CARTESIAN_POINT ( 'NONE',  ( 15.49389368908896714, 25.54012532978367389, -7.832773519083336744 ) ) ;
#22669 = EDGE_CURVE ( 'NONE', #10635, #39810, #13325, .T. ) ;
#22670 = ORIENTED_EDGE ( 'NONE', *, *, #31912, .T. ) ;
#22671 = CARTESIAN_POINT ( 'NONE',  ( 18.94224516238102396, 8.015443379958615111, -28.28845633141069627 ) ) ;
#22672 = CARTESIAN_POINT ( 'NONE',  ( -33.75875814100324845, 2.759858869446484064, 3.000000000000000000 ) ) ;
#22673 = CARTESIAN_POINT ( 'NONE',  ( -15.46713722816187975, -26.73718067935205056, -5.000000000000000000 ) ) ;
#22674 = EDGE_CURVE ( 'NONE', #10078, #3614, #37373, .T. ) ;
#22675 = CARTESIAN_POINT ( 'NONE',  ( 10.35750558343008798, 33.44896173338925394, 17.42190598798391932 ) ) ;
#22676 = VERTEX_POINT ( 'NONE', #599 ) ;
#22677 = CARTESIAN_POINT ( 'NONE',  ( -23.36115073782027096, -2.173507815852580016, -21.26580309426782733 ) ) ;
#22678 = CARTESIAN_POINT ( 'NONE',  ( -17.92566989744610950, 16.47414500506816992, 17.42190598798358181 ) ) ;
#22679 = ORIENTED_EDGE ( 'NONE', *, *, #24599, .F. ) ;
#22680 = CARTESIAN_POINT ( 'NONE',  ( 21.91981567634952910, -15.65087685632039793, 20.99999999999999645 ) ) ;
#22681 = CARTESIAN_POINT ( 'NONE',  ( 10.14716901145161465, 12.46304090461738667, 6.000000000000000000 ) ) ;
#22682 = CARTESIAN_POINT ( 'NONE',  ( 34.43848434938189484, -16.34293750617152696, -6.699837301618770447 ) ) ;
#22683 = CARTESIAN_POINT ( 'NONE',  ( 33.53883321253825756, -0.1552552779180596254, 12.73282698324945805 ) ) ;
#22684 = EDGE_CURVE ( 'NONE', #6323, #7643, #1809, .T. ) ;
#22685 = ORIENTED_EDGE ( 'NONE', *, *, #23538, .F. ) ;
#22686 = ADVANCED_FACE ( 'NONE', ( #36091 ), #17413, .F. ) ;
#22687 = VERTEX_POINT ( 'NONE', #5403 ) ;
#22688 = ADVANCED_FACE ( 'NONE', ( #26738 ), #20250, .T. ) ;
#22689 = VECTOR ( 'NONE', #25741, 1000.000000000000000 ) ;
#22690 = CARTESIAN_POINT ( 'NONE',  ( 10.78893975237932956, 23.27376113029817617, 12.00000000000000000 ) ) ;
#22691 = CARTESIAN_POINT ( 'NONE',  ( -28.92287456554050351, 1.976372635573284242, -5.000000000000000000 ) ) ;
#22692 = DIRECTION ( 'NONE',  ( -1.000000000000000000, 0.000000000000000000, 0.000000000000000000 ) ) ;
#22693 = ORIENTED_EDGE ( 'NONE', *, *, #3800, .T. ) ;
#22694 = CARTESIAN_POINT ( 'NONE',  ( -0.4022046384660851182, 20.75372784789253799, -27.70456478907405184 ) ) ;
#22695 = DIRECTION ( 'NONE',  ( 0.1045284632676437703, -0.9945218953682742891, 0.000000000000000000 ) ) ;
#22696 = CARTESIAN_POINT ( 'NONE',  ( 14.11133924723984379, 27.61078317377176106, 10.63089969389956480 ) ) ;
#22697 = LINE ( 'NONE', #28599, #2665 ) ;
#22698 = DIRECTION ( 'NONE',  ( -0.000000000000000000, 0.000000000000000000, 1.000000000000000000 ) ) ;
#22699 = CARTESIAN_POINT ( 'NONE',  ( -10.63499050845675775, 32.74860482968701092, 10.94611345180490680 ) ) ;
#22700 = CARTESIAN_POINT ( 'NONE',  ( 14.46705284293606120, 29.28167841381910463, -5.921992419550550224 ) ) ;
#22701 = CARTESIAN_POINT ( 'NONE',  ( 1.605696033269625955, 17.55816537872232530, 12.00000000000000000 ) ) ;
#22702 = ORIENTED_EDGE ( 'NONE', *, *, #19562, .F. ) ;
#22704 = DIRECTION ( 'NONE',  ( -0.6691306063588671194, -0.7431448254773863615, 0.000000000000000000 ) ) ;
#22703 = CARTESIAN_POINT ( 'NONE',  ( -16.81891822627442323, 11.75299315897373731, -28.85843616979807535 ) ) ;
#22705 = DIRECTION ( 'NONE',  ( 0.000000000000000000, 0.000000000000000000, -1.000000000000000000 ) ) ;
#22706 = CARTESIAN_POINT ( 'NONE',  ( 15.22463038672936086, -26.29468693911994848, -8.295888942704511493 ) ) ;
#22707 = CARTESIAN_POINT ( 'NONE',  ( -3.784955426773653375, 9.502919080911414795, 10.50000000000000000 ) ) ;
#22708 = CARTESIAN_POINT ( 'NONE',  ( 11.00364732032666382, 17.44887877622111461, -28.07524110270195195 ) ) ;
#22709 = CARTESIAN_POINT ( 'NONE',  ( -21.88444403592365362, 6.126538576424530369, -21.50719306941233455 ) ) ;
#22710 = EDGE_CURVE ( 'NONE', #6233, #31812, #15129, .T. ) ;
#22711 = CYLINDRICAL_SURFACE ( 'NONE', #33675, 16.00000000000000711 ) ;
#22712 = CARTESIAN_POINT ( 'NONE',  ( -15.98951276118712883, -15.93656576511519951, -23.18934444843043607 ) ) ;
#22713 = CARTESIAN_POINT ( 'NONE',  ( 5.693958622330683284, -19.87604177814888473, -27.65608055801159892 ) ) ;
#22714 = CARTESIAN_POINT ( 'NONE',  ( 15.31836689275630370, 26.11603314008040400, -7.829368276863946541 ) ) ;
#22715 = CARTESIAN_POINT ( 'NONE',  ( 18.88587872898141740, 12.68145420873708851, -16.97363421066873812 ) ) ;
#22716 = DIRECTION ( 'NONE',  ( 1.000000000000000000, 0.000000000000000000, 0.000000000000000000 ) ) ;
#22717 = DIRECTION ( 'NONE',  ( 1.000000000000000000, 0.000000000000000000, 0.000000000000000000 ) ) ;
#22718 = EDGE_LOOP ( 'NONE', ( #35079, #20866, #25460, #26716 ) ) ;
#22719 = CIRCLE ( 'NONE', #28550, 6.000000000000014211 ) ;
#22720 = CARTESIAN_POINT ( 'NONE',  ( -9.379895652603979173, 35.46246444712465973, -5.000000000000002665 ) ) ;
#22721 = VERTEX_POINT ( 'NONE', #17002 ) ;
#22722 = DIRECTION ( 'NONE',  ( -0.000000000000000000, -0.000000000000000000, -1.000000000000000000 ) ) ;
#22723 = ORIENTED_EDGE ( 'NONE', *, *, #20058, .F. ) ;
#22724 = CARTESIAN_POINT ( 'NONE',  ( 20.81719713451408893, 0.8112600457793633923, -26.82911930713009241 ) ) ;
#22725 = DIRECTION ( 'NONE',  ( 0.000000000000000000, 0.000000000000000000, -1.000000000000000000 ) ) ;
#22726 = DIRECTION ( 'NONE',  ( 1.000000000000000000, 0.000000000000000000, 0.000000000000000000 ) ) ;
#22727 = ORIENTED_EDGE ( 'NONE', *, *, #40040, .F. ) ;
#22728 = CARTESIAN_POINT ( 'NONE',  ( -22.19870942614620901, 0.7548860820614724521, -22.74607621399518465 ) ) ;
#22729 = CARTESIAN_POINT ( 'NONE',  ( -20.49308933001933397, -27.11270025041355680, -6.352872742357712710 ) ) ;
#22730 = EDGE_LOOP ( 'NONE', ( #11634, #25220, #31391, #13277, #34722 ) ) ;
#22731 = CARTESIAN_POINT ( 'NONE',  ( 34.06363962356728337, -8.139266223780131426, -8.939444182090305446 ) ) ;
#22732 = VECTOR ( 'NONE', #39938, 1000.000000000000000 ) ;
#22733 = ORIENTED_EDGE ( 'NONE', *, *, #10603, .F. ) ;
#22734 = APPLICATION_PROTOCOL_DEFINITION ( 'draft international standard', 'automotive_design', 1998, #24134 ) ;
#22735 = CARTESIAN_POINT ( 'NONE',  ( 9.340438144417221977, 38.00965938232028662, 11.00000000000005151 ) ) ;
#22736 = EDGE_CURVE ( 'NONE', #30411, #4180, #23293, .T. ) ;
#22737 = CARTESIAN_POINT ( 'NONE',  ( 13.94482798346721175, 26.50521816028912525, 11.00000000000000000 ) ) ;
#22738 = CARTESIAN_POINT ( 'NONE',  ( 8.401171878996485987, 21.11424711454080594, 9.000000000000001776 ) ) ;
#22739 = EDGE_CURVE ( 'NONE', #40053, #17409, #12813, .T. ) ;
#22740 = CARTESIAN_POINT ( 'NONE',  ( 6.372562348371962671, 33.08234073371033190, 19.27171037444156809 ) ) ;
#22741 = CYLINDRICAL_SURFACE ( 'NONE', #17501, 1.000000000000000000 ) ;
#22742 = ORIENTED_EDGE ( 'NONE', *, *, #29113, .F. ) ;
#22743 =( NAMED_UNIT ( * ) PLANE_ANGLE_UNIT ( ) SI_UNIT ( $, .RADIAN. ) );
#22744 = CARTESIAN_POINT ( 'NONE',  ( 2.406372317666654492, 20.36914331218811824, -30.00000000000001776 ) ) ;
#22745 = DIRECTION ( 'NONE',  ( -1.000000000000000000, 0.000000000000000000, 0.000000000000000000 ) ) ;
#22746 = CARTESIAN_POINT ( 'NONE',  ( -28.79337657216479940, 4.963436916928028353, 11.00000000000544276 ) ) ;
#22747 = CARTESIAN_POINT ( 'NONE',  ( 17.71135169000040932, 20.05059954136391553, -5.000000000000002665 ) ) ;
#22748 = CARTESIAN_POINT ( 'NONE',  ( 6.687105839631831472, 20.72947162859387404, -24.48960877912796263 ) ) ;
#22749 = EDGE_LOOP ( 'NONE', ( #27264, #3822, #11393, #39654, #5466, #10287 ) ) ;
#22750 = CARTESIAN_POINT ( 'NONE',  ( -18.23649648353780961, -16.09146789626143814, 20.99999999999999645 ) ) ;
#22751 = CARTESIAN_POINT ( 'NONE',  ( 11.44473057578109199, 31.45924896672603310, 7.499999999999997335 ) ) ;
#22752 = CARTESIAN_POINT ( 'NONE',  ( 16.20011322261754216, -26.49736879530895806, -8.260367887910364360 ) ) ;
#22753 = CARTESIAN_POINT ( 'NONE',  ( 7.111215932167702647, 17.81698729810774751, 9.000000000000001776 ) ) ;
#22754 = CARTESIAN_POINT ( 'NONE',  ( 12.39463915635820612, 18.33192650902018883, 13.00000000000000178 ) ) ;
#22755 = EDGE_CURVE ( 'NONE', #26378, #6957, #38730, .T. ) ;
#22756 = VERTEX_POINT ( 'NONE', #17207 ) ;
#22757 = CARTESIAN_POINT ( 'NONE',  ( -15.37168272651113199, 26.67356397381335142, -6.417197371198677835 ) ) ;
#22758 = AXIS2_PLACEMENT_3D ( 'NONE', #27853, #19502, #624 ) ;
#22759 = CARTESIAN_POINT ( 'NONE',  ( -32.49165476041793710, -0.9821698610459400625, 15.72805884748929373 ) ) ;
#22760 = CARTESIAN_POINT ( 'NONE',  ( 11.13984957941081433, -21.02844965650029962, -19.53953216799471448 ) ) ;
#22761 = ADVANCED_FACE ( 'NONE', ( #5002 ), #39124, .F. ) ;
#22762 = EDGE_CURVE ( 'NONE', #21433, #8840, #26541, .T. ) ;
#22763 = CARTESIAN_POINT ( 'NONE',  ( 33.75875814100317029, 2.759858869446390361, 11.00000000000000000 ) ) ;
#22764 = VERTEX_POINT ( 'NONE', #35484 ) ;
#22765 = VERTEX_POINT ( 'NONE', #7641 ) ;
#22766 = CARTESIAN_POINT ( 'NONE',  ( -12.12099249900222731, 26.27303737746609613, -14.20430146812667083 ) ) ;
#22767 = LINE ( 'NONE', #7325, #37302 ) ;
#22768 = FACE_BOUND ( 'NONE', #19164, .T. ) ;
#22769 = EDGE_CURVE ( 'NONE', #24692, #21186, #39438, .T. ) ;
#22770 = CARTESIAN_POINT ( 'NONE',  ( -34.38052266744621477, -7.499778090769174455, -8.068316597692506420 ) ) ;
#22771 = DIRECTION ( 'NONE',  ( -0.2079116908177688350, -0.9781476007338035794, 0.000000000000000000 ) ) ;
#22772 = VERTEX_POINT ( 'NONE', #11309 ) ;
#22773 = CARTESIAN_POINT ( 'NONE',  ( 20.52133710794606358, 0.9695505216964825923, -28.71086575011983300 ) ) ;
#22774 = CARTESIAN_POINT ( 'NONE',  ( 15.34996087503667361, 26.64851995519817152, -6.887892877121212010 ) ) ;
#22775 = CARTESIAN_POINT ( 'NONE',  ( 14.97283176289962903, 21.60377111278808471, 10.49999999999999822 ) ) ;
#22776 = VECTOR ( 'NONE', #24562, 1000.000000000000000 ) ;
#22777 = EDGE_LOOP ( 'NONE', ( #2820, #30750, #39759, #10155 ) ) ;
#22778 = CARTESIAN_POINT ( 'NONE',  ( -30.35055362032863613, -0.002292147019176501987, -8.297710457928772598 ) ) ;
#22779 = FACE_OUTER_BOUND ( 'NONE', #3928, .T. ) ;
#22780 = EDGE_LOOP ( 'NONE', ( #39294, #19940, #13211 ) ) ;
#22781 = CARTESIAN_POINT ( 'NONE',  ( 24.63269681886077223, -1.423661518239742518, -19.25494299242245688 ) ) ;
#22782 = CARTESIAN_POINT ( 'NONE',  ( -1.587667106213708879, 35.31811204475769728, 12.00000000000000000 ) ) ;
#22783 = CARTESIAN_POINT ( 'NONE',  ( 23.94800771174125842, -26.22823558801567145, 16.87380292611481636 ) ) ;
#22784 = ORIENTED_EDGE ( 'NONE', *, *, #34446, .F. ) ;
#22785 = CARTESIAN_POINT ( 'NONE',  ( -1.824109939552144288, 39.35700678546971432, 15.13084544680213561 ) ) ;
#22786 = B_SPLINE_CURVE_WITH_KNOTS ( 'NONE', 3,
 ( #38360, #26576, #13775, #1796, #20085, #31862, #10531, #26167, #22914, #38966, #35115, #10945, #35315, #35922, #7474, #38763, #28816, #38561 ),
 .UNSPECIFIED., .F., .F.,
 ( 4, 2, 2, 2, 2, 2, 2, 2, 4 ),
 ( 0.000000000000000000, 0.1249999999999998335, 0.2499999999999996669, 0.3749999999999995004, 0.4999999999999993339, 0.6249999999999994449, 0.7499999999999996669, 0.8749999999999997780, 1.000000000000000000 ),
 .UNSPECIFIED. ) ;
#22787 = EDGE_CURVE ( 'NONE', #33978, #32396, #10884, .T. ) ;
#22788 = EDGE_CURVE ( 'NONE', #4338, #39554, #24499, .T. ) ;
#22789 = DIRECTION ( 'NONE',  ( 0.000000000000000000, 0.000000000000000000, -1.000000000000000000 ) ) ;
#22790 = ADVANCED_FACE ( 'NONE', ( #14547 ), #23689, .T. ) ;
#22791 = CARTESIAN_POINT ( 'NONE',  ( -4.143025606350054302E-14, 27.50000000000004974, 20.99999999999998934 ) ) ;
#22792 = AXIS2_PLACEMENT_3D ( 'NONE', #36356, #8519, #24359 ) ;
#22793 = DIRECTION ( 'NONE',  ( 0.000000000000000000, 0.000000000000000000, 1.000000000000000000 ) ) ;
#22794 = VECTOR ( 'NONE', #5064, 1000.000000000000114 ) ;
#22795 = CARTESIAN_POINT ( 'NONE',  ( -8.249569378970276645, 9.971997865784310022, 7.485646746502372828 ) ) ;
#22796 = FACE_BOUND ( 'NONE', #33000, .T. ) ;
#22797 = CARTESIAN_POINT ( 'NONE',  ( 15.85745926881093304, 21.40218184472425023, 17.42190598797886025 ) ) ;
#22798 = CARTESIAN_POINT ( 'NONE',  ( -19.81925457214680719, 7.205556427748036619, -24.35504295706233790 ) ) ;
#22799 = AXIS2_PLACEMENT_3D ( 'NONE', #15438, #11991, #30883 ) ;
#22800 = CARTESIAN_POINT ( 'NONE',  ( 20.87224371475484475, -27.19134377947485248, -5.902448757945053970 ) ) ;
#22801 = FACE_OUTER_BOUND ( 'NONE', #12824, .T. ) ;
#22802 = VERTEX_POINT ( 'NONE', #17615 ) ;
#22803 = EDGE_CURVE ( 'NONE', #3779, #32505, #5050, .T. ) ;
#22804 = CARTESIAN_POINT ( 'NONE',  ( 11.77217231312305223, 19.50978363648416547, -21.59411333990740545 ) ) ;
#22805 = ORIENTED_EDGE ( 'NONE', *, *, #14308, .T. ) ;
#22806 = CARTESIAN_POINT ( 'NONE',  ( -14.31861646336927230, 22.24101317123190569, -14.54554263817891702 ) ) ;
#22807 = CARTESIAN_POINT ( 'NONE',  ( -30.79094061804842397, -13.52614530981761831, 19.66345542862528006 ) ) ;
#22808 = ADVANCED_FACE ( 'NONE', ( #8456 ), #27116, .T. ) ;
#22809 = LINE ( 'NONE', #3720, #32835 ) ;
#22810 = CARTESIAN_POINT ( 'NONE',  ( 12.43267688036053187, 20.43562119112951692, -19.50373040854491080 ) ) ;
#22811 = B_SPLINE_CURVE_WITH_KNOTS ( 'NONE', 3,
 ( #2062, #5101, #11200, #29880, #14438, #8751 ),
 .UNSPECIFIED., .F., .F.,
 ( 4, 2, 4 ),
 ( 0.000000000000000000, 0.5000000000000000000, 1.000000000000000000 ),
 .UNSPECIFIED. ) ;
#22812 = ORIENTED_EDGE ( 'NONE', *, *, #5484, .F. ) ;
#22813 = CARTESIAN_POINT ( 'NONE',  ( 22.53426880051877035, -12.42977529295302652, -19.62973737113728490 ) ) ;
#22814 = CARTESIAN_POINT ( 'NONE',  ( -10.80698216227225394, 13.84996144622306247, 13.00000000000000178 ) ) ;
#22815 = ORIENTED_EDGE ( 'NONE', *, *, #6787, .F. ) ;
#22817 = DIRECTION ( 'NONE',  ( 0.4999999999999920064, -0.8660254037844432595, 0.000000000000000000 ) ) ;
#22816 = CARTESIAN_POINT ( 'NONE',  ( -14.69713093287458427, 26.03946747147639584, -10.15458874994915028 ) ) ;
#22818 = CARTESIAN_POINT ( 'NONE',  ( -13.61946501912157714, -23.12974890171631870, -15.38845843242090261 ) ) ;
#22819 = CARTESIAN_POINT ( 'NONE',  ( -13.87104230352202094, 20.53934056656885687, 7.000000000000000000 ) ) ;
#22820 = AXIS2_PLACEMENT_3D ( 'NONE', #25151, #6265, #31253 ) ;
#22821 = ORIENTED_EDGE ( 'NONE', *, *, #29947, .F. ) ;
#22822 = CARTESIAN_POINT ( 'NONE',  ( -29.46499357413496867, -13.19446224756526220, -13.82164065331125968 ) ) ;
#22823 = CARTESIAN_POINT ( 'NONE',  ( -14.23983225781402417, -26.43328798539083735, -5.474040432887671948 ) ) ;
#22824 = CARTESIAN_POINT ( 'NONE',  ( 6.354454053420415249, 35.54304081427981288, 11.00000000000000000 ) ) ;
#22825 = CARTESIAN_POINT ( 'NONE',  ( 16.14888623509959942, 20.94233928415653168, -11.72143342499177088 ) ) ;
#22826 = ORIENTED_EDGE ( 'NONE', *, *, #10476, .T. ) ;
#22827 = CARTESIAN_POINT ( 'NONE',  ( 20.22268228429073034, 4.508760637809952954, -27.05330256971496539 ) ) ;
#22828 = CARTESIAN_POINT ( 'NONE',  ( -3.503793317224519477, 8.420815634768723967, 11.00000000000000000 ) ) ;
#22829 = CYLINDRICAL_SURFACE ( 'NONE', #21251, 1.000000000000000000 ) ;
#22830 = EDGE_LOOP ( 'NONE', ( #12636, #29844, #8813, #21928 ) ) ;
#22831 = CARTESIAN_POINT ( 'NONE',  ( -20.48845606910846939, 0.6931994281368786259, -30.00000000000000000 ) ) ;
#22832 = CARTESIAN_POINT ( 'NONE',  ( 20.54489790006002892, 0.3835546433576813574, -28.69025006841924963 ) ) ;
#22833 = CARTESIAN_POINT ( 'NONE',  ( 19.13253804983751394, -21.21924640916230942, 20.25080042701564764 ) ) ;
#22834 = VERTEX_POINT ( 'NONE', #2367 ) ;
#22835 = CIRCLE ( 'NONE', #33252, 0.4999999999999988898 ) ;
#22836 = CARTESIAN_POINT ( 'NONE',  ( -16.24796006241077961, 15.88921519459651499, -21.50719306941234876 ) ) ;
#22837 = CARTESIAN_POINT ( 'NONE',  ( 10.44103466624280507, 32.57396620494213124, 7.499999999999997335 ) ) ;
#22838 = AXIS2_PLACEMENT_3D ( 'NONE', #15335, #21825, #9048 ) ;
#22839 = DIRECTION ( 'NONE',  ( 0.000000000000000000, 0.000000000000000000, 1.000000000000000000 ) ) ;
#22840 = FACE_OUTER_BOUND ( 'NONE', #37034, .T. ) ;
#22841 = CARTESIAN_POINT ( 'NONE',  ( -11.81630298851966288, 31.79381426990562787, 11.00000000000000000 ) ) ;
#22842 = DIRECTION ( 'NONE',  ( 0.000000000000000000, 0.000000000000000000, 1.000000000000000000 ) ) ;
#22843 = TOROIDAL_SURFACE ( 'NONE', #22202, 1.000000000000000000, 0.5000000000000000000 ) ;
#22844 = CARTESIAN_POINT ( 'NONE',  ( 17.00000000000000000, 22.50000000000000711, 6.000000000000000000 ) ) ;
#22845 = ORIENTED_EDGE ( 'NONE', *, *, #21753, .F. ) ;
#22846 = CARTESIAN_POINT ( 'NONE',  ( 8.118377661053324701, 10.47536095541698486, 7.000000000000000000 ) ) ;
#22847 = DIRECTION ( 'NONE',  ( 0.2079116908177532641, -0.9781476007338069101, 0.000000000000000000 ) ) ;
#22848 = CARTESIAN_POINT ( 'NONE',  ( 19.20779205614405072, -16.68223394817295713, -19.73749630327306903 ) ) ;
#22849 = CARTESIAN_POINT ( 'NONE',  ( -13.03641663870442891, 15.85735326529964873, 13.00000000000000178 ) ) ;
#22850 = FACE_OUTER_BOUND ( 'NONE', #458, .T. ) ;
#22851 = CARTESIAN_POINT ( 'NONE',  ( 10.95309464140887812, 18.88199699059095948, -23.77075622942746591 ) ) ;
#22852 = SURFACE_STYLE_USAGE ( .BOTH. , #26313 ) ;
#22853 = ORIENTED_EDGE ( 'NONE', *, *, #944, .F. ) ;
#22854 = CARTESIAN_POINT ( 'NONE',  ( -17.77135203137562058, 19.64225148421929390, -6.915705780155396276 ) ) ;
#22855 = CARTESIAN_POINT ( 'NONE',  ( -24.08646667827941101, -13.28101593840491290, 20.99999999999999645 ) ) ;
#22856 = VECTOR ( 'NONE', #38178, 1000.000000000000114 ) ;
#22857 = CARTESIAN_POINT ( 'NONE',  ( 14.71950235153890141, -25.64848556417364378, -10.18105174685851999 ) ) ;
#22858 = DIRECTION ( 'NONE',  ( -0.000000000000000000, -0.000000000000000000, -1.000000000000000000 ) ) ;
#22859 = CARTESIAN_POINT ( 'NONE',  ( 15.30169432489863013, 26.49078902709227989, -7.357960067667439930 ) ) ;
#22860 = ORIENTED_EDGE ( 'NONE', *, *, #12857, .T. ) ;
#22861 = CARTESIAN_POINT ( 'NONE',  ( 12.39027692975310124, 20.49132159761027339, -19.49634355596792901 ) ) ;
#22862 = EDGE_LOOP ( 'NONE', ( #13286, #28832, #5786, #914 ) ) ;
#22864 = CARTESIAN_POINT ( 'NONE',  ( 3.503793317224327186, 8.420815634768674229, 7.000000000000000000 ) ) ;
#22863 = CARTESIAN_POINT ( 'NONE',  ( -10.95909218333906487, 17.37826635768778516, -28.70499877695077373 ) ) ;
#22865 = CARTESIAN_POINT ( 'NONE',  ( -12.61201992331770150, -22.55708276399396794, -16.44710463512250342 ) ) ;
#22866 = CARTESIAN_POINT ( 'NONE',  ( -37.13148535761799707, -14.80270701502672459, 11.55979286843934872 ) ) ;
#22867 = AXIS2_PLACEMENT_3D ( 'NONE', #28276, #10594, #6923 ) ;
#22868 = CARTESIAN_POINT ( 'NONE',  ( -30.92005800807112337, -19.98835077949903294, -9.284583649112713388 ) ) ;
#22869 = CARTESIAN_POINT ( 'NONE',  ( -4.809173904559163937, -24.92317228705597287, -5.480779845647450799 ) ) ;
#22870 = CARTESIAN_POINT ( 'NONE',  ( 11.64932880570667351, 17.76966214386914800, -25.05926785085788211 ) ) ;
#22871 = EDGE_LOOP ( 'NONE', ( #34097, #18753 ) ) ;
#22872 = CARTESIAN_POINT ( 'NONE',  ( 23.08742108726735864, 9.144738169211333201, -8.888958855014557514 ) ) ;
#22873 = CARTESIAN_POINT ( 'NONE',  ( -2.166144608099595636, 42.50000000000004974, 11.00000000000000000 ) ) ;
#22874 = CARTESIAN_POINT ( 'NONE',  ( -14.89115357024799380, -26.59122515138228948, -5.000000000000000000 ) ) ;
#22875 = CARTESIAN_POINT ( 'NONE',  ( -8.686999124430418107, 33.93090424204633848, 17.92354375535250810 ) ) ;
#22876 = VERTEX_POINT ( 'NONE', #24092 ) ;
#22877 = CARTESIAN_POINT ( 'NONE',  ( -28.78671411640772959, -1.326716728304855542, -13.36536875498820720 ) ) ;
#22878 = CARTESIAN_POINT ( 'NONE',  ( -14.75813536907479318, 8.520613428071742490, 20.69868183039781329 ) ) ;
#22879 = EDGE_LOOP ( 'NONE', ( #36032, #3191 ) ) ;
#22880 = DIRECTION ( 'NONE',  ( -1.000000000000000000, 0.000000000000000000, 0.000000000000000000 ) ) ;
#22881 = PLANE ( 'NONE',  #3783 ) ;
#22882 = CARTESIAN_POINT ( 'NONE',  ( 34.61427093075294437, -16.43137713082842666, -5.857256890622249301 ) ) ;
#22883 = CIRCLE ( 'NONE', #5377, 1.000000000000000000 ) ;
#22884 = CARTESIAN_POINT ( 'NONE',  ( 35.07402885326985853, -20.24999999999990408, 11.55979286843934872 ) ) ;
#22885 = ADVANCED_FACE ( 'NONE', ( #30984 ), #5992, .F. ) ;
#22886 = CIRCLE ( 'NONE', #27450, 0.4999999999999995559 ) ;
#22887 = ORIENTED_EDGE ( 'NONE', *, *, #9966, .T. ) ;
#22888 = FACE_OUTER_BOUND ( 'NONE', #8208, .T. ) ;
#22889 = CARTESIAN_POINT ( 'NONE',  ( -6.354454053420248272, 35.54304081427989814, 7.000000000000000000 ) ) ;
#22890 = CIRCLE ( 'NONE', #13177, 1.000000000000000000 ) ;
#22891 = DIRECTION ( 'NONE',  ( 0.8090169943749430104, -0.5877852522924791323, 0.000000000000000000 ) ) ;
#22892 = VERTEX_POINT ( 'NONE', #33455 ) ;
#22893 = ADVANCED_FACE ( 'NONE', ( #39726 ), #33846, .T. ) ;
#22894 = CARTESIAN_POINT ( 'NONE',  ( -1.688293718737135851, 33.40510209930049257, -12.89208270232461828 ) ) ;
#22895 = DIRECTION ( 'NONE',  ( 0.000000000000000000, 0.000000000000000000, 1.000000000000000000 ) ) ;
#22896 = CARTESIAN_POINT ( 'NONE',  ( 5.982165713378432059, 28.55918256678898715, 7.000000000000000000 ) ) ;
#22897 = EDGE_CURVE ( 'NONE', #24444, #18426, #34890, .T. ) ;
#22898 = DIRECTION ( 'NONE',  ( 0.000000000000000000, -0.000000000000000000, -1.000000000000000000 ) ) ;
#22899 = CARTESIAN_POINT ( 'NONE',  ( -7.713869163866016621, 10.18146832927085121, 7.500000000000000888 ) ) ;
#22900 = VECTOR ( 'NONE', #26100, 1000.000000000000114 ) ;
#22901 = CARTESIAN_POINT ( 'NONE',  ( -8.100578861132728292, 28.44816123811128605, 10.49999999999999822 ) ) ;
#22902 = CARTESIAN_POINT ( 'NONE',  ( 9.714866619683970583, 18.51369873714040537, -26.70036842142175004 ) ) ;
#22903 = CARTESIAN_POINT ( 'NONE',  ( 30.90412082983250741, -0.04211290444289944590, -5.000000000000000000 ) ) ;
#22904 = VERTEX_POINT ( 'NONE', #2564 ) ;
#22906 = DIRECTION ( 'NONE',  ( 0.8660254037844437036, 0.4999999999999912292, -0.000000000000000000 ) ) ;
#22905 = CARTESIAN_POINT ( 'NONE',  ( -18.33793368410551494, 13.06784656731418437, -17.99966567637481063 ) ) ;
#22907 = VECTOR ( 'NONE', #37097, 999.9999999999998863 ) ;
#22908 = CARTESIAN_POINT ( 'NONE',  ( -0.4999999999999998890, 37.50000000000000711, 10.59344459855561027 ) ) ;
#22909 = CARTESIAN_POINT ( 'NONE',  ( 15.53709981414127483, -26.75515487142352100, -5.000000000000000888 ) ) ;
#22910 = DIRECTION ( 'NONE',  ( 0.4067366430757888840, -0.9135454576426058626, 0.000000000000000000 ) ) ;
#22911 = CARTESIAN_POINT ( 'NONE',  ( 14.51165130258184988, 25.03008843810978235, -11.59459722426760386 ) ) ;
#22912 = AXIS2_PLACEMENT_3D ( 'NONE', #27099, #30150, #36645 ) ;
#22913 = CARTESIAN_POINT ( 'NONE',  ( -1.775381057445013511E-14, 40.84107189184581443, -14.51648065752882566 ) ) ;
#22914 = CARTESIAN_POINT ( 'NONE',  ( -24.08861866610206093, -13.27715813466841865, 23.00000000000000355 ) ) ;
#22915 =( GEOMETRIC_REPRESENTATION_CONTEXT ( 3 ) GLOBAL_UNCERTAINTY_ASSIGNED_CONTEXT ( ( #13639 ) ) GLOBAL_UNIT_ASSIGNED_CONTEXT ( ( #26344, #10918, #39132 ) ) REPRESENTATION_CONTEXT ( 'NONE', 'WORKASPACE' ) );
#22916 = CARTESIAN_POINT ( 'NONE',  ( -23.57342501307383387, -22.18880773095553138, -12.97801393859235297 ) ) ;
#22917 = CARTESIAN_POINT ( 'NONE',  ( 7.182736407388268240, -19.60433374307056908, -26.43616374447599426 ) ) ;
#22918 = CARTESIAN_POINT ( 'NONE',  ( 14.90956390896501915, 25.40097293458214622, -10.18423201954005641 ) ) ;
#22919 = CARTESIAN_POINT ( 'NONE',  ( 18.41239260963195790, 13.48770510890848051, -16.96331977760756970 ) ) ;
#22920 = EDGE_CURVE ( 'NONE', #33392, #27087, #18399, .T. ) ;
#22921 = AXIS2_PLACEMENT_3D ( 'NONE', #23352, #38185, #28839 ) ;
#22922 = DIRECTION ( 'NONE',  ( -1.000000000000000000, 0.000000000000000000, 0.000000000000000000 ) ) ;
#22923 = FACE_OUTER_BOUND ( 'NONE', #3255, .T. ) ;
#22924 = EDGE_CURVE ( 'NONE', #15493, #27371, #34252, .T. ) ;
#22925 = ORIENTED_EDGE ( 'NONE', *, *, #7603, .F. ) ;
#22926 = CARTESIAN_POINT ( 'NONE',  ( -5.279954849186515808, 19.80786611602342973, -29.24590087848358877 ) ) ;
#22927 = VERTEX_POINT ( 'NONE', #24884 ) ;
#22928 = CARTESIAN_POINT ( 'NONE',  ( -11.07691353229041731, -20.48794067953776477, -20.55402119402114991 ) ) ;
#22929 = CIRCLE ( 'NONE', #14525, 1.000000000000000000 ) ;
#22930 = CARTESIAN_POINT ( 'NONE',  ( -14.31603901957233838, 19.98981538725089990, 10.49999999999999822 ) ) ;
#22931 = VERTEX_POINT ( 'NONE', #27732 ) ;
#22932 = CARTESIAN_POINT ( 'NONE',  ( 27.77418311698831488, 0.1426534356837458328, -13.50886777650709902 ) ) ;
#22933 = CARTESIAN_POINT ( 'NONE',  ( 0.000000000000000000, 0.000000000000000000, 7.000000000000000000 ) ) ;
#22934 = DIRECTION ( 'NONE',  ( 0.000000000000000000, 0.000000000000000000, 1.000000000000000000 ) ) ;
#22935 = EDGE_LOOP ( 'NONE', ( #359, #7362, #12024, #17701 ) ) ;
#22936 = CARTESIAN_POINT ( 'NONE',  ( -30.51319350132663288, 0.08894917402604617107, -7.358348470158322385 ) ) ;
#22937 = VERTEX_POINT ( 'NONE', #21634 ) ;
#22938 = CARTESIAN_POINT ( 'NONE',  ( 32.69488556240459332, -8.773221015582116422, -11.16016912004820050 ) ) ;
#22939 = AXIS2_PLACEMENT_3D ( 'NONE', #20013, #23856, #8214 ) ;
#22940 = ORIENTED_EDGE ( 'NONE', *, *, #18338, .F. ) ;
#22941 =( NAMED_UNIT ( * ) SI_UNIT ( $, .STERADIAN. ) SOLID_ANGLE_UNIT ( ) );
#22942 = CARTESIAN_POINT ( 'NONE',  ( 13.80292604922460953, 34.21633694312859575, 11.00000000000012257 ) ) ;
#22943 = DIRECTION ( 'NONE',  ( 0.000000000000000000, 0.000000000000000000, 1.000000000000000000 ) ) ;
#22944 = CARTESIAN_POINT ( 'NONE',  ( 13.84305327410120334, 40.15700533419733631, 10.00000000000000000 ) ) ;
#22945 = EDGE_CURVE ( 'NONE', #15085, #20641, #26447, .T. ) ;
#22946 = CARTESIAN_POINT ( 'NONE',  ( 12.19685572513878036, 28.97783243917147900, 18.42518152272108622 ) ) ;
#22947 = AXIS2_PLACEMENT_3D ( 'NONE', #14166, #23109, #29407 ) ;
#22948 = CARTESIAN_POINT ( 'NONE',  ( -5.440908595777639079, 35.94977745735568675, 9.500000000000000000 ) ) ;
#22949 = ORIENTED_EDGE ( 'NONE', *, *, #11500, .T. ) ;
#22950 = DIRECTION ( 'NONE',  ( 0.000000000000000000, 0.000000000000000000, 1.000000000000000000 ) ) ;
#22951 = DIRECTION ( 'NONE',  ( -0.000000000000000000, -0.000000000000000000, -1.000000000000000000 ) ) ;
#22952 = DIRECTION ( 'NONE',  ( 0.000000000000000000, 0.000000000000000000, 1.000000000000000000 ) ) ;
#22953 = CARTESIAN_POINT ( 'NONE',  ( 15.17029220080370600, 14.77339687257036260, -24.28810107756022063 ) ) ;
#22954 = CARTESIAN_POINT ( 'NONE',  ( 9.102363436486372805, 31.45286188096421043, -12.09631145245175077 ) ) ;
#22955 = AXIS2_PLACEMENT_3D ( 'NONE', #2815, #8317, #36544 ) ;
#22956 = VERTEX_POINT ( 'NONE', #2754 ) ;
#22957 = DIRECTION ( 'NONE',  ( 0.9510565162951544194, 0.3090169943749450643, 0.000000000000000000 ) ) ;
#22958 = CARTESIAN_POINT ( 'NONE',  ( -0.4999999999999998890, 37.50000000000000711, 10.49999999999999822 ) ) ;
#22959 = CARTESIAN_POINT ( 'NONE',  ( 16.10155988989870934, -26.68239398247207461, -7.337369887910988098 ) ) ;
#22960 = FACE_OUTER_BOUND ( 'NONE', #11691, .T. ) ;
#22961 = DIRECTION ( 'NONE',  ( -0.000000000000000000, -0.000000000000000000, -1.000000000000000000 ) ) ;
#22962 = VERTEX_POINT ( 'NONE', #15146 ) ;
#22963 = CARTESIAN_POINT ( 'NONE',  ( -12.66689476310357598, 21.03365424557304664, -18.45460298430356616 ) ) ;
#22964 = AXIS2_PLACEMENT_3D ( 'NONE', #14671, #39446, #3419 ) ;
#22965 = CARTESIAN_POINT ( 'NONE',  ( -27.04902410903751786, -24.92680750149321867, 16.87380292611406318 ) ) ;
#22966 = CARTESIAN_POINT ( 'NONE',  ( 14.88849274807932765, -26.59100623965352739, -5.000000000000000888 ) ) ;
#22967 = CARTESIAN_POINT ( 'NONE',  ( 10.14060191828658120, 25.26915018278934255, 10.50000000000000000 ) ) ;
#22968 = EDGE_CURVE ( 'NONE', #34846, #1082, #24290, .T. ) ;
#22969 = ORIENTED_EDGE ( 'NONE', *, *, #34928, .T. ) ;
#22970 = ORIENTED_EDGE ( 'NONE', *, *, #3771, .T. ) ;
#22971 = CARTESIAN_POINT ( 'NONE',  ( -8.376537992280214340, 19.04457702326376278, -27.24859099131081663 ) ) ;
#22972 = CARTESIAN_POINT ( 'NONE',  ( -16.05099858185807449, -21.51520586029840842, -17.05908743202043709 ) ) ;
#22973 = CARTESIAN_POINT ( 'NONE',  ( 3.503793317224329851, 8.420815634768676006, 9.000000000000001776 ) ) ;
#22974 = CIRCLE ( 'NONE', #9359, 59.99999999999998579 ) ;
#22975 = CARTESIAN_POINT ( 'NONE',  ( -21.19038336318232751, -5.228579731333282687, -24.44094102819527947 ) ) ;
#22976 = CARTESIAN_POINT ( 'NONE',  ( 11.11016527260166420, 31.83082137946473367, 7.000000000000000000 ) ) ;
#22977 = ORIENTED_EDGE ( 'NONE', *, *, #1631, .T. ) ;
#22978 = CARTESIAN_POINT ( 'NONE',  ( 30.39593018562074178, 0.08170413101267633149, -7.828442670039330586 ) ) ;
#22979 = CARTESIAN_POINT ( 'NONE',  ( 12.13489577590003776, 19.91918274404604361, -20.54176213831676634 ) ) ;
#22980 = CARTESIAN_POINT ( 'NONE',  ( -12.80736835487442349, 15.68301270189233954, 7.499999999999993783 ) ) ;
#22981 = ORIENTED_EDGE ( 'NONE', *, *, #7559, .T. ) ;
#22982 = CARTESIAN_POINT ( 'NONE',  ( -26.51672392814666779, 0.2580214034863175243, -15.44851676060052270 ) ) ;
#22983 = CARTESIAN_POINT ( 'NONE',  ( 0.2655024426717602637, 36.24516302788250499, 12.00000000000000000 ) ) ;
#22984 = ORIENTED_EDGE ( 'NONE', *, *, #28544, .T. ) ;
#22985 = CARTESIAN_POINT ( 'NONE',  ( 33.76045296747373925, -4.171667482292196638, -6.352430751017280386 ) ) ;
#22986 = AXIS2_PLACEMENT_3D ( 'NONE', #23703, #36103, #15355 ) ;
#22987 = CARTESIAN_POINT ( 'NONE',  ( 1.872892888448897120, -2.256054360071899634, 7.499999999999997335 ) ) ;
#22988 = CARTESIAN_POINT ( 'NONE',  ( 35.26975574857903695, -18.21959598282672488, 14.53008259254013979 ) ) ;
#22989 = ORIENTED_EDGE ( 'NONE', *, *, #26093, .F. ) ;
#22990 = CARTESIAN_POINT ( 'NONE',  ( 5.259215691052598451, 38.11244126491433803, 15.72805884748939853 ) ) ;
#22991 = CARTESIAN_POINT ( 'NONE',  ( 4.269522338418829820E-14, -20.30912387778604966, 19.66345542862528717 ) ) ;
#22992 = PLANE ( 'NONE',  #31878 ) ;
#22993 = EDGE_CURVE ( 'NONE', #3128, #10038, #21243, .T. ) ;
#22994 = CARTESIAN_POINT ( 'NONE',  ( 4.568463557893653437, 27.32878864566524868, 20.94377226548378346 ) ) ;
#22995 = CARTESIAN_POINT ( 'NONE',  ( 8.927394655428267711, 11.06314620770944757, 11.00000000000000000 ) ) ;
#22996 = ADVANCED_FACE ( 'NONE', ( #33652 ), #36883, .F. ) ;
#22997 = CARTESIAN_POINT ( 'NONE',  ( -8.315274455032252376, 10.01576150750523375, 7.500000000000000888 ) ) ;
#22998 = B_SPLINE_SURFACE_WITH_KNOTS ( 'NONE', 3, 3, ( 
 ( #30800, #33854, #24299, #40129 ),
 ( #5606, #36301, #3163, #12305 ),
 ( #12501, #33661, #8663, #27544 ),
 ( #27149, #18015, #15554, #5411 ),
 ( #17823, #24694, #39929, #2964 ),
 ( #21249, #18211, #15351, #36893 ),
 ( #9258, #30603, #8463, #18608 ),
 ( #8862, #2374, #27740, #14759 ),
 ( #2571, #14956, #27344, #36494 ),
 ( #37091, #30993, #21643, #9063 ),
 ( #21448, #24099, #116, #34046 ),
 ( #20862, #38077, #37877, #10250 ),
 ( #9462, #9665, #34441, #13289 ),
 ( #3555, #34243, #31580, #35040 ),
 ( #25684, #15749, #16349, #6398 ),
 ( #22042, #513, #18804, #709 ),
 ( #10052, #6592, #12696, #19193 ),
 ( #18997, #34836, #15952, #31387 ),
 ( #24893, #28138, #28732, #28332 ),
 ( #31786, #19390, #7193, #315 ),
 ( #12897, #1114, #25289, #3950 ),
 ( #911, #19592, #22634, #13087 ),
 ( #37685, #31982, #37287, #3747 ),
 ( #22231, #9853, #31191, #25477 ),
 ( #3356, #25090, #34635, #37487 ),
 ( #6788, #4148, #16554, #28936 ),
 ( #21840, #16151, #28535, #22431 ),
 ( #6984, #4353, #8210, #23452 ),
 ( #17571, #38892, #29144, #26698 ),
 ( #11068, #16963, #17373, #26084 ),
 ( #13492, #10863, #36048, #19800 ),
 ( #23251, #38484, #4762, #35235 ),
 ( #23041, #20614, #22836, #7393 ),
 ( #29745, #32605, #35842, #32405 ),
 ( #38690, #8003, #20208, #1314 ),
 ( #10659, #1724, #5163, #14100 ),
 ( #33013, #29943, #25884, #35649 ),
 ( #7600, #35445, #13696, #20006 ),
 ( #38283, #20412, #4559, #32808 ),
 ( #10453, #32194, #29343, #7805 ),
 ( #14304, #1514, #13904, #16759 ),
 ( #26295, #17169, #1928, #29545 ),
 ( #26497, #4966, #23652, #39085 ),
 ( #11263, #33806, #23850, #17967 ) ),
 .UNSPECIFIED., .T., .F., .F.,
 ( 4, 1, 1, 1, 2, 1, 1, 1, 1, 1, 1, 1, 2, 1, 1, 1, 2, 1, 1, 1, 1, 1, 1, 1, 2, 1, 1, 1, 2, 1, 1, 1, 1, 1, 1, 1, 4 ),
 ( 4, 4 ),
 ( 0.000000000000000000, 0.03553882639362128393, 0.07107765278724256786, 0.1066164791808638657, 0.1421553055744851357, 0.1660525590443411859, 0.1899498125141971805, 0.2138470659840532306, 0.2377443194539092253, 0.2616415729237652754, 0.2855388263936212701, 0.3094360798634773202, 0.3333333333333333703, 0.3688721597269547514, 0.4044109861205760215, 0.4399498125141973470, 0.4754886389078186171, 0.4993858923776745562, 0.5232831458475305508, 0.5471803993173864900, 0.5710776527872425401, 0.5949749062570985902, 0.6188721597269547514, 0.6427694131968104685, 0.6666666666666665186, 0.7022054930602876777, 0.7377443194539090587, 0.7732831458475302178, 0.8088219722411513768, 0.8327192257110074269, 0.8566164791808634771, 0.8805137326507195272, 0.9044109861205756884, 0.9283082395904318496, 0.9522054930602878997, 0.9761027465301439499, 1.000000000000000000 ),
 ( 0.000000000000000000, 1.000000000000000000 ),
 .UNSPECIFIED. ) ;
#22999 = EDGE_CURVE ( 'NONE', #6543, #38536, #2477, .T. ) ;
#23000 = DIRECTION ( 'NONE',  ( 0.9135454576426059736, 0.4067366430757889395, -0.000000000000000000 ) ) ;
#23001 = CARTESIAN_POINT ( 'NONE',  ( 31.24272016125543416, 0.2902395683448312225, 15.72805884748939498 ) ) ;
#23002 = CARTESIAN_POINT ( 'NONE',  ( -23.58808727774059832, 8.960771098271621327, -5.000000000000000000 ) ) ;
#23003 = CARTESIAN_POINT ( 'NONE',  ( 21.98490994300607682, -27.05380718176246901, -5.895602069099679099 ) ) ;
#23004 = AXIS2_PLACEMENT_3D ( 'NONE', #36396, #8559, #20954 ) ;
#23005 = CARTESIAN_POINT ( 'NONE',  ( -14.57736017774144699, 22.47612012567159567, 7.000000000000000000 ) ) ;
#23006 = ORIENTED_EDGE ( 'NONE', *, *, #11114, .T. ) ;
#23007 = CARTESIAN_POINT ( 'NONE',  ( 10.84452725066743106, 17.39679239189240434, -29.34533630210047406 ) ) ;
#23008 = ORIENTED_EDGE ( 'NONE', *, *, #6746, .F. ) ;
#23009 = AXIS2_PLACEMENT_3D ( 'NONE', #16666, #20725, #32714 ) ;
#23010 = CARTESIAN_POINT ( 'NONE',  ( -11.99665585415270996, 16.62659876986841567, -30.00000000000000000 ) ) ;
#23011 = CARTESIAN_POINT ( 'NONE',  ( -16.80389827882202880, -21.64427909825945662, 19.99202127657103389 ) ) ;
#23012 = CARTESIAN_POINT ( 'NONE',  ( -14.42035624161469798, 26.65972665747689163, 10.59344459855566356 ) ) ;
#23013 = CARTESIAN_POINT ( 'NONE',  ( 11.04912124349541713, 17.32038412190906840, -28.70874619594562915 ) ) ;
#23014 = EDGE_LOOP ( 'NONE', ( #13597, #12899, #877, #20504 ) ) ;
#23015 = CARTESIAN_POINT ( 'NONE',  ( 17.94885553750267349, -9.904091770223047320, -30.00000000000002842 ) ) ;
#23016 = CARTESIAN_POINT ( 'NONE',  ( 1.587660364795204782, 9.681887955242936883, 12.00000000000000000 ) ) ;
#23017 = ORIENTED_EDGE ( 'NONE', *, *, #21784, .T. ) ;
#23019 = CARTESIAN_POINT ( 'NONE',  ( -8.118377661053489902, 10.47536095541709322, 7.000000000000000000 ) ) ;
#23018 = CARTESIAN_POINT ( 'NONE',  ( -10.93774750043060706, 17.74170758838544160, -26.81279356920407864 ) ) ;
#23020 = EDGE_CURVE ( 'NONE', #2159, #18499, #21916, .T. ) ;
#23021 = CARTESIAN_POINT ( 'NONE',  ( -10.04686839703753876, -18.12954247328852020, -27.41699321995579908 ) ) ;
#23022 = CARTESIAN_POINT ( 'NONE',  ( 13.32168723750162975, 15.60515543615789724, 7.485646746502371940 ) ) ;
#23023 = EDGE_CURVE ( 'NONE', #32239, #29026, #18008, .T. ) ;
#23024 = VERTEX_POINT ( 'NONE', #3349 ) ;
#23025 = CARTESIAN_POINT ( 'NONE',  ( -35.02447263591297855, -13.24401549867776318, -7.135927747732872639 ) ) ;
#23026 = CARTESIAN_POINT ( 'NONE',  ( -9.169462346764058580, -18.33493501355543742, -29.35491832476872176 ) ) ;
#23027 = CARTESIAN_POINT ( 'NONE',  ( 10.80697542085375140, 31.15003855377755571, 12.00000000000000000 ) ) ;
#23028 = CARTESIAN_POINT ( 'NONE',  ( 15.06161168841436471, 19.05444440493321423, -16.70087182429124084 ) ) ;
#23029 = ORIENTED_EDGE ( 'NONE', *, *, #16216, .T. ) ;
#23030 = CARTESIAN_POINT ( 'NONE',  ( 27.43674297377669546, 3.779828424379618301, -5.000000000000001776 ) ) ;
#23031 = DIRECTION ( 'NONE',  ( 0.2876062384759567880, 0.6459741880212539478, -0.7071067811865424657 ) ) ;
#23032 = DIRECTION ( 'NONE',  ( 0.000000000000000000, 0.000000000000000000, 1.000000000000000000 ) ) ;
#23033 = ORIENTED_EDGE ( 'NONE', *, *, #37902, .T. ) ;
#23034 = CARTESIAN_POINT ( 'NONE',  ( -24.64392587737382456, 0.2590282008007734893, -18.42865202136458436 ) ) ;
#23035 = AXIS2_PLACEMENT_3D ( 'NONE', #38220, #1444, #25820 ) ;
#23036 = CARTESIAN_POINT ( 'NONE',  ( 21.79677046812914654, 0.2436873253541234352, -23.79487705795048313 ) ) ;
#23037 = CARTESIAN_POINT ( 'NONE',  ( 30.23838254412189386, -12.22961151633820442, 19.99202127657102324 ) ) ;
#23038 = ORIENTED_EDGE ( 'NONE', *, *, #18265, .T. ) ;
#23039 = CARTESIAN_POINT ( 'NONE',  ( -23.05051288410620103, 1.290431267577835772, -20.62872711280308025 ) ) ;
#23040 = AXIS2_PLACEMENT_3D ( 'NONE', #26318, #5383, #17191 ) ;
#23041 = CARTESIAN_POINT ( 'NONE',  ( -19.79815887584811307, 19.84782313723621883, -4.999999999999999112 ) ) ;
#23042 = EDGE_CURVE ( 'NONE', #19485, #15842, #9607, .T. ) ;
#23043 = DIRECTION ( 'NONE',  ( 1.000000000000000000, 0.000000000000000000, 0.000000000000000000 ) ) ;
#23044 = AXIS2_PLACEMENT_3D ( 'NONE', #39594, #30057, #27009 ) ;
#23045 = AXIS2_PLACEMENT_3D ( 'NONE', #14893, #27080, #33588 ) ;
#23046 = DIRECTION ( 'NONE',  ( -0.000000000000000000, -0.000000000000000000, -1.000000000000000000 ) ) ;
#23047 = EDGE_CURVE ( 'NONE', #8550, #1290, #34995, .T. ) ;
#23048 = EDGE_CURVE ( 'NONE', #13187, #14341, #25140, .T. ) ;
#23049 = CARTESIAN_POINT ( 'NONE',  ( -11.58359699910274720, 32.01076754692467574, 10.49999999999999822 ) ) ;
#23050 = CARTESIAN_POINT ( 'NONE',  ( 14.31603901957230462, 19.98981538725069740, 10.50000000000000533 ) ) ;
#23051 = CYLINDRICAL_SURFACE ( 'NONE', #4254, 1.000000000000000888 ) ;
#23052 = ORIENTED_EDGE ( 'NONE', *, *, #29646, .T. ) ;
#23053 = DIRECTION ( 'NONE',  ( 0.000000000000000000, 0.000000000000000000, -1.000000000000000000 ) ) ;
#23054 = CARTESIAN_POINT ( 'NONE',  ( -4.458872323573595864, 26.51478363815348160, 6.000000000000000000 ) ) ;
#23055 = CARTESIAN_POINT ( 'NONE',  ( 25.40476810523085760, -22.14310417253436469, -12.02608197892994468 ) ) ;
#23056 = CARTESIAN_POINT ( 'NONE',  ( -0.6417741116369681809, 11.68927977431952137, 12.00000000000000000 ) ) ;
#23057 = CARTESIAN_POINT ( 'NONE',  ( 16.72075857324119141, 7.444561356925491147, 11.00000000000000000 ) ) ;
#23058 = CARTESIAN_POINT ( 'NONE',  ( 15.10103005678714894, 27.38430384138463225, -6.871694316642929401 ) ) ;
#23059 = CARTESIAN_POINT ( 'NONE',  ( 0.000000000000000000, 22.50000000000000355, 3.000000000000000000 ) ) ;
#23060 = ORIENTED_EDGE ( 'NONE', *, *, #31114, .T. ) ;
#23061 = CARTESIAN_POINT ( 'NONE',  ( -14.44435570328332652, 14.60131355992008473, -28.82039636960078255 ) ) ;
#23062 = CARTESIAN_POINT ( 'NONE',  ( -25.30804003627941867, -11.14301119665289264, 21.00000000000009948 ) ) ;
#23063 = CARTESIAN_POINT ( 'NONE',  ( 15.27748152860279518, -26.61456374246583678, -6.417151305163597996 ) ) ;
#23064 = DIRECTION ( 'NONE',  ( -0.000000000000000000, -0.000000000000000000, -1.000000000000000000 ) ) ;
#23065 = CARTESIAN_POINT ( 'NONE',  ( 15.42339932183901752, 26.75673767418847859, -5.000000000000002665 ) ) ;
#23066 = VERTEX_POINT ( 'NONE', #34826 ) ;
#23067 = CARTESIAN_POINT ( 'NONE',  ( 11.68277618612572866, 18.91466778193324672, -22.73465507004121733 ) ) ;
#23068 = EDGE_LOOP ( 'NONE', ( #19644, #5415 ) ) ;
#23069 = CIRCLE ( 'NONE', #10752, 0.5000000000000004441 ) ;
#23071 = DIRECTION ( 'NONE',  ( 0.000000000000000000, 0.000000000000000000, 1.000000000000000000 ) ) ;
#23070 = CARTESIAN_POINT ( 'NONE',  ( -13.73783782086621308, 23.46750919750577680, -14.46876710495131313 ) ) ;
#23072 = EDGE_CURVE ( 'NONE', #10321, #14195, #14119, .T. ) ;
#23073 = CARTESIAN_POINT ( 'NONE',  ( -12.64202328258549990, -22.55724117488063030, -16.44518350383058447 ) ) ;
#23074 = CARTESIAN_POINT ( 'NONE',  ( -16.88398162953599169, -29.10422986782303667, 12.14047268033038129 ) ) ;
#23075 = EDGE_CURVE ( 'NONE', #12629, #20052, #32313, .T. ) ;
#23076 = VECTOR ( 'NONE', #26958, 999.9999999999998863 ) ;
#23077 = AXIS2_PLACEMENT_3D ( 'NONE', #21337, #2849, #29872 ) ;
#23078 = CARTESIAN_POINT ( 'NONE',  ( -25.88132202143377469, -15.63261420755070930, -15.67704684687844185 ) ) ;
#23079 = CARTESIAN_POINT ( 'NONE',  ( -9.295420884976664411, -25.43675055676933638, -4.999999999999999112 ) ) ;
#23080 = CARTESIAN_POINT ( 'NONE',  ( 11.85474644856143378, 17.60367872427052305, -25.08547864272203398 ) ) ;
#23081 = EDGE_LOOP ( 'NONE', ( #8649, #19508, #19523, #21672, #4603 ) ) ;
#23082 = CARTESIAN_POINT ( 'NONE',  ( 23.30655953786771661, 8.157976315886919849, -10.85338692621293077 ) ) ;
#23083 = CARTESIAN_POINT ( 'NONE',  ( 4.440908595777811385, 35.94977745735560859, 7.000000000000000000 ) ) ;
#23084 = LINE ( 'NONE', #4601, #29656 ) ;
#23085 = ORIENTED_EDGE ( 'NONE', *, *, #39152, .F. ) ;
#23086 = ADVANCED_BREP_SHAPE_REPRESENTATION ( '', ( #9362, #24238 ), #9333 ) ;
#23087 = CARTESIAN_POINT ( 'NONE',  ( -32.18856600309058535, -1.666818702012493381, -6.386702722256275777 ) ) ;
#23088 = CARTESIAN_POINT ( 'NONE',  ( -13.32472804387900567, 14.30980730577158155, 20.25080042701567251 ) ) ;
#23089 = ORIENTED_EDGE ( 'NONE', *, *, #27882, .T. ) ;
#23090 = DIRECTION ( 'NONE',  ( -0.000000000000000000, -0.000000000000000000, -1.000000000000000000 ) ) ;
#23091 = CARTESIAN_POINT ( 'NONE',  ( -14.11133924723978161, 27.61078317377194224, 7.000000000000000000 ) ) ;
#23092 = CARTESIAN_POINT ( 'NONE',  ( 31.34477257452704535, -13.70488752507857910, -11.99102932043097169 ) ) ;
#23093 = CARTESIAN_POINT ( 'NONE',  ( 37.09709568333405372, -7.051483854461498169, 11.55979286843942511 ) ) ;
#23094 = ADVANCED_FACE ( 'NONE', ( #6977 ), #4499, .F. ) ;
#23095 = VERTEX_POINT ( 'NONE', #6583 ) ;
#23096 = DIRECTION ( 'NONE',  ( -0.000000000000000000, -0.000000000000000000, -1.000000000000000000 ) ) ;
#23097 = AXIS2_PLACEMENT_3D ( 'NONE', #21970, #25609, #22165 ) ;
#23098 = CARTESIAN_POINT ( 'NONE',  ( -15.42743469815759028, 26.74224822490523579, -5.000000000000002665 ) ) ;
#23099 = CIRCLE ( 'NONE', #34133, 1.000000000000002665 ) ;
#23100 = AXIS2_PLACEMENT_3D ( 'NONE', #29460, #16475, #10579 ) ;
#23101 = LINE ( 'NONE', #10309, #37612 ) ;
#23102 = ORIENTED_EDGE ( 'NONE', *, *, #7842, .T. ) ;
#23103 = CARTESIAN_POINT ( 'NONE',  ( -0.7219791468970899739, 36.56720658881546626, -9.725050104156155228 ) ) ;
#23104 = CARTESIAN_POINT ( 'NONE',  ( -14.97433423632582006, 21.61937474157331351, 7.485699520496981840 ) ) ;
#23105 = CIRCLE ( 'NONE', #8171, 1.000000000000000888 ) ;
#23106 = CARTESIAN_POINT ( 'NONE',  ( -3.118678732975735279, 7.827785988993307242, 12.00000000000000000 ) ) ;
#23107 = CARTESIAN_POINT ( 'NONE',  ( 19.26948696230199687, 27.85601271560034675, 11.00000000000000000 ) ) ;
#23108 = CARTESIAN_POINT ( 'NONE',  ( 7.293999462566144842, 11.53598992149257008, 6.000000000000000000 ) ) ;
#23109 = DIRECTION ( 'NONE',  ( -0.000000000000000000, -0.000000000000000000, -1.000000000000000000 ) ) ;
#23110 = CARTESIAN_POINT ( 'NONE',  ( 9.501231361094543360, 18.85103192176102738, -26.04902248843100665 ) ) ;
#23111 = CARTESIAN_POINT ( 'NONE',  ( -2.672146553953452575, 12.33340603770394317, 10.00000000000000000 ) ) ;
#23112 = ORIENTED_EDGE ( 'NONE', *, *, #6164, .T. ) ;
#23114 = DIRECTION ( 'NONE',  ( -0.000000000000000000, -0.000000000000000000, -1.000000000000000000 ) ) ;
#23113 = CARTESIAN_POINT ( 'NONE',  ( -17.34395368315986730, 11.20622719433779757, -27.17580777125886726 ) ) ;
#23115 = CARTESIAN_POINT ( 'NONE',  ( -0.4999999999999998890, 37.09261900150649893, 10.99387790580546032 ) ) ;
#23116 = CARTESIAN_POINT ( 'NONE',  ( 9.514046198846664026, -18.15855281542499000, -30.00000000000000000 ) ) ;
#23117 = DIRECTION ( 'NONE',  ( 0.000000000000000000, 0.000000000000000000, 1.000000000000000000 ) ) ;
#23118 = CARTESIAN_POINT ( 'NONE',  ( 11.65547513713623573, 18.94099047327305740, -22.72982294686783789 ) ) ;
#23119 = CARTESIAN_POINT ( 'NONE',  ( -16.84920187454418539, 29.09530251867925443, -5.000000000000000000 ) ) ;
#23120 = PLANE ( 'NONE',  #7703 ) ;
#23121 = CARTESIAN_POINT ( 'NONE',  ( -14.94827155352230186, -14.02787326271796609, -30.00000000000001421 ) ) ;
#23122 = CARTESIAN_POINT ( 'NONE',  ( 7.004305706416510624, -19.31551653162770776, -29.39181977775634991 ) ) ;
#23123 = CARTESIAN_POINT ( 'NONE',  ( 14.41205314296764683, 24.16671282165543388, -12.56218448904276741 ) ) ;
#23124 = CARTESIAN_POINT ( 'NONE',  ( 20.57095190365273396, 13.97674357447790250, -4.999999999999997335 ) ) ;
#23125 = EDGE_CURVE ( 'NONE', #38914, #35744, #37494, .T. ) ;
#23126 = DIRECTION ( 'NONE',  ( 0.000000000000000000, 0.000000000000000000, 1.000000000000000000 ) ) ;
#23127 = CARTESIAN_POINT ( 'NONE',  ( 5.002948306803792100, 36.19539921059735832, 10.49999999999999822 ) ) ;
#23128 = ADVANCED_FACE ( 'NONE', ( #1658 ), #10231, .T. ) ;
#23129 = ORIENTED_EDGE ( 'NONE', *, *, #10877, .T. ) ;
#23130 = CARTESIAN_POINT ( 'NONE',  ( -6.337285794301795505, 36.78338214817075880, -7.138834133703192641 ) ) ;
#23131 = ORIENTED_EDGE ( 'NONE', *, *, #17104, .F. ) ;
#23132 = CARTESIAN_POINT ( 'NONE',  ( -14.47023594716632999, -25.43102382604878642, -10.65652329803860532 ) ) ;
#23133 = AXIS2_PLACEMENT_3D ( 'NONE', #36281, #4992, #7831 ) ;
#23134 = DIRECTION ( 'NONE',  ( 0.000000000000000000, 0.000000000000000000, 1.000000000000000000 ) ) ;
#23135 = VERTEX_POINT ( 'NONE', #506 ) ;
#23136 = CARTESIAN_POINT ( 'NONE',  ( 11.44134295108989363, 15.31698729810773152, 9.500000000000000000 ) ) ;
#23137 = AXIS2_PLACEMENT_3D ( 'NONE', #6769, #15729, #13271 ) ;
#23138 = CARTESIAN_POINT ( 'NONE',  ( 9.156995300982067931, 10.74712803024074503, 10.82238861112330142 ) ) ;
#23139 = EDGE_CURVE ( 'NONE', #31499, #9140, #19988, .T. ) ;
#23140 = ORIENTED_EDGE ( 'NONE', *, *, #36449, .F. ) ;
#23141 = CARTESIAN_POINT ( 'NONE',  ( -20.69120578336301008, 0.8799204947885410633, -27.45047952108874512 ) ) ;
#23142 = ORIENTED_EDGE ( 'NONE', *, *, #38037, .T. ) ;
#23143 = CARTESIAN_POINT ( 'NONE',  ( 33.35964565017460615, -8.962426252800922200, -10.25865101404451352 ) ) ;
#23144 = ORIENTED_EDGE ( 'NONE', *, *, #20232, .T. ) ;
#23145 = CARTESIAN_POINT ( 'NONE',  ( 1.947644445291152104, 40.50000000000006395, 11.55979286843935050 ) ) ;
#23146 = B_SPLINE_CURVE_WITH_KNOTS ( 'NONE', 3,
 ( #10168, #3664, #16059, #28447, #819, #13200, #34951, #31698, #25594, #7105, #22744, #22148, #19109, #35147, #19501, #19707, #4264, #31895, #37602, #37790, #31302, #3469, #37395, #25799, #6900, #4058, #16463, #1024, #25003, #7301, #623, #28049, #32099, #16262, #34354, #13405, #9571, #227, #12612, #21953, #6503, #18909, #15864, #13004, #9768, #25392, #28250, #427, #34750, #12807, #25204, #6700, #34549, #31501, #9964, #22344, #13806, #16874, #7913, #26199, #29850, #26804, #35957, #29253 ),
 .UNSPECIFIED., .F., .F.,
 ( 4, 2, 2, 2, 2, 2, 2, 2, 2, 2, 2, 2, 2, 2, 2, 2, 2, 2, 2, 2, 2, 2, 2, 2, 2, 2, 2, 2, 2, 2, 2, 4 ),
 ( 0.06544620927018722500, 0.06740620535651276057, 0.06838620339967552142, 0.06936620144283828227, 0.07328619361548933953, 0.07524618970181487509, 0.07622618774497763594, 0.07720618578814039679, 0.08112617796079146792, 0.08210617600395422877, 0.08308617404711698962, 0.08504617013344251131, 0.08896616230609356857, 0.08994616034925632941, 0.09092615839241909026, 0.09288615447874459807, 0.09484615056507009201, 0.09582614860823285285, 0.09680614665139561370, 0.1007261388240466016, 0.1026861349103721094, 0.1036661329535348564, 0.1046461309966976172, 0.1085661231693486051, 0.1105261192556741129, 0.1124861153419996207, 0.1164061075146506086, 0.1183661036009761164, 0.1203260996873016242, 0.1222860957736271181, 0.1242460918599526259, 0.1281660840326036277 ),
 .UNSPECIFIED. ) ;
#23147 = CYLINDRICAL_SURFACE ( 'NONE', #24245, 0.5000000000000004441 ) ;
#23148 = FACE_OUTER_BOUND ( 'NONE', #18725, .T. ) ;
#23149 = CARTESIAN_POINT ( 'NONE',  ( 12.83067079990607340, 27.60880874002252128, 18.42518152272263521 ) ) ;
#23150 = CARTESIAN_POINT ( 'NONE',  ( -14.36830325120615548, 20.48707633493503621, 7.000000000000000000 ) ) ;
#23151 = ORIENTED_EDGE ( 'NONE', *, *, #15478, .T. ) ;
#23152 = DIRECTION ( 'NONE',  ( -0.000000000000000000, -0.000000000000000000, 1.000000000000000000 ) ) ;
#23153 = DIRECTION ( 'NONE',  ( -0.000000000000000000, -0.000000000000000000, -1.000000000000000000 ) ) ;
#23154 = EDGE_CURVE ( 'NONE', #21833, #8090, #2447, .T. ) ;
#23155 = FACE_OUTER_BOUND ( 'NONE', #29230, .T. ) ;
#23156 = CARTESIAN_POINT ( 'NONE',  ( 15.66611865990399188, 14.17652996785340314, -24.32473454633646170 ) ) ;
#23157 = TOROIDAL_SURFACE ( 'NONE', #10867, 1.000000000000000000, 0.5000000000000000000 ) ;
#23158 = CARTESIAN_POINT ( 'NONE',  ( 7.918914183234117665, 24.62754220467781607, -18.88895522463596066 ) ) ;
#23159 = VECTOR ( 'NONE', #19985, 1000.000000000000000 ) ;
#23160 = ORIENTED_EDGE ( 'NONE', *, *, #6890, .T. ) ;
#23161 = CARTESIAN_POINT ( 'NONE',  ( -4.817371740575545402, 23.83900317890010001, 20.99999999999999645 ) ) ;
#23162 = CARTESIAN_POINT ( 'NONE',  ( -0.6237384431625470071, 19.56555719779890978, 6.000000000000000000 ) ) ;
#23163 = CARTESIAN_POINT ( 'NONE',  ( 14.62307350666250727, -24.21852764430928318, -13.43612557937942142 ) ) ;
#23164 = CYLINDRICAL_SURFACE ( 'NONE', #8070, 1.000000000000000000 ) ;
#23165 = CARTESIAN_POINT ( 'NONE',  ( -8.633502029282189127, 11.46765470489704342, 7.499999999999999112 ) ) ;
#23166 = ORIENTED_EDGE ( 'NONE', *, *, #21935, .F. ) ;
#23167 = AXIS2_PLACEMENT_3D ( 'NONE', #11124, #17229, #2585 ) ;
#23168 = CARTESIAN_POINT ( 'NONE',  ( -11.02828492200578658, 17.43271654862448372, -28.07671141248061275 ) ) ;
#23169 = CARTESIAN_POINT ( 'NONE',  ( -27.27686897039919955, -25.33890797347529755, 16.30093088680157010 ) ) ;
#23170 = CARTESIAN_POINT ( 'NONE',  ( 14.73837995999511641, -26.18078596994419271, -8.300944784147242572 ) ) ;
#23171 = ADVANCED_FACE ( 'NONE', ( #37675 ), #13837, .T. ) ;
#23172 = PLANE ( 'NONE',  #6876 ) ;
#23173 = EDGE_LOOP ( 'NONE', ( #35821, #4904, #34560, #28029 ) ) ;
#23174 = VERTEX_POINT ( 'NONE', #6779 ) ;
#23175 = CARTESIAN_POINT ( 'NONE',  ( -13.28590053108947799, 29.03689826311631350, -9.996870771847651937 ) ) ;
#23176 = DIRECTION ( 'NONE',  ( 0.6123724356957913617, -0.3535533905932748411, -0.7071067811865496822 ) ) ;
#23177 = ADVANCED_FACE ( 'NONE', ( #19181 ), #4179, .T. ) ;
#23178 = CARTESIAN_POINT ( 'NONE',  ( -12.30736835487442882, 14.81698729810789672, 11.00000000000000000 ) ) ;
#23179 = CARTESIAN_POINT ( 'NONE',  ( -20.12188542190007468, -4.958127744699047490, -27.81140718703422010 ) ) ;
#23180 = CARTESIAN_POINT ( 'NONE',  ( -7.014595103779441843, 35.79644522156330311, 7.000000000000000000 ) ) ;
#23181 = ORIENTED_EDGE ( 'NONE', *, *, #4816, .T. ) ;
#23182 = CARTESIAN_POINT ( 'NONE',  ( 30.64998978746207570, 0.1153925296135153711, -6.417209882492363349 ) ) ;
#23183 = EDGE_CURVE ( 'NONE', #2015, #29633, #8301, .T. ) ;
#23184 = CARTESIAN_POINT ( 'NONE',  ( -10.81260707898136708, 32.90853150812170469, 10.50000000000000533 ) ) ;
#23185 = DIRECTION ( 'NONE',  ( 1.000000000000000000, 0.000000000000000000, 0.000000000000000000 ) ) ;
#23186 = DIRECTION ( 'NONE',  ( 0.4999999999999920064, -0.8660254037844432595, -0.000000000000000000 ) ) ;
#23187 = EDGE_CURVE ( 'NONE', #38979, #6441, #13476, .T. ) ;
#23188 = ORIENTED_EDGE ( 'NONE', *, *, #25127, .T. ) ;
#23189 = CARTESIAN_POINT ( 'NONE',  ( -20.48235837767022716, 0.8503560580662928858, -29.34820720422862550 ) ) ;
#23190 = CARTESIAN_POINT ( 'NONE',  ( 8.410254037844358876, 17.06698729810774395, 10.49999999999999822 ) ) ;
#23191 = ORIENTED_EDGE ( 'NONE', *, *, #33006, .F. ) ;
#23192 = CARTESIAN_POINT ( 'NONE',  ( 30.96795480659843847, -2.880468441431110360, -11.37706435339893041 ) ) ;
#23193 = CONICAL_SURFACE ( 'NONE', #36846, 0.9999999999999986677, 0.7853981633974501664 ) ;
#23194 = AXIS2_PLACEMENT_3D ( 'NONE', #25964, #20091, #10538 ) ;
#23195 = LINE ( 'NONE', #31734, #12257 ) ;
#23196 = CARTESIAN_POINT ( 'NONE',  ( 32.79363849989022839, -0.7437118703939968878, 15.13084544680386578 ) ) ;
#23197 = ORIENTED_EDGE ( 'NONE', *, *, #28481, .T. ) ;
#23198 = CARTESIAN_POINT ( 'NONE',  ( -8.305703523986128545, 36.29191545080267645, 16.30093088680110469 ) ) ;
#23199 = AXIS2_PLACEMENT_3D ( 'NONE', #22837, #22635, #37879 ) ;
#23200 = CARTESIAN_POINT ( 'NONE',  ( -5.409649191045132532, -22.50706359516090060, 18.42518152272108978 ) ) ;
#23201 = CARTESIAN_POINT ( 'NONE',  ( -12.80736835487442349, 15.68301270189233954, 7.000000000000000000 ) ) ;
#23202 = CARTESIAN_POINT ( 'NONE',  ( 5.000428297552684143, 29.07988060316543155, 20.69868183039781329 ) ) ;
#23203 = AXIS2_PLACEMENT_3D ( 'NONE', #24485, #30396, #27338 ) ;
#23204 = DIRECTION ( 'NONE',  ( -0.8153776007405543202, 0.04273212933195244534, 0.5773502691896267303 ) ) ;
#23205 = ORIENTED_EDGE ( 'NONE', *, *, #27931, .T. ) ;
#23206 = ADVANCED_FACE ( 'NONE', ( #20550 ), #32943, .T. ) ;
#23207 = DIRECTION ( 'NONE',  ( 0.2876062384759450197, -0.6459741880212619414, -0.7071067811865398012 ) ) ;
#23208 = ADVANCED_FACE ( 'NONE', ( #26632 ), #33146, .T. ) ;
#23209 = CARTESIAN_POINT ( 'NONE',  ( 3.650831912126976331, 27.51027965810262543, -17.63966039508103023 ) ) ;
#23210 = CARTESIAN_POINT ( 'NONE',  ( -12.80736835487441816, 15.68301270189233243, 11.00000000000000000 ) ) ;
#23211 = CARTESIAN_POINT ( 'NONE',  ( 22.19651343351639738, 6.568638172588949331, 18.42518152272089793 ) ) ;
#23212 = CARTESIAN_POINT ( 'NONE',  ( -22.21927468398150296, 10.75596765700722024, -7.916699199386848740 ) ) ;
#23213 = CARTESIAN_POINT ( 'NONE',  ( 14.40695447559362918, -17.97978767915237341, -22.25716284559454650 ) ) ;
#23214 = LINE ( 'NONE', #26860, #13905 ) ;
#23215 = VECTOR ( 'NONE', #30634, 1000.000000000000227 ) ;
#23216 = CARTESIAN_POINT ( 'NONE',  ( -9.165211421344535481, 24.66068167190384841, 12.00000000000000000 ) ) ;
#23217 = CARTESIAN_POINT ( 'NONE',  ( 2.036571916123607551, 8.108948098542043681, 10.49999999999999822 ) ) ;
#23218 = CARTESIAN_POINT ( 'NONE',  ( 15.25445287089756441, 26.65416740092992498, -7.354337790751865889 ) ) ;
#23219 = CIRCLE ( 'NONE', #25157, 1.000000000000000888 ) ;
#23220 = EDGE_LOOP ( 'NONE', ( #4242, #20548, #29523, #20933 ) ) ;
#23222 = VECTOR ( 'NONE', #29184, 1000.000000000000000 ) ;
#23221 = CARTESIAN_POINT ( 'NONE',  ( -12.79219479534856774, 19.13966889506235347, -20.65395721553354846 ) ) ;
#23223 = CARTESIAN_POINT ( 'NONE',  ( -30.78606151650984657, -16.23943018785164938, 19.27171037444191981 ) ) ;
#23224 = CARTESIAN_POINT ( 'NONE',  ( -14.12406941186437770, 26.56345723075652998, 10.96580508970279766 ) ) ;
#23225 = CARTESIAN_POINT ( 'NONE',  ( 11.03950910960345766, 17.27365618835783678, -29.34954168035285704 ) ) ;
#23226 = EDGE_LOOP ( 'NONE', ( #1339, #18307 ) ) ;
#23227 = CARTESIAN_POINT ( 'NONE',  ( 23.87817301747191934, -12.24222096213839706, -18.61666795014612674 ) ) ;
#23228 = ORIENTED_EDGE ( 'NONE', *, *, #4583, .F. ) ;
#23229 = AXIS2_PLACEMENT_3D ( 'NONE', #24647, #24448, #36841 ) ;
#23231 = DIRECTION ( 'NONE',  ( 1.000000000000000000, 1.734723475976809067E-15, 0.000000000000000000 ) ) ;
#23230 = CARTESIAN_POINT ( 'NONE',  ( -10.93239227196862906, 17.93597283121687269, -26.19762304272490638 ) ) ;
#23232 = CARTESIAN_POINT ( 'NONE',  ( -15.80249673657252529, -25.67169305692603842, -10.58215573314341462 ) ) ;
#23233 = EDGE_CURVE ( 'NONE', #2993, #13835, #18054, .T. ) ;
#23234 = DIRECTION ( 'NONE',  ( -1.000000000000000000, 2.602085213965210642E-15, 0.000000000000000000 ) ) ;
#23235 = CONICAL_SURFACE ( 'NONE', #31041, 1.000000000000002665, 0.7853981633974543852 ) ;
#23236 = ORIENTED_EDGE ( 'NONE', *, *, #32117, .F. ) ;
#23237 = CARTESIAN_POINT ( 'NONE',  ( -18.92370352201584538, -8.520676925239653698, -27.71828468939111545 ) ) ;
#23238 = CARTESIAN_POINT ( 'NONE',  ( -12.50179810955727966, -23.06732317427903922, -15.48378489298444549 ) ) ;
#23239 = CARTESIAN_POINT ( 'NONE',  ( 14.48927117870122494, -30.61587158504688588, 22.99999999999999289 ) ) ;
#23240 = CARTESIAN_POINT ( 'NONE',  ( 17.21933148029187421, 21.00599287609430732, -6.908854110444175411 ) ) ;
#23241 = ORIENTED_EDGE ( 'NONE', *, *, #21797, .T. ) ;
#23242 = CARTESIAN_POINT ( 'NONE',  ( 22.98885138662875960, 3.755270039684655892, -18.76986221281831391 ) ) ;
#23243 = DIRECTION ( 'NONE',  ( -0.000000000000000000, -0.000000000000000000, 1.000000000000000000 ) ) ;
#23244 = CARTESIAN_POINT ( 'NONE',  ( 1.981960960816328887, 14.62372257652092422, 6.000000000000000000 ) ) ;
#23245 = ORIENTED_EDGE ( 'NONE', *, *, #21447, .T. ) ;
#23246 = CARTESIAN_POINT ( 'NONE',  ( -30.99742014632522569, -0.1379718400911539578, -4.999999999999999112 ) ) ;
#23247 = CARTESIAN_POINT ( 'NONE',  ( 26.83762895626454537, -0.2330588716970352914, -15.38901361913504928 ) ) ;
#23248 = CARTESIAN_POINT ( 'NONE',  ( 28.25018339770975118, -2.647087534805041553, 19.27171037444157164 ) ) ;
#23249 = VERTEX_POINT ( 'NONE', #36185 ) ;
#23250 = CARTESIAN_POINT ( 'NONE',  ( -28.19786622711188784, 2.629271227132516486, -7.374041015958935574 ) ) ;
#23251 = CARTESIAN_POINT ( 'NONE',  ( -23.06249103411543544, 13.31513540672989926, -4.999999999999996447 ) ) ;
#23252 = DIRECTION ( 'NONE',  ( -0.4999999999999919509, 0.8660254037844432595, 0.000000000000000000 ) ) ;
#23253 = VECTOR ( 'NONE', #13389, 1000.000000000000000 ) ;
#23254 = CIRCLE ( 'NONE', #40086, 0.5000000000000000000 ) ;
#23255 = CARTESIAN_POINT ( 'NONE',  ( -12.53024597560957609, 27.62278594035707613, 9.500000000000000000 ) ) ;
#23256 = AXIS2_PLACEMENT_3D ( 'NONE', #26700, #23046, #38487 ) ;
#23257 = EDGE_CURVE ( 'NONE', #11482, #11960, #19341, .T. ) ;
#23258 = CARTESIAN_POINT ( 'NONE',  ( -2.231935796429922902, 7.666817632609298272, 7.382773698552460573 ) ) ;
#23259 = LINE ( 'NONE', #23457, #19693 ) ;
#23260 = DIRECTION ( 'NONE',  ( 0.5720614028176864707, -0.4156269377774609031, -0.7071067811865414665 ) ) ;
#23261 = ORIENTED_EDGE ( 'NONE', *, *, #18199, .F. ) ;
#23262 = CARTESIAN_POINT ( 'NONE',  ( -22.33022999260465724, 5.911010040927092035, -17.87267886299877162 ) ) ;
#23263 = DIRECTION ( 'NONE',  ( -1.000000000000000000, 0.000000000000000000, 0.000000000000000000 ) ) ;
#23264 = CARTESIAN_POINT ( 'NONE',  ( -5.184280209938394002, 31.68549066217158483, 10.50000000000000355 ) ) ;
#23265 = CARTESIAN_POINT ( 'NONE',  ( 20.87822957844602456, -19.29698014627262737, -16.74541713236688167 ) ) ;
#23266 = CARTESIAN_POINT ( 'NONE',  ( -0.2655091840902661926, 8.754836972118123839, 12.00000000000000000 ) ) ;
#23267 = CARTESIAN_POINT ( 'NONE',  ( -14.83795255154715598, 20.43771420437966313, 10.68306085400112870 ) ) ;
#23268 = CARTESIAN_POINT ( 'NONE',  ( 14.16267402188527313, 24.80506001027335472, -12.52237342293435240 ) ) ;
#23269 = ORIENTED_EDGE ( 'NONE', *, *, #32917, .F. ) ;
#23270 = CARTESIAN_POINT ( 'NONE',  ( -17.22179567822546176, 20.49768920708832454, -8.352296547685462258 ) ) ;
#23271 = CARTESIAN_POINT ( 'NONE',  ( -24.81299795227001326, -13.60183200321525732, 21.00000000000004619 ) ) ;
#23272 = CARTESIAN_POINT ( 'NONE',  ( 11.85325580602118301, -21.48896600845587557, -18.45743837482206828 ) ) ;
#23273 = DIRECTION ( 'NONE',  ( 0.9945218953682742891, 0.1045284632676437425, 0.000000000000000000 ) ) ;
#23274 = CARTESIAN_POINT ( 'NONE',  ( 14.85248842483373188, 25.57170511055247175, -10.18105171841187584 ) ) ;
#23275 = ORIENTED_EDGE ( 'NONE', *, *, #32459, .T. ) ;
#23276 = CARTESIAN_POINT ( 'NONE',  ( 12.12763111783735503, 19.92791405175542607, -20.54027923519833010 ) ) ;
#23277 = ORIENTED_EDGE ( 'NONE', *, *, #34625, .F. ) ;
#23279 = CARTESIAN_POINT ( 'NONE',  ( 3.558056881628218981, 8.165525635826492490, 10.94611345180490503 ) ) ;
#23278 = CARTESIAN_POINT ( 'NONE',  ( -10.99314221940617564, 17.45576443972036529, -28.07461421731269979 ) ) ;
#23280 = CARTESIAN_POINT ( 'NONE',  ( -14.86193584663134892, -25.83070395712688949, -9.709670777925021312 ) ) ;
#23281 = EDGE_CURVE ( 'NONE', #37730, #25929, #22811, .T. ) ;
#23282 = CARTESIAN_POINT ( 'NONE',  ( -24.63751168576463968, -28.54157386114988881, 12.14047268033103322 ) ) ;
#23283 = TOROIDAL_SURFACE ( 'NONE', #9659, 1.000000000000000000, 0.5000000000000000000 ) ;
#23284 = CIRCLE ( 'NONE', #21967, 0.5000000000000001110 ) ;
#23285 = CARTESIAN_POINT ( 'NONE',  ( -26.84768961812649835, -16.21779228968876652, -14.72956622491983758 ) ) ;
#23286 = CARTESIAN_POINT ( 'NONE',  ( -5.926965089342771442, -22.63169345552070055, -16.85668200393126526 ) ) ;
#23287 = CARTESIAN_POINT ( 'NONE',  ( 11.69146759026597238, 16.83997637742415776, -29.36300835845053570 ) ) ;
#23289 = EDGE_CURVE ( 'NONE', #22335, #18302, #26833, .T. ) ;
#23288 = EDGE_LOOP ( 'NONE', ( #29638, #28580 ) ) ;
#23290 = CARTESIAN_POINT ( 'NONE',  ( 23.35054822394877760, 9.216580574185069707, -6.449451739544402429 ) ) ;
#23291 = CARTESIAN_POINT ( 'NONE',  ( 2.166144608099552116, 42.50000000000005684, 11.00000000000000178 ) ) ;
#23292 = DIRECTION ( 'NONE',  ( 0.07391278520358141035, -0.7032331762534025366, -0.7071067811865476838 ) ) ;
#23293 = LINE ( 'NONE', #14143, #7617 ) ;
#23294 = ORIENTED_EDGE ( 'NONE', *, *, #27520, .F. ) ;
#23295 = CARTESIAN_POINT ( 'NONE',  ( -27.79641046810536054, -1.962788507153767847, -15.20952948633108193 ) ) ;
#23296 = EDGE_CURVE ( 'NONE', #10818, #17668, #11403, .T. ) ;
#23297 = CARTESIAN_POINT ( 'NONE',  ( -11.93114467671392553, 6.888449590841186243, 20.99999999999999645 ) ) ;
#23298 = EDGE_LOOP ( 'NONE', ( #33595, #21376, #17954, #29119 ) ) ;
#23299 = CARTESIAN_POINT ( 'NONE',  ( 25.20894334605389986, -14.55439022683022543, 20.94377226548378346 ) ) ;
#23300 = DIRECTION ( 'NONE',  ( 0.000000000000000000, 0.000000000000000000, 1.000000000000000000 ) ) ;
#23301 = FACE_OUTER_BOUND ( 'NONE', #35939, .T. ) ;
#23302 = CARTESIAN_POINT ( 'NONE',  ( 34.10630787157268884, -17.48172648250967143, -6.276852260651874182 ) ) ;
#23303 = CARTESIAN_POINT ( 'NONE',  ( 36.68766582957253064, -16.69324967293806239, 12.14047268033083249 ) ) ;
#23304 = ORIENTED_EDGE ( 'NONE', *, *, #16325, .F. ) ;
#23305 = DIRECTION ( 'NONE',  ( -0.000000000000000000, -0.000000000000000000, -1.000000000000000000 ) ) ;
#23306 = FACE_OUTER_BOUND ( 'NONE', #12351, .T. ) ;
#23307 = EDGE_CURVE ( 'NONE', #30940, #29040, #30291, .T. ) ;
#23308 = EDGE_CURVE ( 'NONE', #22563, #11320, #27037, .T. ) ;
#23309 = CIRCLE ( 'NONE', #36942, 1.000000000000000000 ) ;
#23310 = AXIS2_PLACEMENT_3D ( 'NONE', #15363, #21068, #27755 ) ;
#23311 = FACE_OUTER_BOUND ( 'NONE', #35470, .T. ) ;
#23312 = ORIENTED_EDGE ( 'NONE', *, *, #19398, .F. ) ;
#23313 = CARTESIAN_POINT ( 'NONE',  ( 1.051372576265723557, 25.72197380671092048, -19.63089720651151282 ) ) ;
#23314 = CARTESIAN_POINT ( 'NONE',  ( -13.86495741630578316, 28.22533134718097259, 7.202682876670049694 ) ) ;
#23315 = DIRECTION ( 'NONE',  ( 0.7032331762534032027, 0.07391278520355958059, 0.7071067811865493491 ) ) ;
#23316 = CIRCLE ( 'NONE', #5803, 1.000000000000000000 ) ;
#23317 = DIRECTION ( 'NONE',  ( -1.000000000000000000, 0.000000000000000000, 0.000000000000000000 ) ) ;
#23318 = CARTESIAN_POINT ( 'NONE',  ( -5.458872323573595864, 26.51478363815348160, 12.00000000000000000 ) ) ;
#23319 = DIRECTION ( 'NONE',  ( 0.000000000000000000, 0.000000000000000000, 1.000000000000000000 ) ) ;
#23320 = CARTESIAN_POINT ( 'NONE',  ( 12.11678078314277762, 23.99614306916164708, -16.23412490227547522 ) ) ;
#23321 = CARTESIAN_POINT ( 'NONE',  ( -8.927394655428429360, 11.06314620770957013, 7.000000000000000000 ) ) ;
#23322 = ORIENTED_EDGE ( 'NONE', *, *, #24930, .F. ) ;
#23324 = DIRECTION ( 'NONE',  ( 0.5778781230734078012, 0.000000000000000000, -0.8161230758121934548 ) ) ;
#23323 = CARTESIAN_POINT ( 'NONE',  ( -20.20456973212974106, 14.66708349146731827, -5.482234822857553702 ) ) ;
#23325 = FACE_OUTER_BOUND ( 'NONE', #15337, .T. ) ;
#23326 = CARTESIAN_POINT ( 'NONE',  ( 13.74681413364860383, -24.12214955346338741, -13.51035512735945154 ) ) ;
#23327 = DIRECTION ( 'NONE',  ( 1.000000000000000000, 0.000000000000000000, 0.000000000000000000 ) ) ;
#23328 = CARTESIAN_POINT ( 'NONE',  ( 15.27289138331547669, 26.59085539454768821, -7.356080397504305424 ) ) ;
#23329 = CARTESIAN_POINT ( 'NONE',  ( -19.54664213359414404, -11.28525909758381651, -19.69475445967427163 ) ) ;
#23330 = DIRECTION ( 'NONE',  ( 0.000000000000000000, 0.000000000000000000, 1.000000000000000000 ) ) ;
#23331 = ADVANCED_FACE ( 'NONE', ( #11995 ), #23235, .T. ) ;
#23332 = CARTESIAN_POINT ( 'NONE',  ( -22.15736500781834906, -20.84727699870213868, -14.83950653091789817 ) ) ;
#23333 = CARTESIAN_POINT ( 'NONE',  ( 4.192399910511806382, -20.06660217949758618, -29.41646740880849364 ) ) ;
#23334 = CARTESIAN_POINT ( 'NONE',  ( 11.85241674728229988, 18.75149653998677124, -22.76202379300414691 ) ) ;
#23335 = EDGE_CURVE ( 'NONE', #29633, #35208, #21344, .T. ) ;
#23336 = CARTESIAN_POINT ( 'NONE',  ( 17.07516244282002660, 12.28144768211119953, -24.39718017846627518 ) ) ;
#23337 = FACE_OUTER_BOUND ( 'NONE', #21342, .T. ) ;
#23338 = ORIENTED_EDGE ( 'NONE', *, *, #15074, .T. ) ;
#23339 = CARTESIAN_POINT ( 'NONE',  ( -7.410464713192979502, 36.46669482336120183, -6.720204936114559935 ) ) ;
#23340 = ORIENTED_EDGE ( 'NONE', *, *, #20389, .T. ) ;
#23341 = AXIS2_PLACEMENT_3D ( 'NONE', #23663, #12067, #33428 ) ;
#23342 = DIRECTION ( 'NONE',  ( 0.000000000000000000, 0.000000000000000000, 1.000000000000000000 ) ) ;
#23343 = VERTEX_POINT ( 'NONE', #17907 ) ;
#23344 = CARTESIAN_POINT ( 'NONE',  ( -19.48557158514998022, -11.24999999999982414, 23.00000000000000000 ) ) ;
#23345 = CARTESIAN_POINT ( 'NONE',  ( 9.221287281574511496, 10.65863771052197428, 10.49999999999999822 ) ) ;
#23346 = AXIS2_PLACEMENT_3D ( 'NONE', #8516, #33316, #2426 ) ;
#23347 = ORIENTED_EDGE ( 'NONE', *, *, #5416, .T. ) ;
#23348 = CARTESIAN_POINT ( 'NONE',  ( -22.70365180105937242, 0.7008854888786294479, -21.62861051218136055 ) ) ;
#23349 = ORIENTED_EDGE ( 'NONE', *, *, #32271, .T. ) ;
#23350 = CARTESIAN_POINT ( 'NONE',  ( 35.11092860954450856, -11.76153023245262297, -7.147189329740518460 ) ) ;
#23351 = EDGE_LOOP ( 'NONE', ( #1698, #23629, #5029, #3300 ) ) ;
#23352 = CARTESIAN_POINT ( 'NONE',  ( 0.000000000000000000, 0.000000000000000000, 0.000000000000000000 ) ) ;
#23353 = CARTESIAN_POINT ( 'NONE',  ( 10.47671942996444905, 33.23510584127189560, 7.339470489435492517 ) ) ;
#23354 = VERTEX_POINT ( 'NONE', #2460 ) ;
#23355 = B_SPLINE_CURVE_WITH_KNOTS ( 'NONE', 3,
 ( #14772, #39144, #33072, #15165, #11123, #39546 ),
 .UNSPECIFIED., .F., .F.,
 ( 4, 2, 4 ),
 ( 0.000000000000000000, 0.5000000000000000000, 1.000000000000000000 ),
 .UNSPECIFIED. ) ;
#23356 = FACE_OUTER_BOUND ( 'NONE', #38022, .T. ) ;
#23357 = FACE_OUTER_BOUND ( 'NONE', #11447, .T. ) ;
#23358 = CARTESIAN_POINT ( 'NONE',  ( 6.055828121132759811, 35.60995051739030259, 17.92354375535250099 ) ) ;
#23359 = DIRECTION ( 'NONE',  ( 0.000000000000000000, 0.000000000000000000, 1.000000000000000000 ) ) ;
#23360 = ORIENTED_EDGE ( 'NONE', *, *, #1303, .F. ) ;
#23361 = LINE ( 'NONE', #7714, #19768 ) ;
#23362 = CARTESIAN_POINT ( 'NONE',  ( 5.440829913680675034, 10.60893893836775348, 6.000000000000000000 ) ) ;
#23363 = EDGE_CURVE ( 'NONE', #1365, #2652, #18711, .T. ) ;
#23364 = CARTESIAN_POINT ( 'NONE',  ( -17.34253826607186966, 27.32041144404028188, 11.00000000000000000 ) ) ;
#23365 = CARTESIAN_POINT ( 'NONE',  ( 18.42725648993722842, 16.20988549689709757, -11.84062711183378092 ) ) ;
#23367 = AXIS2_PLACEMENT_3D ( 'NONE', #4678, #8334, #23570 ) ;
#23366 = CARTESIAN_POINT ( 'NONE',  ( 6.331554793186663588, 19.58397683058095140, -28.53572403070387864 ) ) ;
#23368 = EDGE_LOOP ( 'NONE', ( #15862, #23751 ) ) ;
#23369 = CARTESIAN_POINT ( 'NONE',  ( 1.229431105722923023, 20.49260818092372460, 12.00000000000000000 ) ) ;
#23370 = LINE ( 'NONE', #14421, #16879 ) ;
#23371 = CARTESIAN_POINT ( 'NONE',  ( 15.36935833352434777, -25.93966974496969513, -9.682725942216546144 ) ) ;
#23372 = CARTESIAN_POINT ( 'NONE',  ( 37.19292564617598629, -15.51005328467150512, -4.999999999999994671 ) ) ;
#23373 = CIRCLE ( 'NONE', #14296, 1.000000000000000000 ) ;
#23374 = CARTESIAN_POINT ( 'NONE',  ( -6.762317648414995830, 29.93445088906605633, 10.49999999999999822 ) ) ;
#23375 = VERTEX_POINT ( 'NONE', #21141 ) ;
#23376 = CARTESIAN_POINT ( 'NONE',  ( -11.68537700245894762, 18.91218677661948888, -22.73505939135654330 ) ) ;
#23377 = CARTESIAN_POINT ( 'NONE',  ( -31.36686156446269536, -22.11446460981446549, 16.30093088680186852 ) ) ;
#23378 = CARTESIAN_POINT ( 'NONE',  ( 11.39961882692148087, -22.05299179249424313, -17.51387407834204168 ) ) ;
#23379 = CARTESIAN_POINT ( 'NONE',  ( -9.645751987030186214, 11.01237070952370622, 7.281642668398248475 ) ) ;
#23380 = EDGE_LOOP ( 'NONE', ( #32029, #27939, #36794, #27487, #6071 ) ) ;
#23381 = ORIENTED_EDGE ( 'NONE', *, *, #867, .F. ) ;
#23382 = CARTESIAN_POINT ( 'NONE',  ( -7.682719301950634794, 20.99212371924112119, -23.35384790439877278 ) ) ;
#23383 = DIRECTION ( 'NONE',  ( 1.000000000000000000, 0.000000000000000000, 0.000000000000000000 ) ) ;
#23384 = FACE_BOUND ( 'NONE', #15011, .T. ) ;
#23385 = AXIS2_PLACEMENT_3D ( 'NONE', #37245, #14915, #72 ) ;
#23386 = CARTESIAN_POINT ( 'NONE',  ( -32.20191614452445350, -5.996939808026042762, -11.23890058235647160 ) ) ;
#23387 = CYLINDRICAL_SURFACE ( 'NONE', #2064, 1.000000000000000888 ) ;
#23388 = ORIENTED_EDGE ( 'NONE', *, *, #8815, .F. ) ;
#23389 = CARTESIAN_POINT ( 'NONE',  ( 20.80995787673824893, 0.8960491595669888287, -26.83562114098080187 ) ) ;
#23390 = DIRECTION ( 'NONE',  ( -1.000000000000000000, 0.000000000000000000, 0.000000000000000000 ) ) ;
#23391 = DIRECTION ( 'NONE',  ( 0.5906904945688822295, 0.000000000000000000, -0.8068982213550660587 ) ) ;
#23392 = CARTESIAN_POINT ( 'NONE',  ( -29.42868960315909632, -26.31588593299390411, 11.00000000000013856 ) ) ;
#23393 = VERTEX_POINT ( 'NONE', #33548 ) ;
#23394 = CARTESIAN_POINT ( 'NONE',  ( -30.63049699552009031, -0.03312779925433120137, -7.357393045505457252 ) ) ;
#23395 = CARTESIAN_POINT ( 'NONE',  ( -14.11133924723978161, 27.61078317377194224, 10.49999999999999822 ) ) ;
#23396 = VERTEX_POINT ( 'NONE', #18105 ) ;
#23397 = CARTESIAN_POINT ( 'NONE',  ( 26.43890877042912990, -2.343727469559957033, -17.12617500785380997 ) ) ;
#23398 = CARTESIAN_POINT ( 'NONE',  ( 27.69088631811219159, -26.08775134479562396, 15.13084544680181054 ) ) ;
#23399 = ORIENTED_EDGE ( 'NONE', *, *, #21959, .F. ) ;
#23400 = CARTESIAN_POINT ( 'NONE',  ( 5.476246462222536415, 38.75671607062970025, 14.53008259254011136 ) ) ;
#23401 = VECTOR ( 'NONE', #7915, 1000.000000000000000 ) ;
#23402 = CARTESIAN_POINT ( 'NONE',  ( 5.356921161177231383, -23.13411080437162326, 17.92354375535250810 ) ) ;
#23403 = DIRECTION ( 'NONE',  ( 1.000000000000000000, 0.000000000000000000, 0.000000000000000000 ) ) ;
#23404 = CARTESIAN_POINT ( 'NONE',  ( -7.722840163547155967, 25.57530741997960888, 20.69868183039764276 ) ) ;
#23405 = DIRECTION ( 'NONE',  ( -1.000000000000000000, 0.000000000000000000, 0.000000000000000000 ) ) ;
#23406 = ORIENTED_EDGE ( 'NONE', *, *, #25998, .F. ) ;
#23407 = ADVANCED_FACE ( 'NONE', ( #36780 ), #8951, .F. ) ;
#23408 = CARTESIAN_POINT ( 'NONE',  ( 3.458865582155095986, 18.48521636184714012, 13.00000000000000178 ) ) ;
#23409 = CARTESIAN_POINT ( 'NONE',  ( 4.110008236141186266, 30.79763600885550190, -14.76321218211128716 ) ) ;
#23410 = AXIS2_PLACEMENT_3D ( 'NONE', #31502, #25595, #3665 ) ;
#23411 = CARTESIAN_POINT ( 'NONE',  ( -3.585575659063838572, 32.39727978755421134, 10.75000000000000888 ) ) ;
#23412 = EDGE_CURVE ( 'NONE', #4988, #39486, #34286, .T. ) ;
#23413 = CARTESIAN_POINT ( 'NONE',  ( 12.60925743022028378, 20.19802119776807103, 19.66345542862461215 ) ) ;
#23414 = CIRCLE ( 'NONE', #33810, 0.5000000000000004441 ) ;
#23415 = EDGE_CURVE ( 'NONE', #39789, #19274, #33628, .T. ) ;
#23416 = CARTESIAN_POINT ( 'NONE',  ( 19.84635048062218488, -25.97363186618970943, -9.943601658171525415 ) ) ;
#23417 = CARTESIAN_POINT ( 'NONE',  ( 12.30736835487432579, 14.81698729810772619, 7.000000000000000000 ) ) ;
#23418 = CARTESIAN_POINT ( 'NONE',  ( -13.09742388243079070, 16.09289933416735963, 10.49999999999999822 ) ) ;
#23419 = DIRECTION ( 'NONE',  ( 0.000000000000000000, 0.000000000000000000, 1.000000000000000000 ) ) ;
#23420 = CARTESIAN_POINT ( 'NONE',  ( 11.22254838620092343, 18.10604511926858962, -25.00253263116462321 ) ) ;
#23421 = ORIENTED_EDGE ( 'NONE', *, *, #30913, .F. ) ;
#23422 = CARTESIAN_POINT ( 'NONE',  ( -11.31188296672360671, 17.14851204919853345, -28.71951328966818906 ) ) ;
#23423 = CARTESIAN_POINT ( 'NONE',  ( -31.08318648610590884, -11.03630075675877364, 19.66345542862590889 ) ) ;
#23424 = DIRECTION ( 'NONE',  ( 1.000000000000000000, 0.000000000000000000, 0.000000000000000000 ) ) ;
#23425 = CARTESIAN_POINT ( 'NONE',  ( 12.17448594789072303, 19.87244906308695036, -20.54873440190374012 ) ) ;
#23426 = ORIENTED_EDGE ( 'NONE', *, *, #27135, .T. ) ;
#23427 = CARTESIAN_POINT ( 'NONE',  ( 17.33150493693412031, -10.96591108411289639, -29.21252997676894481 ) ) ;
#23428 = VECTOR ( 'NONE', #29206, 1000.000000000000000 ) ;
#23429 = ORIENTED_EDGE ( 'NONE', *, *, #10603, .T. ) ;
#23431 = LINE ( 'NONE', #36234, #3037 ) ;
#23430 = CARTESIAN_POINT ( 'NONE',  ( -10.72859233046692395, 17.88194238571141170, -26.79320594746885931 ) ) ;
#23432 = CARTESIAN_POINT ( 'NONE',  ( -11.02901866483229121, -18.34862447518570505, -24.88864236400666030 ) ) ;
#23433 = DIRECTION ( 'NONE',  ( 1.000000000000000000, 0.000000000000000000, 0.000000000000000000 ) ) ;
#23434 = ORIENTED_EDGE ( 'NONE', *, *, #35046, .F. ) ;
#23435 = CARTESIAN_POINT ( 'NONE',  ( -27.44899772917025871, -12.30322565212499342, -15.69884287347142404 ) ) ;
#23436 = CARTESIAN_POINT ( 'NONE',  ( -10.23778664914769720, -19.66181284788236994, -22.77101389171386003 ) ) ;
#23437 = CARTESIAN_POINT ( 'NONE',  ( -7.611215932167762155, 18.68301270189229513, 9.000000000000001776 ) ) ;
#23438 = CARTESIAN_POINT ( 'NONE',  ( 15.53819178773900589, 18.26476869418323190, -16.75515271693409147 ) ) ;
#23439 = EDGE_LOOP ( 'NONE', ( #30945, #24627, #29007, #22375 ) ) ;
#23440 = CARTESIAN_POINT ( 'NONE',  ( 28.94531653062197307, 1.996249385887188810, -5.947783999245325859 ) ) ;
#23441 = EDGE_CURVE ( 'NONE', #32004, #25935, #9554, .T. ) ;
#23442 = DIRECTION ( 'NONE',  ( 0.000000000000000000, 0.000000000000000000, 1.000000000000000000 ) ) ;
#23443 = EDGE_CURVE ( 'NONE', #257, #4300, #22132, .T. ) ;
#23444 = EDGE_LOOP ( 'NONE', ( #14145, #27083, #13669 ) ) ;
#23445 = CARTESIAN_POINT ( 'NONE',  ( -21.75755899457715259, 0.4677864005904093236, -23.82221529625467227 ) ) ;
#23446 = CARTESIAN_POINT ( 'NONE',  ( 20.49706908807578287, 0.3883427504116045981, -29.33974050869597150 ) ) ;
#23447 = CIRCLE ( 'NONE', #33808, 0.5000000000000004441 ) ;
#23448 = CARTESIAN_POINT ( 'NONE',  ( 25.46386631785966159, -22.05997124774561513, 19.27171037444122348 ) ) ;
#23449 = CIRCLE ( 'NONE', #5920, 1.000000000000000000 ) ;
#23450 = ORIENTED_EDGE ( 'NONE', *, *, #4405, .T. ) ;
#23451 = CARTESIAN_POINT ( 'NONE',  ( -20.74887948658896164, 1.506378959947736629, -26.88035768992763508 ) ) ;
#23452 = CARTESIAN_POINT ( 'NONE',  ( -22.45323650136969462, -2.382502413133420038, -30.00000000000000000 ) ) ;
#23453 = CARTESIAN_POINT ( 'NONE',  ( -5.440836655099179353, 34.39106106163288246, 13.00000000000000178 ) ) ;
#23454 = DIRECTION ( 'NONE',  ( 0.000000000000000000, 0.000000000000000000, 1.000000000000000000 ) ) ;
#23455 = EDGE_CURVE ( 'NONE', #3736, #6333, #3753, .T. ) ;
#23456 = FACE_OUTER_BOUND ( 'NONE', #11928, .T. ) ;
#23457 = CARTESIAN_POINT ( 'NONE',  ( 7.111215932167702647, 17.81698729810774751, 9.000000000000001776 ) ) ;
#23458 = DIRECTION ( 'NONE',  ( 1.000000000000000000, 0.000000000000000000, 0.000000000000000000 ) ) ;
#23459 = ORIENTED_EDGE ( 'NONE', *, *, #27420, .F. ) ;
#23460 = CARTESIAN_POINT ( 'NONE',  ( -24.28833252230154827, 5.197361523840480224, -13.76725034441404460 ) ) ;
#23461 = DIRECTION ( 'NONE',  ( 0.000000000000000000, 0.000000000000000000, 1.000000000000000000 ) ) ;
#23462 = CARTESIAN_POINT ( 'NONE',  ( -13.26585111513660031, 17.86474508437623143, 13.00000000000000178 ) ) ;
#23463 = CARTESIAN_POINT ( 'NONE',  ( 20.76506965807099192, -18.05532636877229180, -17.69242679302543664 ) ) ;
#23464 = DIRECTION ( 'NONE',  ( 0.000000000000000000, 0.000000000000000000, 1.000000000000000000 ) ) ;
#23465 = CARTESIAN_POINT ( 'NONE',  ( -6.354454053420248272, 35.54304081427989814, 7.000000000000000000 ) ) ;
#23466 = CARTESIAN_POINT ( 'NONE',  ( 12.72381738783331251, 21.98735769358159686, -17.39217821953997145 ) ) ;
#23467 = ORIENTED_EDGE ( 'NONE', *, *, #2616, .T. ) ;
#23468 = AXIS2_PLACEMENT_3D ( 'NONE', #5072, #21315, #12166 ) ;
#23469 = CARTESIAN_POINT ( 'NONE',  ( -16.79589040972348002, 21.53745278782425032, -8.341412201671980498 ) ) ;
#23470 = DIRECTION ( 'NONE',  ( 1.000000000000000000, 0.000000000000000000, 0.000000000000000000 ) ) ;
#23471 = CARTESIAN_POINT ( 'NONE',  ( 10.76785045493358339, -20.00693649655310580, -21.62580521813471535 ) ) ;
#23472 = DIRECTION ( 'NONE',  ( 1.000000000000000000, 0.000000000000000000, 0.000000000000000000 ) ) ;
#23473 = CARTESIAN_POINT ( 'NONE',  ( 12.93818047135676785, 21.63701063370047706, -17.43940108704190450 ) ) ;
#23474 = ORIENTED_EDGE ( 'NONE', *, *, #38334, .T. ) ;
#23475 = FACE_OUTER_BOUND ( 'NONE', #8470, .T. ) ;
#23476 = ORIENTED_EDGE ( 'NONE', *, *, #23308, .T. ) ;
#23478 = CARTESIAN_POINT ( 'NONE',  ( -0.5000000000000005551, 31.00000000000000355, 9.000000000000001776 ) ) ;
#23477 = CARTESIAN_POINT ( 'NONE',  ( -10.94041201910780359, 17.33660477453622306, -29.34740466869044440 ) ) ;
#23479 = CARTESIAN_POINT ( 'NONE',  ( -15.48655661866953892, -26.71642918275651368, -5.945876010756700580 ) ) ;
#23480 = CARTESIAN_POINT ( 'NONE',  ( -34.04990527597851013, -21.89993885138022378, 12.14047268033099591 ) ) ;
#23481 = CARTESIAN_POINT ( 'NONE',  ( -32.15735702992046896, -20.77263526992292242, -6.277248360418026252 ) ) ;
#23482 = CARTESIAN_POINT ( 'NONE',  ( -6.821084136371410089, -20.84928387019777318, -22.02595131697182751 ) ) ;
#23483 = CARTESIAN_POINT ( 'NONE',  ( 15.86158329389953536, 24.87666108630855177, -6.892499796494895747 ) ) ;
#23484 = ORIENTED_EDGE ( 'NONE', *, *, #8409, .T. ) ;
#23485 = CARTESIAN_POINT ( 'NONE',  ( 22.72982457100355802, 9.046144286754186581, -10.86715459307012033 ) ) ;
#23486 = CARTESIAN_POINT ( 'NONE',  ( 15.00099999999999945, 33.00000000000000000, 10.00000000000000000 ) ) ;
#23487 = VECTOR ( 'NONE', #23588, 1000.000000000000000 ) ;
#23488 = CARTESIAN_POINT ( 'NONE',  ( -15.41367234785094809, -26.72342555440733136, -4.999999999999999112 ) ) ;
#23489 = EDGE_CURVE ( 'NONE', #18534, #490, #28142, .T. ) ;
#23490 = DIRECTION ( 'NONE',  ( 0.000000000000000000, 0.000000000000000000, 1.000000000000000000 ) ) ;
#23491 = ORIENTED_EDGE ( 'NONE', *, *, #20581, .T. ) ;
#23492 = CARTESIAN_POINT ( 'NONE',  ( -20.89685344739347173, -1.175242339315835105, -26.67474265850594506 ) ) ;
#23493 = CARTESIAN_POINT ( 'NONE',  ( -15.00309677617818771, 1.567672476163658013, 20.99999999999999645 ) ) ;
#23494 = CARTESIAN_POINT ( 'NONE',  ( 24.70330546561584129, -7.131334670375485629, 20.94377226548427018 ) ) ;
#23495 = DIRECTION ( 'NONE',  ( -0.8090169943749504489, -0.5877852522924690293, 0.000000000000000000 ) ) ;
#23496 = FILL_AREA_STYLE_COLOUR ( '', #17757 ) ;
#23497 = CARTESIAN_POINT ( 'NONE',  ( 29.24088705168217572, -13.85790213908317980, -13.81488898234178642 ) ) ;
#23498 = CARTESIAN_POINT ( 'NONE',  ( 37.34232268491259532, -8.983628415038339199, 11.00000000000000000 ) ) ;
#23499 = AXIS2_PLACEMENT_3D ( 'NONE', #26458, #4526, #14270 ) ;
#23500 = ORIENTED_EDGE ( 'NONE', *, *, #28583, .T. ) ;
#23501 = CARTESIAN_POINT ( 'NONE',  ( -2.421689871081829537, 8.701977744317861863, 7.499999999999997335 ) ) ;
#23502 = ADVANCED_FACE ( 'NONE', ( #37774 ), #15242, .F. ) ;
#23503 = CARTESIAN_POINT ( 'NONE',  ( 6.492361549287938516, 35.85278612139531162, 10.87262190629436986 ) ) ;
#23504 = DIRECTION ( 'NONE',  ( -0.000000000000000000, -0.000000000000000000, -1.000000000000000000 ) ) ;
#23505 = EDGE_CURVE ( 'NONE', #5646, #7027, #33500, .T. ) ;
#23506 = CARTESIAN_POINT ( 'NONE',  ( 1.510082208727901110, 36.50975218198507832, -9.726556050585005053 ) ) ;
#23507 = CARTESIAN_POINT ( 'NONE',  ( 5.348106467989403257, 35.16482219193073178, 13.00000000000000178 ) ) ;
#23508 = CARTESIAN_POINT ( 'NONE',  ( 5.578133564216165574, 24.05045924978295702, 20.99999999999999645 ) ) ;
#23509 = CIRCLE ( 'NONE', #26082, 1.000000000000000888 ) ;
#23510 = EDGE_CURVE ( 'NONE', #7967, #27371, #24588, .T. ) ;
#23511 = CARTESIAN_POINT ( 'NONE',  ( 14.50767453556300701, 21.81310552875920550, 10.66666666666667140 ) ) ;
#23512 = CARTESIAN_POINT ( 'NONE',  ( 3.863783140547853712E-14, -86.77689918168233874, 23.00000000000000000 ) ) ;
#23513 = CARTESIAN_POINT ( 'NONE',  ( -19.26948696230207858, 27.85601271560029701, 11.00000000000000000 ) ) ;
#23514 = CARTESIAN_POINT ( 'NONE',  ( 10.91375165427755789, 19.61687978590818204, -22.60510580339686015 ) ) ;
#23515 = CARTESIAN_POINT ( 'NONE',  ( 21.98892638600344895, 13.77082694162504417, 10.00000000000000000 ) ) ;
#23516 = ORIENTED_EDGE ( 'NONE', *, *, #20452, .T. ) ;
#23517 = EDGE_CURVE ( 'NONE', #10557, #17915, #26478, .T. ) ;
#23518 = AXIS2_PLACEMENT_3D ( 'NONE', #35322, #7275, #16643 ) ;
#23520 = DIRECTION ( 'NONE',  ( 1.000000000000000000, 0.000000000000000000, 0.000000000000000000 ) ) ;
#23519 = CARTESIAN_POINT ( 'NONE',  ( -19.51546397819036827, 15.47399000601905250, -8.398378205727166090 ) ) ;
#23521 = DIRECTION ( 'NONE',  ( 1.000000000000000000, 0.000000000000000000, 0.000000000000000000 ) ) ;
#23522 = CARTESIAN_POINT ( 'NONE',  ( 15.40300567925599395, -26.59730094924787380, -6.887548287194356966 ) ) ;
#23523 = DIRECTION ( 'NONE',  ( 0.000000000000000000, 0.000000000000000000, 1.000000000000000000 ) ) ;
#23524 = CARTESIAN_POINT ( 'NONE',  ( 15.28201387016975232, 26.55918798812530923, -7.356955115318605465 ) ) ;
#23525 = DIRECTION ( 'NONE',  ( -0.6691306063588569053, 0.7431448254773954654, 0.000000000000000000 ) ) ;
#23526 = DIRECTION ( 'NONE',  ( 0.000000000000000000, 0.000000000000000000, 1.000000000000000000 ) ) ;
#23527 = CARTESIAN_POINT ( 'NONE',  ( -15.37464264532748004, -13.57371270378507866, -29.23195595578610195 ) ) ;
#23528 = AXIS2_PLACEMENT_3D ( 'NONE', #38250, #10017, #28301 ) ;
#23529 = CARTESIAN_POINT ( 'NONE',  ( 2.755021161861860080, -20.38581168850896930, -28.85590101152765286 ) ) ;
#23530 = CARTESIAN_POINT ( 'NONE',  ( 12.08865418433290806, 19.17331245234230508, -21.65079422309015911 ) ) ;
#23531 = CARTESIAN_POINT ( 'NONE',  ( 20.38739101816897659, 13.83500035239263859, -8.405622461330182205 ) ) ;
#23532 = CARTESIAN_POINT ( 'NONE',  ( -3.485571585149855434, -11.25000000000002132, 0.000000000000000000 ) ) ;
#23534 = ORIENTED_EDGE ( 'NONE', *, *, #14923, .T. ) ;
#23533 = EDGE_CURVE ( 'NONE', #24240, #15902, #36983, .T. ) ;
#23535 = CARTESIAN_POINT ( 'NONE',  ( -6.207178120114770437, 35.88840053175069755, -8.874516004040346573 ) ) ;
#23536 = ADVANCED_FACE ( 'NONE', ( #12392 ), #9, .F. ) ;
#23537 = VERTEX_POINT ( 'NONE', #3253 ) ;
#23538 = EDGE_CURVE ( 'NONE', #34288, #14430, #1979, .T. ) ;
#23539 = AXIS2_PLACEMENT_3D ( 'NONE', #12268, #18569, #30954 ) ;
#23540 = CARTESIAN_POINT ( 'NONE',  ( 23.05386822411318803, -7.747535282638377652, 20.99999999999999645 ) ) ;
#23541 = ORIENTED_EDGE ( 'NONE', *, *, #21166, .T. ) ;
#23542 = FACE_OUTER_BOUND ( 'NONE', #9398, .T. ) ;
#23543 = AXIS2_PLACEMENT_3D ( 'NONE', #9153, #27840, #8756 ) ;
#23544 = DIRECTION ( 'NONE',  ( 1.000000000000000000, 0.000000000000000000, 0.000000000000000000 ) ) ;
#23545 = EDGE_LOOP ( 'NONE', ( #24061, #6451, #14798, #34008 ) ) ;
#23546 = CARTESIAN_POINT ( 'NONE',  ( -30.47170454527866923, 0.4016671284418431020, -5.474069987333029630 ) ) ;
#23547 = VERTEX_POINT ( 'NONE', #3845 ) ;
#23548 = CARTESIAN_POINT ( 'NONE',  ( 33.42056292424250330, -10.04652305323077144, -10.23864384795611926 ) ) ;
#23549 = AXIS2_PLACEMENT_3D ( 'NONE', #4341, #6971, #28520 ) ;
#23550 = ORIENTED_EDGE ( 'NONE', *, *, #23187, .F. ) ;
#23551 = CARTESIAN_POINT ( 'NONE',  ( -6.953812613386785912, 14.77701242934787906, 6.000000000000000000 ) ) ;
#23552 = VERTEX_POINT ( 'NONE', #38376 ) ;
#23553 = DIRECTION ( 'NONE',  ( 0.9510565162951544194, 0.3090169943749449533, -0.000000000000000000 ) ) ;
#23554 = CARTESIAN_POINT ( 'NONE',  ( -7.354454053420251824, 35.54304081427989814, 7.000000000000000000 ) ) ;
#23555 = EDGE_CURVE ( 'NONE', #1674, #959, #29432, .T. ) ;
#23556 = CIRCLE ( 'NONE', #33940, 0.4999999999999995559 ) ;
#23557 = CARTESIAN_POINT ( 'NONE',  ( -9.490716042090618032, 32.53254263376179267, 18.42518152272187137 ) ) ;
#23558 = EDGE_CURVE ( 'NONE', #29828, #19377, #36859, .T. ) ;
#23559 = LINE ( 'NONE', #27204, #6452 ) ;
#23560 = ORIENTED_EDGE ( 'NONE', *, *, #13823, .F. ) ;
#23561 = ADVANCED_FACE ( 'NONE', ( #16246 ), #10149, .F. ) ;
#23562 = LINE ( 'NONE', #7507, #13908 ) ;
#23563 = DIRECTION ( 'NONE',  ( 1.000000000000000000, 0.000000000000000000, 0.000000000000000000 ) ) ;
#23564 = CARTESIAN_POINT ( 'NONE',  ( 0.5459530983554482519, 27.49993477425252664, 23.00000000000000355 ) ) ;
#23565 = CARTESIAN_POINT ( 'NONE',  ( 14.79081071437772010, 14.21365739191439737, -29.41171982604052815 ) ) ;
#23566 = CIRCLE ( 'NONE', #857, 16.99999999999999645 ) ;
#23567 = CARTESIAN_POINT ( 'NONE',  ( 13.12592325053682174, 31.71798720882053502, -4.999999999999997335 ) ) ;
#23568 = ORIENTED_EDGE ( 'NONE', *, *, #31640, .T. ) ;
#23569 = DIRECTION ( 'NONE',  ( 0.000000000000000000, 0.000000000000000000, -1.000000000000000000 ) ) ;
#23570 = DIRECTION ( 'NONE',  ( 1.000000000000000000, 0.000000000000000000, 0.000000000000000000 ) ) ;
#23571 = AXIS2_PLACEMENT_3D ( 'NONE', #28709, #7576, #887 ) ;
#23572 = CARTESIAN_POINT ( 'NONE',  ( 12.28942040934312985, -21.45707787718824733, -18.40523778129498567 ) ) ;
#23573 = DIRECTION ( 'NONE',  ( 0.000000000000000000, 0.000000000000000000, 1.000000000000000000 ) ) ;
#23574 = DIRECTION ( 'NONE',  ( 0.2079116908177535972, -0.9781476007338069101, 1.734723475976807292E-15 ) ) ;
#23575 = CARTESIAN_POINT ( 'NONE',  ( -15.17240177202555529, 26.28854900485869450, -8.297591635734974602 ) ) ;
#23576 = AXIS2_PLACEMENT_3D ( 'NONE', #616, #18902, #22534 ) ;
#23577 = CARTESIAN_POINT ( 'NONE',  ( -27.98024382195074367, -26.61114576561620026, 13.92931973827786685 ) ) ;
#23578 = CARTESIAN_POINT ( 'NONE',  ( 8.917746432365776244, -18.50716487789387088, -28.72979828505872746 ) ) ;
#23579 = DIRECTION ( 'NONE',  ( 0.1045284632676422437, -0.9945218953682746221, 0.000000000000000000 ) ) ;
#23580 = EDGE_LOOP ( 'NONE', ( #30933, #38657, #39638, #40008 ) ) ;
#23581 = ORIENTED_EDGE ( 'NONE', *, *, #7637, .F. ) ;
#23582 = CARTESIAN_POINT ( 'NONE',  ( -8.544825274508923485, 21.36057392928206511, -22.27686155045734751 ) ) ;
#23583 = DIRECTION ( 'NONE',  ( -0.3090169943749573322, -0.9510565162951504226, 0.000000000000000000 ) ) ;
#23584 = AXIS2_PLACEMENT_3D ( 'NONE', #30166, #17589, #11281 ) ;
#23585 = CYLINDRICAL_SURFACE ( 'NONE', #38621, 1.000000000000000888 ) ;
#23586 = EDGE_CURVE ( 'NONE', #20973, #2015, #12209, .T. ) ;
#23587 = CARTESIAN_POINT ( 'NONE',  ( -22.05567186454189255, -3.361187274895892418, -23.39584885048158114 ) ) ;
#23588 = DIRECTION ( 'NONE',  ( 0.9135454576426059736, 0.4067366430757887730, 0.000000000000000000 ) ) ;
#23589 = EDGE_LOOP ( 'NONE', ( #2116, #27883, #15300, #37639 ) ) ;
#23590 = CARTESIAN_POINT ( 'NONE',  ( 28.29240262143307660, 0.1985313112800510538, -12.55298984254547534 ) ) ;
#23591 = DIRECTION ( 'NONE',  ( 0.5720614028176860266, 0.4156269377774551299, -0.7071067811865451302 ) ) ;
#23592 = CARTESIAN_POINT ( 'NONE',  ( -14.81329996725647469, 19.93755115561707569, 11.00000000000000000 ) ) ;
#23593 = CARTESIAN_POINT ( 'NONE',  ( -2.629601561899601592, 7.723830143584057062, 10.49999999999999822 ) ) ;
#23594 = ORIENTED_EDGE ( 'NONE', *, *, #30569, .F. ) ;
#23595 = CARTESIAN_POINT ( 'NONE',  ( -28.87100298341330529, 0.1244608980665242309, -11.59986624588286652 ) ) ;
#23596 = CARTESIAN_POINT ( 'NONE',  ( -5.478580155932212925, 36.03438916679318282, 10.99387789255783154 ) ) ;
#23597 = ORIENTED_EDGE ( 'NONE', *, *, #35310, .T. ) ;
#23598 = CARTESIAN_POINT ( 'NONE',  ( 34.31080765618935402, -5.232520982112594865, -5.000000000000004441 ) ) ;
#23599 = CIRCLE ( 'NONE', #25523, 1.000000000000000888 ) ;
#23600 = CARTESIAN_POINT ( 'NONE',  ( 35.60445263620119505, -7.407141432647699197, 15.72805884748942518 ) ) ;
#23601 = EDGE_LOOP ( 'NONE', ( #20152, #32135, #38606 ) ) ;
#23602 = CARTESIAN_POINT ( 'NONE',  ( -7.235364705666516905, 38.16413851588594497, 14.53008259254001544 ) ) ;
#23603 = CARTESIAN_POINT ( 'NONE',  ( -11.06125417660426535, -21.75993793948570953, 19.27171037444298207 ) ) ;
#23604 = DIRECTION ( 'NONE',  ( -0.000000000000000000, -0.000000000000000000, 1.000000000000000000 ) ) ;
#23605 = CARTESIAN_POINT ( 'NONE',  ( -3.486159013132843043, 30.04627872069379535, 20.69868183039781684 ) ) ;
#23606 = VECTOR ( 'NONE', #21499, 1000.000000000000000 ) ;
#23607 = DIRECTION ( 'NONE',  ( 1.000000000000000000, 0.000000000000000000, 0.000000000000000000 ) ) ;
#23608 = VERTEX_POINT ( 'NONE', #35130 ) ;
#23609 = EDGE_CURVE ( 'NONE', #35485, #2390, #28629, .T. ) ;
#23610 = CARTESIAN_POINT ( 'NONE',  ( -5.578133564216452456, 24.05045924978193739, 20.99999999999999289 ) ) ;
#23611 = CARTESIAN_POINT ( 'NONE',  ( -8.072173610822130030, 9.857023699286527219, 7.382773698552463237 ) ) ;
#23612 = CARTESIAN_POINT ( 'NONE',  ( 5.775113167322606600, 35.08353508384845298, -10.20345263113499890 ) ) ;
#23613 = FACE_OUTER_BOUND ( 'NONE', #7956, .T. ) ;
#23614 = CIRCLE ( 'NONE', #22294, 1.000000000000000888 ) ;
#23615 = CARTESIAN_POINT ( 'NONE',  ( 18.74997338759060383, -3.362744936764435089, 21.00000000000000000 ) ) ;
#23616 = CARTESIAN_POINT ( 'NONE',  ( 19.79884881832018806, -27.24719281008185590, -5.000000000000007994 ) ) ;
#23617 = FACE_OUTER_BOUND ( 'NONE', #35019, .T. ) ;
#23618 = FACE_OUTER_BOUND ( 'NONE', #22528, .T. ) ;
#23619 = CARTESIAN_POINT ( 'NONE',  ( 4.458865582155095986, 18.48521636184714012, 13.00000000000000178 ) ) ;
#23620 = ORIENTED_EDGE ( 'NONE', *, *, #10314, .F. ) ;
#23621 = CARTESIAN_POINT ( 'NONE',  ( 11.81796877063049855, 19.46134122272024669, -21.60282401223847515 ) ) ;
#23622 = ORIENTED_EDGE ( 'NONE', *, *, #27897, .T. ) ;
#23623 = CARTESIAN_POINT ( 'NONE',  ( -14.50388987035031896, 23.93725455160438997, -12.57114492812263329 ) ) ;
#23624 = CARTESIAN_POINT ( 'NONE',  ( -25.46386631785724219, -22.05997124774662055, 19.27171037444124124 ) ) ;
#23625 = CARTESIAN_POINT ( 'NONE',  ( -8.410254037844435260, 17.06698729810786475, 10.50000000000000355 ) ) ;
#23626 = CARTESIAN_POINT ( 'NONE',  ( 15.28593968016526539, 26.22478663915245889, -7.828761890089739772 ) ) ;
#23627 = ORIENTED_EDGE ( 'NONE', *, *, #35344, .T. ) ;
#23628 = CARTESIAN_POINT ( 'NONE',  ( 32.51966212229606867, -20.60195123665384287, -5.435513030541969215 ) ) ;
#23629 = ORIENTED_EDGE ( 'NONE', *, *, #24764, .T. ) ;
#23631 = CARTESIAN_POINT ( 'NONE',  ( -0.8712085880691411433, 13.69667159339610762, 12.00000000000000000 ) ) ;
#23630 = CARTESIAN_POINT ( 'NONE',  ( -11.17525274941712965, 18.69957113221303757, -23.80519623910948823 ) ) ;
#23632 = CARTESIAN_POINT ( 'NONE',  ( -10.57413422691279159, -17.73442412422751246, -28.02013674793951026 ) ) ;
#23633 = CARTESIAN_POINT ( 'NONE',  ( -5.400683141673551901, 15.91724817395922997, 9.000000000000001776 ) ) ;
#23634 = AXIS2_PLACEMENT_3D ( 'NONE', #30203, #1984, #30000 ) ;
#23635 = VERTEX_POINT ( 'NONE', #13587 ) ;
#23636 = CARTESIAN_POINT ( 'NONE',  ( -35.49576857290053766, -12.23958519446773785, -5.439352978075872258 ) ) ;
#23637 = CARTESIAN_POINT ( 'NONE',  ( -12.84450433006265690, -23.57826165373034399, -14.50520116907959434 ) ) ;
#23638 = ORIENTED_EDGE ( 'NONE', *, *, #35182, .F. ) ;
#23639 = CARTESIAN_POINT ( 'NONE',  ( 20.36878409817081703, 2.417852450439661460, -29.99999999999999289 ) ) ;
#23640 = ADVANCED_FACE ( 'NONE', ( #19684 ), #798, .T. ) ;
#23641 = CARTESIAN_POINT ( 'NONE',  ( -8.118377661053488126, 10.47536095541708967, 10.99999999999999289 ) ) ;
#23642 = FACE_OUTER_BOUND ( 'NONE', #10892, .T. ) ;
#23643 = ORIENTED_EDGE ( 'NONE', *, *, #22185, .T. ) ;
#23644 = CARTESIAN_POINT ( 'NONE',  ( -23.38024468256067578, 0.3787364488140903540, -20.51809825364033202 ) ) ;
#23645 = CARTESIAN_POINT ( 'NONE',  ( 21.35776115567573896, 0.1272554325118729346, -24.94344375846707607 ) ) ;
#23646 = VECTOR ( 'NONE', #14165, 1000.000000000000000 ) ;
#23647 = EDGE_CURVE ( 'NONE', #10152, #4297, #25780, .T. ) ;
#23648 = CARTESIAN_POINT ( 'NONE',  ( 16.23042486173695309, -23.86708630543283149, 18.87996532025784546 ) ) ;
#23649 = EDGE_LOOP ( 'NONE', ( #1000, #609 ) ) ;
#23650 = CARTESIAN_POINT ( 'NONE',  ( -22.28349864444602701, 2.069094159404865518, -21.78945192521086938 ) ) ;
#23651 = EDGE_CURVE ( 'NONE', #31096, #29068, #7283, .T. ) ;
#23652 = CARTESIAN_POINT ( 'NONE',  ( 11.10756861982301125, 19.59949212537556562, -20.90349153980999475 ) ) ;
#23653 = CONICAL_SURFACE ( 'NONE', #11331, 1.000000000000005995, 0.7853981633974496113 ) ;
#23654 = CARTESIAN_POINT ( 'NONE',  ( 14.84160187385922036, 20.32586711126977619, 7.500000000000010658 ) ) ;
#23655 = CARTESIAN_POINT ( 'NONE',  ( -33.14621996124576953, 0.5287779871183843072, 10.99999999999978506 ) ) ;
#23656 = DIRECTION ( 'NONE',  ( 0.000000000000000000, 0.000000000000000000, 1.000000000000000000 ) ) ;
#23657 = DIRECTION ( 'NONE',  ( 0.000000000000000000, 0.000000000000000000, 1.000000000000000000 ) ) ;
#23658 = DIRECTION ( 'NONE',  ( 0.1045284632676437703, -0.9945218953682745111, -0.000000000000000000 ) ) ;
#23659 = EDGE_LOOP ( 'NONE', ( #37980, #11203 ) ) ;
#23660 = CARTESIAN_POINT ( 'NONE',  ( -26.20904522235016287, 5.310845850833655568, -5.000000000000001776 ) ) ;
#23661 = DIRECTION ( 'NONE',  ( 1.000000000000000000, 0.000000000000000000, 0.000000000000000000 ) ) ;
#23662 = ADVANCED_FACE ( 'NONE', ( #4451 ), #7685, .T. ) ;
#23663 = CARTESIAN_POINT ( 'NONE',  ( 14.47283171447379502, 21.48159823030311344, 9.000000000000001776 ) ) ;
#23664 = CARTESIAN_POINT ( 'NONE',  ( 26.21722217325281079, -25.61866019997112076, -6.304309572116824967 ) ) ;
#23665 = DIRECTION ( 'NONE',  ( 0.3535533905932642940, 0.6123724356958055726, -0.7071067811865426878 ) ) ;
#23666 = CARTESIAN_POINT ( 'NONE',  ( -14.75678334372862466, 20.44624543189450705, 10.82238861112329609 ) ) ;
#23667 = CARTESIAN_POINT ( 'NONE',  ( 14.90256438169874365, 26.33380216902334325, -9.220340838230743685 ) ) ;
#23668 = CARTESIAN_POINT ( 'NONE',  ( -5.473344025737330476, 14.11593743010433855, 10.50000000000000000 ) ) ;
#23669 = VERTEX_POINT ( 'NONE', #25975 ) ;
#23670 = CARTESIAN_POINT ( 'NONE',  ( -16.99205359343081057, 21.87216257061389157, -5.000000000000000888 ) ) ;
#23671 = CARTESIAN_POINT ( 'NONE',  ( 16.87498849720590144, -29.16588574430808123, 10.99999999999838174 ) ) ;
#23672 = CARTESIAN_POINT ( 'NONE',  ( -11.33320880805449526, 31.58310643763908487, 10.66666666666665897 ) ) ;
#23673 = CARTESIAN_POINT ( 'NONE',  ( 10.99973294177321215, 17.29901363094238675, -29.34868498375898227 ) ) ;
#23674 = ORIENTED_EDGE ( 'NONE', *, *, #20452, .F. ) ;
#23675 = DIRECTION ( 'NONE',  ( 0.000000000000000000, 0.000000000000000000, -1.000000000000000000 ) ) ;
#23676 = ORIENTED_EDGE ( 'NONE', *, *, #29294, .T. ) ;
#23678 = DIRECTION ( 'NONE',  ( 0.000000000000000000, 0.000000000000000000, 1.000000000000000000 ) ) ;
#23677 = CARTESIAN_POINT ( 'NONE',  ( -10.95797138140908089, 17.47870688081035340, -28.07251611394456603 ) ) ;
#23679 = CARTESIAN_POINT ( 'NONE',  ( -15.50788136758524871, -26.74767648567673817, -5.000000000000000888 ) ) ;
#23680 = CARTESIAN_POINT ( 'NONE',  ( -26.45121176803932173, -27.84758587393086060, 11.00000000000000000 ) ) ;
#23681 = AXIS2_PLACEMENT_3D ( 'NONE', #3188, #39956, #37117 ) ;
#23682 = CARTESIAN_POINT ( 'NONE',  ( -32.89506354292129231, -17.22296157212681322, -8.845019317189917629 ) ) ;
#23683 = CARTESIAN_POINT ( 'NONE',  ( -9.128838725168229473, -25.12525415319764477, -8.353599142830312019 ) ) ;
#23684 = CARTESIAN_POINT ( 'NONE',  ( 11.87583182831933293, 17.23919556405288844, -26.29577713834995834 ) ) ;
#23685 = ORIENTED_EDGE ( 'NONE', *, *, #2172, .T. ) ;
#23686 = CARTESIAN_POINT ( 'NONE',  ( 23.88329450473187165, 7.269808345019653117, -10.83961925935574122 ) ) ;
#23687 = CARTESIAN_POINT ( 'NONE',  ( 3.587660364795204782, 9.681887955242936883, 12.00000000000000000 ) ) ;
#23688 = CYLINDRICAL_SURFACE ( 'NONE', #30304, 1.000000000000000888 ) ;
#23689 = PLANE ( 'NONE',  #17392 ) ;
#23690 = CIRCLE ( 'NONE', #17208, 15.00000000000000000 ) ;
#23691 = VERTEX_POINT ( 'NONE', #4038 ) ;
#23692 = CARTESIAN_POINT ( 'NONE',  ( -31.99486564968922409, -1.644587291267736617, -7.306215044918229040 ) ) ;
#23693 = ADVANCED_FACE ( 'NONE', ( #1608 ), #26381, .T. ) ;
#23694 = CARTESIAN_POINT ( 'NONE',  ( 20.69502533546467049, 0.8251162403339853402, -27.44695267912525694 ) ) ;
#23695 = VECTOR ( 'NONE', #23907, 1000.000000000000227 ) ;
#23696 = CARTESIAN_POINT ( 'NONE',  ( -11.07177992392671939, 13.25002113301073159, 20.82122704794080903 ) ) ;
#23697 = CARTESIAN_POINT ( 'NONE',  ( 18.40750778688494904, -18.65192611823397328, 20.82122704794068113 ) ) ;
#23698 = CARTESIAN_POINT ( 'NONE',  ( -13.47830981910552772, 21.58612669357095015, 9.500000000000000000 ) ) ;
#23699 = ADVANCED_FACE ( 'NONE', ( #32079 ), #32290, .T. ) ;
#23700 = LINE ( 'NONE', #2171, #6045 ) ;
#23701 = LINE ( 'NONE', #5607, #26504 ) ;
#23702 = VERTEX_POINT ( 'NONE', #13181 ) ;
#23703 = CARTESIAN_POINT ( 'NONE',  ( 13.94482798346721175, 26.50521816028912525, 7.000000000000000000 ) ) ;
#23704 = CONICAL_SURFACE ( 'NONE', #6185, 0.4999999999999947264, 0.7853981633974468357 ) ;
#23705 = CARTESIAN_POINT ( 'NONE',  ( 6.392125613574994425, 35.62765252371730895, 10.99387789255783687 ) ) ;
#23706 = CARTESIAN_POINT ( 'NONE',  ( 7.330070799514983193, 27.28854476845134513, 12.00000000000000000 ) ) ;
#23707 = CARTESIAN_POINT ( 'NONE',  ( 0.4114189264675339741, 38.49512827994399800, -5.000000000000003553 ) ) ;
#23708 = DIRECTION ( 'NONE',  ( -0.9781476007338070211, -0.2079116908177534029, 0.000000000000000000 ) ) ;
#23709 = EDGE_CURVE ( 'NONE', #32281, #18451, #27151, .T. ) ;
#23710 = CARTESIAN_POINT ( 'NONE',  ( 17.28285333400959445, 27.30382183500221771, 12.14047268033097282 ) ) ;
#23711 = EDGE_CURVE ( 'NONE', #10646, #3986, #25834, .T. ) ;
#23712 = AXIS2_PLACEMENT_3D ( 'NONE', #4378, #10076, #31605 ) ;
#23713 = CARTESIAN_POINT ( 'NONE',  ( -8.927394655428429360, 11.06314620770957013, 7.000000000000000000 ) ) ;
#23714 = CARTESIAN_POINT ( 'NONE',  ( -6.354454053420243831, 35.54304081427989814, 7.000000000000000000 ) ) ;
#23715 = DIRECTION ( 'NONE',  ( 1.000000000000000000, 0.000000000000000000, 0.000000000000000000 ) ) ;
#23716 = CARTESIAN_POINT ( 'NONE',  ( 11.15866139110228161, 21.00416962748823480, -20.35793133617824680 ) ) ;
#23718 = VECTOR ( 'NONE', #24308, 1000.000000000000114 ) ;
#23717 = FACE_OUTER_BOUND ( 'NONE', #7598, .T. ) ;
#23719 = EDGE_LOOP ( 'NONE', ( #20790, #449, #1182, #34687 ) ) ;
#23721 = CARTESIAN_POINT ( 'NONE',  ( 6.607858460703812220, 34.88289976392060510, 10.50000000000000000 ) ) ;
#23720 = CARTESIAN_POINT ( 'NONE',  ( -17.86741215881691858, 13.84986514057024287, -17.98417663591535032 ) ) ;
#23722 = DIRECTION ( 'NONE',  ( 0.000000000000000000, 0.000000000000000000, 1.000000000000000000 ) ) ;
#23723 = CARTESIAN_POINT ( 'NONE',  ( 9.723126879071481099, -18.42578174174817462, -26.82764559573607599 ) ) ;
#23724 = CARTESIAN_POINT ( 'NONE',  ( 7.577540944421576441, 33.15743037285414374, 13.00000000000000178 ) ) ;
#23725 = CARTESIAN_POINT ( 'NONE',  ( 10.96431188987212479, 17.32148673788787718, -29.34792031095122056 ) ) ;
#23726 = DIRECTION ( 'NONE',  ( -0.000000000000000000, -0.000000000000000000, -1.000000000000000000 ) ) ;
#23727 = DIRECTION ( 'NONE',  ( 1.000000000000000000, 6.938893903907210234E-15, 0.000000000000000000 ) ) ;
#23728 = CARTESIAN_POINT ( 'NONE',  ( -15.95643642716439814, -14.97217458464374218, -24.37019123110221130 ) ) ;
#23729 = CARTESIAN_POINT ( 'NONE',  ( 2.749517794474013233, -20.36689819698734993, -29.42597746536911885 ) ) ;
#23730 = CARTESIAN_POINT ( 'NONE',  ( 14.43692155601393523, 24.10478420696655633, -12.56460344322019118 ) ) ;
#23731 = CARTESIAN_POINT ( 'NONE',  ( 19.13270401218881389, 10.69174942926454364, -20.12447810330580822 ) ) ;
#23732 = LINE ( 'NONE', #27185, #10868 ) ;
#23733 = ORIENTED_EDGE ( 'NONE', *, *, #24297, .F. ) ;
#23734 = CARTESIAN_POINT ( 'NONE',  ( -5.927024997082391167, 29.01444388681059294, -15.76666309069987904 ) ) ;
#23735 = VERTEX_POINT ( 'NONE', #13992 ) ;
#23736 = EDGE_CURVE ( 'NONE', #34769, #7567, #13789, .T. ) ;
#23737 = CYLINDRICAL_SURFACE ( 'NONE', #17673, 15.00000000000000000 ) ;
#23738 = ORIENTED_EDGE ( 'NONE', *, *, #9015, .F. ) ;
#23739 = LINE ( 'NONE', #14997, #13446 ) ;
#23740 = DIRECTION ( 'NONE',  ( -0.9510565162951543083, -0.3090169943749450088, -0.000000000000000000 ) ) ;
#23741 = ORIENTED_EDGE ( 'NONE', *, *, #28988, .F. ) ;
#23742 = AXIS2_PLACEMENT_3D ( 'NONE', #3880, #1043, #28063 ) ;
#23743 = CARTESIAN_POINT ( 'NONE',  ( -24.46827507224332976, 0.6227895819650135500, -18.47284972081245158 ) ) ;
#23744 = ORIENTED_EDGE ( 'NONE', *, *, #5515, .T. ) ;
#23745 = CARTESIAN_POINT ( 'NONE',  ( 30.96083639235021678, -10.32297208420813384, -12.95559803073687277 ) ) ;
#23746 = AXIS2_PLACEMENT_3D ( 'NONE', #32053, #37004, #16221 ) ;
#23747 = CIRCLE ( 'NONE', #10788, 1.000000000000000888 ) ;
#23748 = VERTEX_POINT ( 'NONE', #10748 ) ;
#23749 = ITEM_DEFINED_TRANSFORMATION ( 'NONE', 'NONE', #22279,  #24238 ) ;
#23750 = CARTESIAN_POINT ( 'NONE',  ( 10.52439982978253674, 33.18839767067679958, 7.382773698552464126 ) ) ;
#23751 = ORIENTED_EDGE ( 'NONE', *, *, #28252, .T. ) ;
#23752 = CARTESIAN_POINT ( 'NONE',  ( 14.97277451176449325, 21.48159783397873923, 10.49999999999999822 ) ) ;
#23753 = DIRECTION ( 'NONE',  ( 0.2079116908177533474, -0.9781476007338067991, 0.000000000000000000 ) ) ;
#23754 = CARTESIAN_POINT ( 'NONE',  ( -4.211402178667006169, 32.38366924255629442, 13.00000000000000178 ) ) ;
#23755 = ORIENTED_EDGE ( 'NONE', *, *, #159, .F. ) ;
#23756 = FILL_AREA_STYLE_COLOUR ( '', #35929 ) ;
#23757 = CARTESIAN_POINT ( 'NONE',  ( 3.100636323082810009, 29.29593658752792962, 6.000000000000000000 ) ) ;
#23758 = CYLINDRICAL_SURFACE ( 'NONE', #22792, 0.4999999999999998335 ) ;
#23759 = CARTESIAN_POINT ( 'NONE',  ( 2.629601561899395534, 7.723830143584016206, 7.000000000000000000 ) ) ;
#23760 = EDGE_CURVE ( 'NONE', #15678, #2130, #23901, .T. ) ;
#23761 = CARTESIAN_POINT ( 'NONE',  ( 17.77173691806767764, 16.90998488025378421, -12.82112725625904659 ) ) ;
#23762 = CARTESIAN_POINT ( 'NONE',  ( 13.08272806821811685, 31.59167807745777523, -6.349128532506149725 ) ) ;
#23763 = ORIENTED_EDGE ( 'NONE', *, *, #27671, .F. ) ;
#23764 = DIRECTION ( 'NONE',  ( 0.000000000000000000, 0.000000000000000000, -1.000000000000000000 ) ) ;
#23765 = CARTESIAN_POINT ( 'NONE',  ( -2.501562340374943183, 7.696614566897864940, 10.49999999999999822 ) ) ;
#23766 = CARTESIAN_POINT ( 'NONE',  ( 15.50750456237632235, -26.45556754333551552, -7.819482178144383511 ) ) ;
#23767 = CARTESIAN_POINT ( 'NONE',  ( 3.229431105722923245, 20.49260818092372460, 6.000000000000000000 ) ) ;
#23768 = VECTOR ( 'NONE', #1645, 1000.000000000000000 ) ;
#23769 = DIRECTION ( 'NONE',  ( 0.1045284632676436315, -0.9945218953682742891, 0.000000000000000000 ) ) ;
#23770 = CARTESIAN_POINT ( 'NONE',  ( -15.39383690649032488, 26.76996700796825479, -5.945875866430524681 ) ) ;
#23771 = AXIS2_PLACEMENT_3D ( 'NONE', #36870, #12477, #39906 ) ;
#23772 = CARTESIAN_POINT ( 'NONE',  ( -22.52485696384032110, -27.93079472553808529, 15.13084544680170218 ) ) ;
#23773 = CARTESIAN_POINT ( 'NONE',  ( 14.00981168397869325, -26.01563153178782528, -8.306567882437748906 ) ) ;
#23774 = CIRCLE ( 'NONE', #2294, 15.00000000000000000 ) ;
#23775 = CARTESIAN_POINT ( 'NONE',  ( -14.84160187385924523, 20.32586711126994672, 7.000000000000000000 ) ) ;
#23776 = ORIENTED_EDGE ( 'NONE', *, *, #18248, .T. ) ;
#23777 = ORIENTED_EDGE ( 'NONE', *, *, #15452, .F. ) ;
#23778 = CARTESIAN_POINT ( 'NONE',  ( -11.25898764560963272, 28.46192956650065753, -13.15053914888870956 ) ) ;
#23779 = CARTESIAN_POINT ( 'NONE',  ( 13.22516817658079802, 40.70288237343621063, 11.00000000000000000 ) ) ;
#23780 = ADVANCED_FACE ( 'NONE', ( #36534 ), #29634, .T. ) ;
#23781 = FACE_OUTER_BOUND ( 'NONE', #20836, .T. ) ;
#23782 = DIRECTION ( 'NONE',  ( 0.000000000000000000, 0.000000000000000000, 1.000000000000000000 ) ) ;
#23783 = ORIENTED_EDGE ( 'NONE', *, *, #355, .T. ) ;
#23784 = CARTESIAN_POINT ( 'NONE',  ( 20.69061391627001711, 0.8884056894011840289, -27.45102547293791417 ) ) ;
#23785 = EDGE_CURVE ( 'NONE', #23843, #3978, #11576, .T. ) ;
#23786 = DIRECTION ( 'NONE',  ( 0.000000000000000000, 0.000000000000000000, 1.000000000000000000 ) ) ;
#23787 = DIRECTION ( 'NONE',  ( -0.9945218953682744001, -0.1045284632676436315, 0.000000000000000000 ) ) ;
#23788 = CARTESIAN_POINT ( 'NONE',  ( -37.32914646357117050, -13.98551220633469150, 10.99999999999993783 ) ) ;
#23789 = ORIENTED_EDGE ( 'NONE', *, *, #38589, .F. ) ;
#23790 = CARTESIAN_POINT ( 'NONE',  ( -25.84690816252402357, 0.3462692498223990945, -16.44622743198997483 ) ) ;
#23791 = DIRECTION ( 'NONE',  ( 0.000000000000000000, 0.000000000000000000, 1.000000000000000000 ) ) ;
#23792 = ORIENTED_EDGE ( 'NONE', *, *, #14509, .T. ) ;
#23793 = CARTESIAN_POINT ( 'NONE',  ( 23.46557895267442362, -3.401122285006365153, -21.14145122161913548 ) ) ;
#23794 = EDGE_CURVE ( 'NONE', #36540, #32987, #20502, .T. ) ;
#23795 = CARTESIAN_POINT ( 'NONE',  ( 27.50471383176380868, -25.75100844545640300, 15.72805884748903971 ) ) ;
#23796 = ORIENTED_EDGE ( 'NONE', *, *, #21849, .F. ) ;
#23797 = CARTESIAN_POINT ( 'NONE',  ( 7.235364705665938700, 38.16413851588617234, 14.53008259254001011 ) ) ;
#23798 = CARTESIAN_POINT ( 'NONE',  ( -16.05557028315303469, -24.54483004364683296, 18.42518152272108978 ) ) ;
#23799 = DIRECTION ( 'NONE',  ( 0.000000000000000000, 0.000000000000000000, 1.000000000000000000 ) ) ;
#23800 = CARTESIAN_POINT ( 'NONE',  ( 3.858525888476776800, 28.90799431746422243, 20.82122704794079837 ) ) ;
#23801 = CIRCLE ( 'NONE', #20567, 1.000000000000000000 ) ;
#23802 = AXIS2_PLACEMENT_3D ( 'NONE', #21379, #38568, #35732 ) ;
#23803 = CARTESIAN_POINT ( 'NONE',  ( -10.06946225350398194, 32.23940090176283491, 7.500000000000005329 ) ) ;
#23804 = ORIENTED_EDGE ( 'NONE', *, *, #1941, .F. ) ;
#23805 = DIRECTION ( 'NONE',  ( 0.000000000000000000, 0.000000000000000000, 1.000000000000000000 ) ) ;
#23806 = CYLINDRICAL_SURFACE ( 'NONE', #27958, 1.000000000000000000 ) ;
#23807 = ADVANCED_FACE ( 'NONE', ( #5647 ), #32697, .T. ) ;
#23808 = ADVANCED_FACE ( 'NONE', ( #39577 ), #14181, .T. ) ;
#23809 = CARTESIAN_POINT ( 'NONE',  ( 3.962059598754420708, 20.50340585479708011, -27.03137393839747560 ) ) ;
#23810 = DIRECTION ( 'NONE',  ( 0.000000000000000000, 0.000000000000000000, 1.000000000000000000 ) ) ;
#23811 = CARTESIAN_POINT ( 'NONE',  ( 23.79662817859708568, 0.8209266585812692307, 19.66345542863611939 ) ) ;
#23812 = CARTESIAN_POINT ( 'NONE',  ( 12.39337453381797616, -17.63539129962619967, -24.72786391051304378 ) ) ;
#23813 = CARTESIAN_POINT ( 'NONE',  ( -12.03641663870442713, 15.85735326529964873, 12.00000000000000000 ) ) ;
#23814 = LINE ( 'NONE', #33176, #33266 ) ;
#23815 = FACE_BOUND ( 'NONE', #12304, .T. ) ;
#23816 = ORIENTED_EDGE ( 'NONE', *, *, #38451, .F. ) ;
#23817 = CARTESIAN_POINT ( 'NONE',  ( 10.91660561822348896, 17.40535124426578761, -28.70322919763274783 ) ) ;
#23818 = ORIENTED_EDGE ( 'NONE', *, *, #8407, .F. ) ;
#23819 = CARTESIAN_POINT ( 'NONE',  ( -11.77357070864453092, 18.18633671150151443, -23.89743119366780633 ) ) ;
#23820 = CARTESIAN_POINT ( 'NONE',  ( -32.25947621352474215, -13.82181017473423346, 18.87996532025784191 ) ) ;
#23821 = CYLINDRICAL_SURFACE ( 'NONE', #30213, 0.5000000000000001110 ) ;
#23822 = CARTESIAN_POINT ( 'NONE',  ( 14.57902638507616366, 24.84342498027717383, -11.60275616826175948 ) ) ;
#23823 = ORIENTED_EDGE ( 'NONE', *, *, #28735, .T. ) ;
#23824 = CARTESIAN_POINT ( 'NONE',  ( 31.14704341106911656, -19.74704749676938675, -9.282700252451727252 ) ) ;
#23825 = EDGE_LOOP ( 'NONE', ( #33727, #39828 ) ) ;
#23827 = DIRECTION ( 'NONE',  ( -0.000000000000000000, -0.000000000000000000, -1.000000000000000000 ) ) ;
#23826 = CARTESIAN_POINT ( 'NONE',  ( -14.95020005163037702, 26.98781491602204952, -8.271018971934079644 ) ) ;
#23828 = CARTESIAN_POINT ( 'NONE',  ( -18.24387349984239037, -27.08452756295628205, -6.833357348710000778 ) ) ;
#23829 = ADVANCED_FACE ( 'NONE', ( #23542 ), #17666, .T. ) ;
#23830 = DIRECTION ( 'NONE',  ( 0.9510565162951538642, 0.3090169943749465631, 0.000000000000000000 ) ) ;
#23831 = VECTOR ( 'NONE', #27881, 999.9999999999998863 ) ;
#23832 = AXIS2_PLACEMENT_3D ( 'NONE', #749, #36931, #9097 ) ;
#23833 = ORIENTED_EDGE ( 'NONE', *, *, #15926, .T. ) ;
#23834 = CARTESIAN_POINT ( 'NONE',  ( -19.25070363287986197, -7.311498989063264453, -28.46895897768014905 ) ) ;
#23835 = CARTESIAN_POINT ( 'NONE',  ( -9.241419177041928279, -18.43513586380258573, -28.09520835628508095 ) ) ;
#23836 = CARTESIAN_POINT ( 'NONE',  ( -14.48927117870122316, -30.61587158504648087, 23.00000000000000000 ) ) ;
#23837 = ORIENTED_EDGE ( 'NONE', *, *, #29653, .T. ) ;
#23838 = CARTESIAN_POINT ( 'NONE',  ( 27.69967049059682296, 2.038585896039051271, -10.70918416779063165 ) ) ;
#23839 = EDGE_CURVE ( 'NONE', #19392, #3779, #36895, .T. ) ;
#23840 = DIRECTION ( 'NONE',  ( 0.000000000000000000, 0.000000000000000000, 1.000000000000000000 ) ) ;
#23841 = CARTESIAN_POINT ( 'NONE',  ( -39.51968005975108866, -13.07391886567259220, 11.00000000000000000 ) ) ;
#23842 = VECTOR ( 'NONE', #10661, 1000.000000000000000 ) ;
#23843 = VERTEX_POINT ( 'NONE', #26588 ) ;
#23844 = CARTESIAN_POINT ( 'NONE',  ( -20.48527248842334458, 0.7769947089114559446, -29.34686795096567380 ) ) ;
#23845 = CARTESIAN_POINT ( 'NONE',  ( 32.07997776912482379, -1.415336196370684529, -5.928950972838648248 ) ) ;
#23846 = AXIS2_PLACEMENT_3D ( 'NONE', #13708, #22445, #19816 ) ;
#23847 = CARTESIAN_POINT ( 'NONE',  ( 31.98112326865622279, -15.20435932463063899, 18.87996532025785967 ) ) ;
#23848 = ORIENTED_EDGE ( 'NONE', *, *, #21338, .F. ) ;
#23849 = CARTESIAN_POINT ( 'NONE',  ( -25.95428780700007820, 2.674197598944707099, -13.64957008435976960 ) ) ;
#23850 = CARTESIAN_POINT ( 'NONE',  ( 12.05832241004688399, 18.99596958976722760, -21.04195414767209726 ) ) ;
#23851 = CARTESIAN_POINT ( 'NONE',  ( 8.368303251206119953, 20.48707633493483371, 9.000000000000001776 ) ) ;
#23852 = CARTESIAN_POINT ( 'NONE',  ( -15.74227866054087066, -25.75916161678338057, 17.42190598798392998 ) ) ;
#23853 = AXIS2_PLACEMENT_3D ( 'NONE', #30087, #14849, #36386 ) ;
#23854 = AXIS2_PLACEMENT_3D ( 'NONE', #1967, #14544, #18006 ) ;
#23855 = CARTESIAN_POINT ( 'NONE',  ( -2.369380564245688436, 7.688150949816208168, 7.455686640544898935 ) ) ;
#23856 = DIRECTION ( 'NONE',  ( 0.000000000000000000, 0.000000000000000000, 1.000000000000000000 ) ) ;
#23857 = CARTESIAN_POINT ( 'NONE',  ( -2.494943660522439099, 10.76222879119470832, 6.000000000000000000 ) ) ;
#23858 = ORIENTED_EDGE ( 'NONE', *, *, #37201, .T. ) ;
#23859 = CARTESIAN_POINT ( 'NONE',  ( -19.97087465710904652, 5.004486353843795143, -28.23393442912554008 ) ) ;
#23860 = CYLINDRICAL_SURFACE ( 'NONE', #10571, 0.5000000000000002220 ) ;
#23861 = DIRECTION ( 'NONE',  ( 1.000000000000000000, 0.000000000000000000, 0.000000000000000000 ) ) ;
#23862 = CARTESIAN_POINT ( 'NONE',  ( 22.07789268346514433, -22.99653480363242153, -13.02319493230320724 ) ) ;
#23863 = EDGE_CURVE ( 'NONE', #13219, #36438, #5015, .T. ) ;
#23864 = DIRECTION ( 'NONE',  ( 1.000000000000000000, 0.000000000000000000, 0.000000000000000000 ) ) ;
#23865 = CARTESIAN_POINT ( 'NONE',  ( -14.36830325120615903, 20.48707633493503621, 11.00000000000000355 ) ) ;
#23866 = CARTESIAN_POINT ( 'NONE',  ( 14.11939125880675938, 24.91404824547022301, -12.51327720378664310 ) ) ;
#23867 = AXIS2_PLACEMENT_3D ( 'NONE', #26940, #10906, #1762 ) ;
#23868 = CARTESIAN_POINT ( 'NONE',  ( -14.98890121934409869, -28.67928442654153542, 11.55979286843934872 ) ) ;
#23869 = EDGE_LOOP ( 'NONE', ( #654, #56, #8480, #17540 ) ) ;
#23870 = CARTESIAN_POINT ( 'NONE',  ( -13.97090665946301336, 15.18147329247454280, -27.63196484367346883 ) ) ;
#23871 = CARTESIAN_POINT ( 'NONE',  ( -22.04303751225598873, -17.34387783897684443, 20.94377226548378346 ) ) ;
#23872 = CARTESIAN_POINT ( 'NONE',  ( -9.593266739736645121, 18.11602540378452986, 10.50000000000000000 ) ) ;
#23873 = CARTESIAN_POINT ( 'NONE',  ( 15.38381738949339272, 26.63070857578979300, -6.417047948954210490 ) ) ;
#23874 = EDGE_LOOP ( 'NONE', ( #20136, #35527, #40126 ) ) ;
#23875 = CARTESIAN_POINT ( 'NONE',  ( 11.89393184209720111, 19.38028970819424757, -21.61737904418153988 ) ) ;
#23876 = ORIENTED_EDGE ( 'NONE', *, *, #40180, .F. ) ;
#23878 = CARTESIAN_POINT ( 'NONE',  ( -6.354454053420243831, 35.54304081427989814, 7.000000000000000000 ) ) ;
#23877 = CARTESIAN_POINT ( 'NONE',  ( -13.15316605911461245, 22.33945200540117426, -16.43108139302208315 ) ) ;
#23879 = CARTESIAN_POINT ( 'NONE',  ( -13.09026340579413628, -23.09710496079592446, -15.44275337101657186 ) ) ;
#23880 = CARTESIAN_POINT ( 'NONE',  ( -27.36225479889090906, 10.16098284204026569, 11.00000000000000178 ) ) ;
#23881 = CARTESIAN_POINT ( 'NONE',  ( -32.00223536558479509, -16.75185194936180011, -10.17489710537347669 ) ) ;
#23882 = CARTESIAN_POINT ( 'NONE',  ( -8.966847780561042924, -24.82021992796463294, -9.807061091129195773 ) ) ;
#23883 = CARTESIAN_POINT ( 'NONE',  ( -23.19735768193462278, -14.64350930037788423, 21.00000000000000355 ) ) ;
#23884 = CARTESIAN_POINT ( 'NONE',  ( 12.15445636706326482, 17.84729731487952265, -23.95206648447458164 ) ) ;
#23885 = VERTEX_POINT ( 'NONE', #2215 ) ;
#23886 = CARTESIAN_POINT ( 'NONE',  ( 24.51742203815395982, 7.367698884986912056, -7.410464452778436240 ) ) ;
#23887 = CARTESIAN_POINT ( 'NONE',  ( 8.927394655428274817, 11.06314620770945290, 7.000000000000000000 ) ) ;
#23888 = DIRECTION ( 'NONE',  ( 0.000000000000000000, 0.000000000000000000, 1.000000000000000000 ) ) ;
#23889 = DIRECTION ( 'NONE',  ( 0.000000000000000000, 0.000000000000000000, 1.000000000000000000 ) ) ;
#23890 = ORIENTED_EDGE ( 'NONE', *, *, #9638, .F. ) ;
#23891 = CARTESIAN_POINT ( 'NONE',  ( -23.66820407423360351, -0.4863796308273267699, -20.40241117499521906 ) ) ;
#23893 = CARTESIAN_POINT ( 'NONE',  ( 30.78377185402874971, -0.09069996828062186489, -6.886088703951912748 ) ) ;
#23892 = VECTOR ( 'NONE', #14400, 1000.000000000000000 ) ;
#23894 = AXIS2_PLACEMENT_3D ( 'NONE', #5749, #30935, #34383 ) ;
#23895 = DIRECTION ( 'NONE',  ( 0.8386705679454212747, -0.5446390350150315252, 0.000000000000000000 ) ) ;
#23896 = CARTESIAN_POINT ( 'NONE',  ( 25.56674216509423658, -13.93466449336444413, 20.94377226548378346 ) ) ;
#23897 = ADVANCED_FACE ( 'NONE', ( #7894 ), #8706, .T. ) ;
#23898 = AXIS2_PLACEMENT_3D ( 'NONE', #3113, #15700, #15509 ) ;
#23899 = CARTESIAN_POINT ( 'NONE',  ( -8.472151273871419974, 28.78272654129072095, 10.49999999999999822 ) ) ;
#23901 = CIRCLE ( 'NONE', #6365, 0.4999999999999997780 ) ;
#23900 = CYLINDRICAL_SURFACE ( 'NONE', #4366, 15.99999999999999645 ) ;
#23902 = ORIENTED_EDGE ( 'NONE', *, *, #14241, .T. ) ;
#23903 = CARTESIAN_POINT ( 'NONE',  ( 14.96930490892014554, 21.54088032874971859, 7.500000000000010658 ) ) ;
#23904 = CARTESIAN_POINT ( 'NONE',  ( 6.832768599201303417, 35.70122713809256254, 10.49999999999999822 ) ) ;
#23905 = CARTESIAN_POINT ( 'NONE',  ( -1.547498115756908321, 8.004992253133190516, 7.000000000000000000 ) ) ;
#23906 = CARTESIAN_POINT ( 'NONE',  ( 0.4103210871597268716, 38.34576889810298894, -6.276193439666084117 ) ) ;
#23907 = DIRECTION ( 'NONE',  ( 0.1045284632676436176, -0.9945218953682742891, -0.000000000000000000 ) ) ;
#23908 = EDGE_CURVE ( 'NONE', #25824, #21424, #11356, .T. ) ;
#23909 = DIRECTION ( 'NONE',  ( 0.000000000000000000, 0.000000000000000000, 1.000000000000000000 ) ) ;
#23910 = DIRECTION ( 'NONE',  ( -0.000000000000000000, -0.000000000000000000, -1.000000000000000000 ) ) ;
#23911 = DIRECTION ( 'NONE',  ( 1.000000000000000000, 0.000000000000000000, 0.000000000000000000 ) ) ;
#23913 = EDGE_CURVE ( 'NONE', #26292, #24105, #17450, .T. ) ;
#23912 = DIRECTION ( 'NONE',  ( 1.000000000000000000, 0.000000000000000000, 0.000000000000000000 ) ) ;
#23914 = CARTESIAN_POINT ( 'NONE',  ( -18.23649648353769948, -16.09146789626166196, 23.00000000000000000 ) ) ;
#23915 = VECTOR ( 'NONE', #13646, 1000.000000000000000 ) ;
#23916 = CARTESIAN_POINT ( 'NONE',  ( 9.842964772816607422, 17.98588232539188425, -29.32391334795786975 ) ) ;
#23917 = DIRECTION ( 'NONE',  ( -0.9945218953682746221, -0.1045284632676422437, -0.000000000000000000 ) ) ;
#23918 = CIRCLE ( 'NONE', #13528, 1.000000000000000222 ) ;
#23919 = ORIENTED_EDGE ( 'NONE', *, *, #11339, .F. ) ;
#23921 = DIRECTION ( 'NONE',  ( -0.000000000000000000, -0.000000000000000000, -1.000000000000000000 ) ) ;
#23920 = CARTESIAN_POINT ( 'NONE',  ( -16.78989029355724583, 13.95002842669032006, -21.11808514744672749 ) ) ;
#23922 = EDGE_CURVE ( 'NONE', #27126, #12690, #23739, .T. ) ;
#23923 = CARTESIAN_POINT ( 'NONE',  ( 8.843266739736574067, 16.81698729810774395, 10.00000000000000000 ) ) ;
#23924 = CARTESIAN_POINT ( 'NONE',  ( 15.20883357874183517, -26.29087852017448057, -8.296495227514824933 ) ) ;
#23925 = ADVANCED_FACE ( 'NONE', ( #8306 ), #8502, .F. ) ;
#23926 = CARTESIAN_POINT ( 'NONE',  ( 13.48758456246937065, 22.82324740036665744, -15.44989232396192236 ) ) ;
#23927 = CARTESIAN_POINT ( 'NONE',  ( 12.12035967098243283, 19.93664080562797025, -20.53879709934572162 ) ) ;
#23928 = AXIS2_PLACEMENT_3D ( 'NONE', #30458, #5654, #27594 ) ;
#23929 = CARTESIAN_POINT ( 'NONE',  ( -32.33143948542088708, 1.358872982498823268, -5.000000000000000888 ) ) ;
#23930 = LINE ( 'NONE', #2400, #23215 ) ;
#23931 = CARTESIAN_POINT ( 'NONE',  ( -27.24402026484078476, -22.73710829990762861, -10.20726825364095269 ) ) ;
#23932 = CARTESIAN_POINT ( 'NONE',  ( 4.543046482400002972, -20.88912539285810155, -23.23170238819161426 ) ) ;
#23933 = CARTESIAN_POINT ( 'NONE',  ( 12.80356091706831556, 20.83509046290971156, -18.47796576163459648 ) ) ;
#23934 = CARTESIAN_POINT ( 'NONE',  ( 19.82717930584050947, 11.06638669728694602, -16.98486891981015390 ) ) ;
#23935 = DIRECTION ( 'NONE',  ( 1.000000000000000000, 0.000000000000000000, 0.000000000000000000 ) ) ;
#23936 = ORIENTED_EDGE ( 'NONE', *, *, #31583, .T. ) ;
#23937 = CARTESIAN_POINT ( 'NONE',  ( -6.355925524898499823, 36.92694055957776555, -6.714009213630858675 ) ) ;
#23938 = ORIENTED_EDGE ( 'NONE', *, *, #35340, .F. ) ;
#23939 = CARTESIAN_POINT ( 'NONE',  ( -25.43795106045734045, 8.821996438890993275, 13.32518128616756314 ) ) ;
#23940 = ORIENTED_EDGE ( 'NONE', *, *, #39678, .T. ) ;
#23941 = DIRECTION ( 'NONE',  ( 0.000000000000000000, 0.000000000000000000, 1.000000000000000000 ) ) ;
#23942 = EDGE_CURVE ( 'NONE', #22931, #16537, #33100, .T. ) ;
#23943 = CARTESIAN_POINT ( 'NONE',  ( -3.503793317224517700, 8.420815634768727520, 9.000000000000001776 ) ) ;
#23944 = ADVANCED_FACE ( 'NONE', ( #20900 ), #33303, .T. ) ;
#23945 = ORIENTED_EDGE ( 'NONE', *, *, #32250, .T. ) ;
#23946 = CARTESIAN_POINT ( 'NONE',  ( -30.47170454527866923, 0.4016671284418433796, -4.999999999999999112 ) ) ;
#23947 = CARTESIAN_POINT ( 'NONE',  ( 28.06320634686874627, -9.371851771698166189, -15.76881348996817067 ) ) ;
#23948 = VECTOR ( 'NONE', #23419, 1000.000000000000000 ) ;
#23949 = AXIS2_PLACEMENT_3D ( 'NONE', #11534, #23921, #27171 ) ;
#23950 = EDGE_LOOP ( 'NONE', ( #29116, #21767, #18842, #34859 ) ) ;
#23951 = ITEM_DEFINED_TRANSFORMATION ( 'NONE', 'NONE', #2834,  #24238 ) ;
#23952 = CARTESIAN_POINT ( 'NONE',  ( -35.48557158514988430, -11.25000000000002309, 10.00000000000000000 ) ) ;
#23953 = EDGE_LOOP ( 'NONE', ( #32454, #25450, #14048, #14042 ) ) ;
#23954 = AXIS2_PLACEMENT_3D ( 'NONE', #6743, #28091, #25048 ) ;
#23955 = DIRECTION ( 'NONE',  ( -0.8090169943749426773, 0.5877852522924796874, 0.000000000000000000 ) ) ;
#23956 = CARTESIAN_POINT ( 'NONE',  ( -6.654030453887829211, 35.94335816374515247, 7.500000000000000888 ) ) ;
#23957 = CARTESIAN_POINT ( 'NONE',  ( 12.05736835487432579, 14.38397459621550567, 11.00000000000000000 ) ) ;
#23958 = ORIENTED_EDGE ( 'NONE', *, *, #20844, .F. ) ;
#23959 = SURFACE_STYLE_USAGE ( .BOTH. , #20724 ) ;
#23960 = CARTESIAN_POINT ( 'NONE',  ( 12.80736835487433289, 15.68301270189216545, 7.000000000000000000 ) ) ;
#23961 = CARTESIAN_POINT ( 'NONE',  ( 5.688300058587269170, 16.47782454277055564, 12.00000000000000000 ) ) ;
#23962 = DIRECTION ( 'NONE',  ( 1.000000000000000000, 0.000000000000000000, 0.000000000000000000 ) ) ;
#23963 = ADVANCED_FACE ( 'NONE', ( #30243 ), #2412, .T. ) ;
#23964 = CARTESIAN_POINT ( 'NONE',  ( 16.84224471403853229, 14.37780181299635984, -20.04792273672603997 ) ) ;
#23965 = CARTESIAN_POINT ( 'NONE',  ( 9.502174681210730611, 24.54420635781409388, -17.97437483132709701 ) ) ;
#23966 = ORIENTED_EDGE ( 'NONE', *, *, #12614, .T. ) ;
#23967 = CARTESIAN_POINT ( 'NONE',  ( -21.48623309969284989, 11.60342812567675885, -9.394375087043044914 ) ) ;
#23968 = DIRECTION ( 'NONE',  ( 0.000000000000000000, 0.000000000000000000, 1.000000000000000000 ) ) ;
#23969 = DIRECTION ( 'NONE',  ( -0.2185080122244173473, -0.6724985119639624864, -0.7071067811865404673 ) ) ;
#23970 = CARTESIAN_POINT ( 'NONE',  ( 10.09390139374666262, -18.42364844336855256, -26.19501470389041842 ) ) ;
#23971 = CARTESIAN_POINT ( 'NONE',  ( 21.24426311945340373, 15.07158936841588215, 11.00000000000000000 ) ) ;
#23972 = CARTESIAN_POINT ( 'NONE',  ( 27.08779848459123585, 7.221796966026763798, -5.000000000000007105 ) ) ;
#23974 = VECTOR ( 'NONE', #19204, 999.9999999999998863 ) ;
#23973 = CARTESIAN_POINT ( 'NONE',  ( -12.92966971681751431, 21.65081211195085942, -17.43791612333144414 ) ) ;
#23975 = CARTESIAN_POINT ( 'NONE',  ( -20.88456819748228810, -23.43278618219788711, -13.06947050431665858 ) ) ;
#23976 = CARTESIAN_POINT ( 'NONE',  ( 13.62892564869307854, -25.43202621200122948, -10.20098705052232724 ) ) ;
#23977 = CARTESIAN_POINT ( 'NONE',  ( -1.000000000000000000, 37.00000000000000711, 7.000000000000000000 ) ) ;
#23978 = EDGE_LOOP ( 'NONE', ( #3851, #38671 ) ) ;
#23979 = EDGE_LOOP ( 'NONE', ( #29031, #16778, #31429, #10071, #3540 ) ) ;
#23980 = AXIS2_PLACEMENT_3D ( 'NONE', #20518, #30462, #2229 ) ;
#23981 = CARTESIAN_POINT ( 'NONE',  ( -7.677290147211061289, 19.01944725762398392, -29.99999999999998934 ) ) ;
#23982 = DIRECTION ( 'NONE',  ( 0.000000000000000000, 0.000000000000000000, 1.000000000000000000 ) ) ;
#23983 = CARTESIAN_POINT ( 'NONE',  ( -12.29179778625728403, 14.31343464431660628, 10.49999999999999822 ) ) ;
#23984 = CARTESIAN_POINT ( 'NONE',  ( 5.237540274239915306, 35.49300472853430222, 7.500000000000000888 ) ) ;
#23985 = ORIENTED_EDGE ( 'NONE', *, *, #24789, .F. ) ;
#23986 = CARTESIAN_POINT ( 'NONE',  ( 28.27163672435500530, 0.2247573307824139721, -12.55420016491700608 ) ) ;
#23987 = CARTESIAN_POINT ( 'NONE',  ( -10.44103466624267540, 32.57396620494226624, 11.00000000000000000 ) ) ;
#23988 = PLANE ( 'NONE',  #23853 ) ;
#23989 = ADVANCED_FACE ( 'NONE', ( #24734 ), #6443, .T. ) ;
#23990 = ORIENTED_EDGE ( 'NONE', *, *, #4044, .F. ) ;
#23991 = CARTESIAN_POINT ( 'NONE',  ( -22.21514529423838979, 0.6880714958666251935, -22.73802149961197472 ) ) ;
#23992 = DIRECTION ( 'NONE',  ( 0.9945218953682730678, -0.1045284632676569819, 0.000000000000000000 ) ) ;
#23993 = ORIENTED_EDGE ( 'NONE', *, *, #37086, .T. ) ;
#23994 = CARTESIAN_POINT ( 'NONE',  ( 33.42451262833972692, -5.048360147377955798, -8.566326254722081757 ) ) ;
#23995 = CARTESIAN_POINT ( 'NONE',  ( 37.24966284334288247, -10.92205745603815714, 13.32518128616603015 ) ) ;
#23996 = ORIENTED_EDGE ( 'NONE', *, *, #34472, .T. ) ;
#23997 = CARTESIAN_POINT ( 'NONE',  ( -15.50250408130212421, 30.73387816234496484, 13.92931973827792191 ) ) ;
#23998 = DIRECTION ( 'NONE',  ( -0.5254827454987676116, -0.4731467892558093857, -0.7071067811865447972 ) ) ;
#23999 = CARTESIAN_POINT ( 'NONE',  ( 0.000000000000000000, 22.50000000000000355, 6.000000000000000000 ) ) ;
#24000 = CARTESIAN_POINT ( 'NONE',  ( 4.288075229727362547, 29.62123851724225077, 20.69868183039781329 ) ) ;
#24001 = AXIS2_PLACEMENT_3D ( 'NONE', #18175, #2727, #30955 ) ;
#24002 = CARTESIAN_POINT ( 'NONE',  ( 4.000124606132156480, 8.490627681068716015, 10.49999999999999822 ) ) ;
#24003 = ORIENTED_EDGE ( 'NONE', *, *, #73, .T. ) ;
#24004 = CARTESIAN_POINT ( 'NONE',  ( -16.81416712651214951, 27.17354907310119572, 13.92931973827808712 ) ) ;
#24005 = DIRECTION ( 'NONE',  ( 0.4446959099295487161, 0.6847716512521470067, 0.5773502691896305050 ) ) ;
#24006 = AXIS2_PLACEMENT_3D ( 'NONE', #10509, #4414, #10111 ) ;
#24007 = EDGE_CURVE ( 'NONE', #14195, #22764, #14556, .T. ) ;
#24008 = CARTESIAN_POINT ( 'NONE',  ( 6.458614852237183790, 33.04048157560279009, -12.02760640721125363 ) ) ;
#24009 = CYLINDRICAL_SURFACE ( 'NONE', #34031, 1.000000000000000888 ) ;
#24010 = EDGE_CURVE ( 'NONE', #2130, #16315, #360, .T. ) ;
#24011 = CARTESIAN_POINT ( 'NONE',  ( 27.71565130972690127, -3.171757977843685961, 19.66345542862528362 ) ) ;
#24012 = CARTESIAN_POINT ( 'NONE',  ( 18.56734095888186786, -27.10473135465256433, -6.828420776304507278 ) ) ;
#24013 = CARTESIAN_POINT ( 'NONE',  ( 2.853166178176219425, 23.42705098312512746, 13.00000000000000178 ) ) ;
#24014 = CARTESIAN_POINT ( 'NONE',  ( -18.00000000000000000, 22.50000000000000355, 11.00000000000000178 ) ) ;
#24015 = CARTESIAN_POINT ( 'NONE',  ( -4.835137251120299240, 29.44922644035488446, 6.000000000000000000 ) ) ;
#24016 = VERTEX_POINT ( 'NONE', #18452 ) ;
#24017 = CARTESIAN_POINT ( 'NONE',  ( 12.86711912072691177, 21.75488451896397279, -17.42369386892843863 ) ) ;
#24018 = EDGE_LOOP ( 'NONE', ( #21808, #2511, #17354, #31506 ) ) ;
#24019 = CARTESIAN_POINT ( 'NONE',  ( -13.99681549934592084, 22.91249579894840949, -14.50524598184051150 ) ) ;
#24020 = VECTOR ( 'NONE', #25791, 1000.000000000000000 ) ;
#24021 = EDGE_CURVE ( 'NONE', #23635, #14685, #12236, .T. ) ;
#24022 = CARTESIAN_POINT ( 'NONE',  ( -28.56250045050152409, -21.55178514600735440, 18.42518152272108978 ) ) ;
#24023 = LINE ( 'NONE', #36417, #2352 ) ;
#24024 = CARTESIAN_POINT ( 'NONE',  ( 15.22753785222040435, 26.10542462839032041, -8.299041287613635021 ) ) ;
#24025 = ORIENTED_EDGE ( 'NONE', *, *, #9858, .F. ) ;
#24026 = CARTESIAN_POINT ( 'NONE',  ( 29.11864404320880340, -18.46465774631702672, -11.97498759040503913 ) ) ;
#24027 = ORIENTED_EDGE ( 'NONE', *, *, #7045, .T. ) ;
#24029 = FACE_OUTER_BOUND ( 'NONE', #29501, .T. ) ;
#24028 = CARTESIAN_POINT ( 'NONE',  ( -11.54653377988851304, 19.74306190993011256, -21.55203727238154343 ) ) ;
#24030 = CARTESIAN_POINT ( 'NONE',  ( -11.33884614197604890, -19.32953085267849502, -22.62991861938991889 ) ) ;
#24031 = CARTESIAN_POINT ( 'NONE',  ( 13.53280532430061989, 27.77329351534933721, 10.66666666666666607 ) ) ;
#24032 = ORIENTED_EDGE ( 'NONE', *, *, #32599, .F. ) ;
#24033 = CARTESIAN_POINT ( 'NONE',  ( -19.17275462598830060, -7.282501898908932958, -29.22487285613485852 ) ) ;
#24034 = UNCERTAINTY_MEASURE_WITH_UNIT (LENGTH_MEASURE( 1.000000000000000082E-05 ), #14816, 'distance_accuracy_value', 'NONE');
#24035 = CARTESIAN_POINT ( 'NONE',  ( -14.56418105446348932, -25.61681370524265589, -10.18385066514556669 ) ) ;
#24036 = LINE ( 'NONE', #33196, #27429 ) ;
#24037 = ORIENTED_EDGE ( 'NONE', *, *, #9132, .T. ) ;
#24038 = CARTESIAN_POINT ( 'NONE',  ( 26.85566260921343584, 2.066112236289315174, -12.63869616061161061 ) ) ;
#24039 = CARTESIAN_POINT ( 'NONE',  ( 13.01837422881150452, 21.26636931122159169, 12.00000000000000000 ) ) ;
#24040 = DIRECTION ( 'NONE',  ( 0.000000000000000000, 0.000000000000000000, 1.000000000000000000 ) ) ;
#24041 = EDGE_CURVE ( 'NONE', #22404, #13041, #38837, .T. ) ;
#24042 = VECTOR ( 'NONE', #18415, 1000.000000000000000 ) ;
#24043 = ORIENTED_EDGE ( 'NONE', *, *, #14080, .F. ) ;
#24044 = ADVANCED_FACE ( 'NONE', ( #15596 ), #21490, .F. ) ;
#24045 = CARTESIAN_POINT ( 'NONE',  ( -20.48447659325206516, 0.7979435291051002466, -30.00000000000000000 ) ) ;
#24047 = EDGE_CURVE ( 'NONE', #19728, #23375, #5110, .T. ) ;
#24046 = ORIENTED_EDGE ( 'NONE', *, *, #30399, .T. ) ;
#24048 = CARTESIAN_POINT ( 'NONE',  ( 31.18558700419108831, -0.9481828064721339322, -8.253045886946059895 ) ) ;
#24049 = CARTESIAN_POINT ( 'NONE',  ( 28.17486335742866643, -23.56478353225200095, 17.42190598798355339 ) ) ;
#24050 = ORIENTED_EDGE ( 'NONE', *, *, #20389, .F. ) ;
#24051 = CARTESIAN_POINT ( 'NONE',  ( -27.66981915501925826, 3.518264008085504546, -5.475398431093116081 ) ) ;
#24052 = CARTESIAN_POINT ( 'NONE',  ( 4.984135866956514782, 36.15314577889351000, 7.000000000000000000 ) ) ;
#24053 = DIRECTION ( 'NONE',  ( -1.224646799147351235E-16, 1.000000000000000000, 0.000000000000000000 ) ) ;
#24054 = AXIS2_PLACEMENT_3D ( 'NONE', #37835, #22387, #10008 ) ;
#24055 = CARTESIAN_POINT ( 'NONE',  ( 11.48173768534036121, 32.16538668264416145, 10.49999999999999822 ) ) ;
#24056 = DIRECTION ( 'NONE',  ( -0.1045284632676422437, 0.9945218953682746221, 0.000000000000000000 ) ) ;
#24057 = ADVANCED_FACE ( 'NONE', ( #18255 ), #156, .T. ) ;
#24058 = FACE_BOUND ( 'NONE', #30039, .T. ) ;
#24059 = EDGE_CURVE ( 'NONE', #19420, #22904, #18079, .T. ) ;
#24060 = DIRECTION ( 'NONE',  ( 0.000000000000000000, 0.000000000000000000, 1.000000000000000000 ) ) ;
#24061 = ORIENTED_EDGE ( 'NONE', *, *, #13311, .T. ) ;
#24062 = CARTESIAN_POINT ( 'NONE',  ( -26.09954572027081454, 5.304898449170225128, -6.914248030060270445 ) ) ;
#24063 = DIRECTION ( 'NONE',  ( 0.9945218953682729568, -0.1045284632676570929, -0.000000000000000000 ) ) ;
#24064 = DIRECTION ( 'NONE',  ( -0.4067366430758009299, -0.9135454576426005335, 0.000000000000000000 ) ) ;
#24065 = CARTESIAN_POINT ( 'NONE',  ( 24.71631120996009656, -24.23736600738799396, -10.25405846535409538 ) ) ;
#24066 = AXIS2_PLACEMENT_3D ( 'NONE', #16265, #15463, #37397 ) ;
#24067 = CARTESIAN_POINT ( 'NONE',  ( 34.47241746879583957, 3.460351812918713854, 3.000000000000000000 ) ) ;
#24068 = CARTESIAN_POINT ( 'NONE',  ( 10.70229295774111478, 17.48483442551455269, -29.34227022712989452 ) ) ;
#24069 = CARTESIAN_POINT ( 'NONE',  ( -10.09822582592840590, -27.41751403068705528, 11.00000000001392308 ) ) ;
#24070 = ORIENTED_EDGE ( 'NONE', *, *, #37352, .T. ) ;
#24071 = CARTESIAN_POINT ( 'NONE',  ( -16.07951411908364392, 20.32485814370012633, -12.71120202138577504 ) ) ;
#24072 = CARTESIAN_POINT ( 'NONE',  ( -25.95165700074868553, -9.707988825434739510, 20.94377226548358806 ) ) ;
#24073 = CARTESIAN_POINT ( 'NONE',  ( -36.48557158514989140, -11.24999999999987743, 10.00000000000000000 ) ) ;
#24074 = CARTESIAN_POINT ( 'NONE',  ( 12.40954600831128296, 20.46600775631657854, -19.49970488155097215 ) ) ;
#24075 = ORIENTED_EDGE ( 'NONE', *, *, #20355, .T. ) ;
#24076 = CARTESIAN_POINT ( 'NONE',  ( -14.96161608456797687, 21.61429412723690291, 10.49999999999999822 ) ) ;
#24077 = VERTEX_POINT ( 'NONE', #31434 ) ;
#24079 = FACE_OUTER_BOUND ( 'NONE', #28316, .T. ) ;
#24078 = CARTESIAN_POINT ( 'NONE',  ( -11.40498260276712017, 18.50559946058070082, -23.84136616158568600 ) ) ;
#24080 = CARTESIAN_POINT ( 'NONE',  ( -10.28329067726930113, -19.14409761816654054, -23.84654465020906500 ) ) ;
#24081 = DIRECTION ( 'NONE',  ( 0.000000000000000000, 0.000000000000000000, -1.000000000000000000 ) ) ;
#24082 = AXIS2_PLACEMENT_3D ( 'NONE', #4720, #10615, #36007 ) ;
#24083 = CARTESIAN_POINT ( 'NONE',  ( -25.36562297843122238, -14.28257506075462047, -16.62385786568234636 ) ) ;
#24084 = CARTESIAN_POINT ( 'NONE',  ( -7.791008596474476633, -19.63400282832837362, -25.23920589239619261 ) ) ;
#24085 = DIRECTION ( 'NONE',  ( 0.000000000000000000, 0.000000000000000000, 1.000000000000000000 ) ) ;
#24086 = CARTESIAN_POINT ( 'NONE',  ( 11.84859450830439442, 16.77681853612139662, -28.74023605449830399 ) ) ;
#24087 = VERTEX_POINT ( 'NONE', #39974 ) ;
#24088 = CARTESIAN_POINT ( 'NONE',  ( 19.48206314129080141, 6.618909439000534967, -28.26876915201039964 ) ) ;
#24089 = VECTOR ( 'NONE', #22789, 1000.000000000000000 ) ;
#24090 = DIRECTION ( 'NONE',  ( 0.000000000000000000, 0.000000000000000000, 1.000000000000000000 ) ) ;
#24091 = DIRECTION ( 'NONE',  ( 0.000000000000000000, 0.000000000000000000, -1.000000000000000000 ) ) ;
#24092 = CARTESIAN_POINT ( 'NONE',  ( 1.828660225305861919, 9.087095699275852922, 10.50000000000000000 ) ) ;
#24093 = ORIENTED_EDGE ( 'NONE', *, *, #25970, .T. ) ;
#24094 = CARTESIAN_POINT ( 'NONE',  ( -20.64734822606397913, -0.1544862121781659936, -28.02694178585644735 ) ) ;
#24095 = CARTESIAN_POINT ( 'NONE',  ( 29.95060329414361533, -0.1183784304507303486, -9.698056910375742135 ) ) ;
#24096 = DIRECTION ( 'NONE',  ( -0.7431448254773862505, 0.6691306063588670083, 0.000000000000000000 ) ) ;
#24097 = CARTESIAN_POINT ( 'NONE',  ( 26.10558707266147493, -11.85287147006363462, 20.94377226548379056 ) ) ;
#24098 = CIRCLE ( 'NONE', #24728, 15.00000000000000000 ) ;
#24099 = CARTESIAN_POINT ( 'NONE',  ( 35.36940577612500647, -20.42053594592275800, -14.51648065752882566 ) ) ;
#24100 = CARTESIAN_POINT ( 'NONE',  ( 35.07402885326985142, -20.24999999999992184, 11.00000000000000000 ) ) ;
#24101 = VERTEX_POINT ( 'NONE', #12152 ) ;
#24102 = LINE ( 'NONE', #17827, #32064 ) ;
#24103 = CIRCLE ( 'NONE', #14363, 1.000000000000000000 ) ;
#24104 = DIRECTION ( 'NONE',  ( 1.000000000000000000, 0.000000000000000000, 0.000000000000000000 ) ) ;
#24105 = VERTEX_POINT ( 'NONE', #6247 ) ;
#24106 = CARTESIAN_POINT ( 'NONE',  ( 1.465318874961157203, 35.37165157456092857, -11.06833281905744570 ) ) ;
#24107 = CIRCLE ( 'NONE', #29212, 0.5000000000000002220 ) ;
#24108 = LINE ( 'NONE', #5425, #23718 ) ;
#24109 = FACE_OUTER_BOUND ( 'NONE', #12915, .T. ) ;
#24110 = DIRECTION ( 'NONE',  ( 1.000000000000000000, 0.000000000000000000, 0.000000000000000000 ) ) ;
#24111 = PLANE ( 'NONE',  #25776 ) ;
#24112 = DIRECTION ( 'NONE',  ( 0.000000000000000000, -0.000000000000000000, -1.000000000000000000 ) ) ;
#24113 = FACE_OUTER_BOUND ( 'NONE', #34834, .T. ) ;
#24114 = CARTESIAN_POINT ( 'NONE',  ( 14.38792334706498899, 28.09311145835767221, -8.686077744534234313 ) ) ;
#24115 = DIRECTION ( 'NONE',  ( -0.2185080122244104361, 0.6724985119639612652, -0.7071067811865437980 ) ) ;
#24116 = ORIENTED_EDGE ( 'NONE', *, *, #18557, .T. ) ;
#24118 = DIRECTION ( 'NONE',  ( -0.000000000000000000, -0.000000000000000000, 1.000000000000000000 ) ) ;
#24117 = CARTESIAN_POINT ( 'NONE',  ( -18.91572163234467041, 16.32661989365160338, -9.372685314759676700 ) ) ;
#24119 = CARTESIAN_POINT ( 'NONE',  ( -13.81877807188819851, 20.04207961888471345, 9.500000000000000000 ) ) ;
#24120 = CIRCLE ( 'NONE', #20884, 0.5000000000000004441 ) ;
#24121 = CARTESIAN_POINT ( 'NONE',  ( 15.30940322879717286, -26.50162545292337057, -7.357895834298116888 ) ) ;
#24122 = DIRECTION ( 'NONE',  ( 1.000000000000000000, 0.000000000000000000, 0.000000000000000000 ) ) ;
#24123 = CARTESIAN_POINT ( 'NONE',  ( 14.92592191758538434, 25.82844783702134350, -9.707335997509764169 ) ) ;
#24124 = ORIENTED_EDGE ( 'NONE', *, *, #39823, .T. ) ;
#24125 = LINE ( 'NONE', #36521, #25047 ) ;
#24126 = CARTESIAN_POINT ( 'NONE',  ( 16.58673509445612382, -31.15700704434060242, 11.00000000000000000 ) ) ;
#24127 = CARTESIAN_POINT ( 'NONE',  ( -16.46786645114412551, -12.86135933887615579, -27.00130938684783999 ) ) ;
#24128 = CARTESIAN_POINT ( 'NONE',  ( 3.891635163620496662, -24.39404397995950546, -9.874836895460536113 ) ) ;
#24129 = CARTESIAN_POINT ( 'NONE',  ( 11.28285220518144172, 17.35954613783441758, -27.46386206762080207 ) ) ;
#24130 = CARTESIAN_POINT ( 'NONE',  ( 20.72356761093054089, 11.55030529434603181, -12.89082050402462976 ) ) ;
#24131 = LINE ( 'NONE', #39167, #3700 ) ;
#24132 = CARTESIAN_POINT ( 'NONE',  ( -4.317981579255198987, 25.11931188802156711, -19.71681041348662333 ) ) ;
#24133 = ORIENTED_EDGE ( 'NONE', *, *, #31693, .T. ) ;
#24134 = APPLICATION_CONTEXT ( 'automotive_design' ) ;
#24135 = CARTESIAN_POINT ( 'NONE',  ( -23.01716326618291575, 13.28896540771138213, 12.73282698324853079 ) ) ;
#24136 = VERTEX_POINT ( 'NONE', #18847 ) ;
#24137 = CARTESIAN_POINT ( 'NONE',  ( -7.766013557953293400, 28.81973365084998306, 10.50000000000000000 ) ) ;
#24138 = ADVANCED_FACE ( 'NONE', ( #30841, #24542 ), #3007, .T. ) ;
#24139 = CARTESIAN_POINT ( 'NONE',  ( -5.100643064501314328, 15.70406341247269211, 12.00000000000000000 ) ) ;
#24140 = CARTESIAN_POINT ( 'NONE',  ( -25.13567556507226897, 0.5201041552294234371, -17.45255897844877069 ) ) ;
#24141 = CARTESIAN_POINT ( 'NONE',  ( 20.44673976918552327, -6.181689145942012686, -25.69967426495654905 ) ) ;
#24142 = EDGE_CURVE ( 'NONE', #39323, #659, #37533, .T. ) ;
#24143 = VERTEX_POINT ( 'NONE', #31045 ) ;
#24144 = CIRCLE ( 'NONE', #799, 0.5000000000000003331 ) ;
#24145 = DIRECTION ( 'NONE',  ( -1.000000000000000000, 0.000000000000000000, 0.000000000000000000 ) ) ;
#24146 = ORIENTED_EDGE ( 'NONE', *, *, #38192, .F. ) ;
#24147 = EDGE_CURVE ( 'NONE', #23843, #22927, #12739, .T. ) ;
#24148 = CARTESIAN_POINT ( 'NONE',  ( 13.28503138821879581, 15.53523575316139649, 7.000000000000000000 ) ) ;
#24149 = DIRECTION ( 'NONE',  ( -1.000000000000000000, 0.000000000000000000, 0.000000000000000000 ) ) ;
#24150 = CONICAL_SURFACE ( 'NONE', #23518, 1.000000000000007772, 0.7853981633974554954 ) ;
#24151 = PLANE ( 'NONE',  #39528 ) ;
#24152 = EDGE_LOOP ( 'NONE', ( #29542, #35751, #20512 ) ) ;
#24153 =( NAMED_UNIT ( * ) SI_UNIT ( $, .STERADIAN. ) SOLID_ANGLE_UNIT ( ) );
#24154 = CARTESIAN_POINT ( 'NONE',  ( -10.41268156625113228, 18.79179606750104981, 12.00000000000000000 ) ) ;
#24155 = CARTESIAN_POINT ( 'NONE',  ( -0.4999999999999950040, -6.123233995736694545E-17, 11.00000000000000000 ) ) ;
#24156 = LINE ( 'NONE', #1837, #17586 ) ;
#24157 = CARTESIAN_POINT ( 'NONE',  ( 26.90452307301082158, -22.05113920026022356, -11.10173837139930697 ) ) ;
#24158 = CARTESIAN_POINT ( 'NONE',  ( 17.72686569301070492, 14.07852954895453479, -17.97737483715281570 ) ) ;
#24159 = CARTESIAN_POINT ( 'NONE',  ( 7.566615708652627781, 19.25748430301096192, -27.88712974580454329 ) ) ;
#24160 = ORIENTED_EDGE ( 'NONE', *, *, #40144, .T. ) ;
#24161 = CARTESIAN_POINT ( 'NONE',  ( -19.21278935434771995, 9.517384517114377829, -22.24295473033291515 ) ) ;
#24162 = CARTESIAN_POINT ( 'NONE',  ( 8.412270287199559604, 10.07085245822950981, 10.50000000000000000 ) ) ;
#24163 = AXIS2_PLACEMENT_3D ( 'NONE', #36410, #8573, #33774 ) ;
#24164 = DIRECTION ( 'NONE',  ( -0.07391278520356926729, -0.7032331762534078656, -0.7071067811865435759 ) ) ;
#24165 = EDGE_CURVE ( 'NONE', #6733, #21617, #34948, .T. ) ;
#24166 = EDGE_CURVE ( 'NONE', #24961, #37999, #9708, .T. ) ;
#24167 = CARTESIAN_POINT ( 'NONE',  ( 14.83614609751987423, -25.15722166327546105, -11.56489435687942802 ) ) ;
#24168 = DIRECTION ( 'NONE',  ( 1.000000000000000000, 0.000000000000000000, 0.000000000000000000 ) ) ;
#24169 = CARTESIAN_POINT ( 'NONE',  ( -5.100643064501314328, 15.70406341247269211, 13.00000000000000178 ) ) ;
#24170 = CARTESIAN_POINT ( 'NONE',  ( -14.27227629280091215, 24.52115250329153540, -12.54634419364836262 ) ) ;
#24171 = CARTESIAN_POINT ( 'NONE',  ( -17.64560943446032937, -21.02421742741433164, -16.93458103129471226 ) ) ;
#24172 = CARTESIAN_POINT ( 'NONE',  ( 13.69821889811312410, -26.30560278297641830, -5.000000000000000000 ) ) ;
#24173 = AXIS2_PLACEMENT_3D ( 'NONE', #21349, #39627, #3257 ) ;
#24174 = LINE ( 'NONE', #36569, #21159 ) ;
#24175 = ORIENTED_EDGE ( 'NONE', *, *, #6937, .F. ) ;
#24176 = VERTEX_POINT ( 'NONE', #37732 ) ;
#24177 = CARTESIAN_POINT ( 'NONE',  ( -7.081591661052614839, 19.23835092891137322, -29.27181413004323929 ) ) ;
#24178 = DIRECTION ( 'NONE',  ( 0.000000000000000000, 0.000000000000000000, 1.000000000000000000 ) ) ;
#24179 = CARTESIAN_POINT ( 'NONE',  ( 10.54146960747273987, 17.40487552589537401, 12.00000000000000000 ) ) ;
#24180 = AXIS2_PLACEMENT_3D ( 'NONE', #13429, #18935, #3887 ) ;
#24181 = CARTESIAN_POINT ( 'NONE',  ( -9.038171950369942920, 10.91067434175333872, 10.96580508970281720 ) ) ;
#24182 = ORIENTED_EDGE ( 'NONE', *, *, #36830, .F. ) ;
#24183 = CARTESIAN_POINT ( 'NONE',  ( 29.75086405456110938, 0.1002501869623030895, -9.710278012872217701 ) ) ;
#24184 = DIRECTION ( 'NONE',  ( 0.000000000000000000, 0.000000000000000000, 1.000000000000000000 ) ) ;
#24185 = CARTESIAN_POINT ( 'NONE',  ( -2.564829916171942337, 8.028556778314829501, 10.96580508970281898 ) ) ;
#24186 = ORIENTED_EDGE ( 'NONE', *, *, #30238, .T. ) ;
#24187 = CARTESIAN_POINT ( 'NONE',  ( -25.85423149439973400, 0.3339084734886691441, -16.44513718936062929 ) ) ;
#24188 = EDGE_CURVE ( 'NONE', #36419, #11885, #28983, .T. ) ;
#24189 = CYLINDRICAL_SURFACE ( 'NONE', #35865, 1.000000000000000000 ) ;
#24190 = ORIENTED_EDGE ( 'NONE', *, *, #17618, .T. ) ;
#24191 = CARTESIAN_POINT ( 'NONE',  ( 25.82646452138326154, -3.017894876147785510, -18.05725647810044521 ) ) ;
#24192 = CARTESIAN_POINT ( 'NONE',  ( 36.42486030274157116, -16.61012894281671137, 13.32518128616598574 ) ) ;
#24193 = ORIENTED_EDGE ( 'NONE', *, *, #27520, .T. ) ;
#24194 = CARTESIAN_POINT ( 'NONE',  ( 13.15436037709940287, 33.66595454666934728, 14.53008259254018242 ) ) ;
#24195 = CARTESIAN_POINT ( 'NONE',  ( -5.799013854623373376, -17.87737810982027398, 20.50957957746029336 ) ) ;
#24196 = DIRECTION ( 'NONE',  ( 1.000000000000000000, 0.000000000000000000, 0.000000000000000000 ) ) ;
#24197 = CARTESIAN_POINT ( 'NONE',  ( -9.555312204553054301, 25.15592819202761632, 20.25080042701566541 ) ) ;
#24198 = VECTOR ( 'NONE', #26707, 1000.000000000000000 ) ;
#24199 = CARTESIAN_POINT ( 'NONE',  ( 0.000000000000000000, 22.50000000000000355, 13.00000000000000178 ) ) ;
#24200 = ORIENTED_EDGE ( 'NONE', *, *, #7144, .F. ) ;
#24201 = CARTESIAN_POINT ( 'NONE',  ( 14.31603901957230462, 19.98981538725070095, 9.500000000000000000 ) ) ;
#24202 = AXIS2_PLACEMENT_3D ( 'NONE', #34415, #39903, #2936 ) ;
#24203 = DIRECTION ( 'NONE',  ( 1.000000000000000000, 0.000000000000000000, 0.000000000000000000 ) ) ;
#24204 = CARTESIAN_POINT ( 'NONE',  ( 7.399002019425528154, 32.59854033243159677, -12.04523620305728393 ) ) ;
#24205 = AXIS2_PLACEMENT_3D ( 'NONE', #34742, #9762, #3460 ) ;
#24206 = CARTESIAN_POINT ( 'NONE',  ( 5.537946624086020009, 36.44027069998191593, 7.000000000000000000 ) ) ;
#24207 = CARTESIAN_POINT ( 'NONE',  ( 10.32009510687484521, 12.89643020664140316, 20.94377226548379411 ) ) ;
#24208 = ADVANCED_FACE ( 'NONE', ( #3995 ), #19851, .T. ) ;
#24209 = ADVANCED_FACE ( 'NONE', ( #22478 ), #20606, .T. ) ;
#24210 = CARTESIAN_POINT ( 'NONE',  ( 12.31336357260648562, -16.48320293064839959, -28.59255635963331699 ) ) ;
#24211 = CARTESIAN_POINT ( 'NONE',  ( 4.440908595777811385, 35.94977745735560859, 7.000000000000000000 ) ) ;
#24212 = FACE_BOUND ( 'NONE', #32795, .T. ) ;
#24213 = ORIENTED_EDGE ( 'NONE', *, *, #7121, .F. ) ;
#24214 = CIRCLE ( 'NONE', #38485, 6.000000000000000000 ) ;
#24215 = CARTESIAN_POINT ( 'NONE',  ( 15.26368502715787656, 26.62251295125168582, -7.355208640532818976 ) ) ;
#24216 = ORIENTED_EDGE ( 'NONE', *, *, #29670, .F. ) ;
#24217 = CARTESIAN_POINT ( 'NONE',  ( -12.79441350932495780, 20.84820608835214983, -18.47654784684910112 ) ) ;
#24218 = AXIS2_PLACEMENT_3D ( 'NONE', #37496, #5612, #34053 ) ;
#24219 = CARTESIAN_POINT ( 'NONE',  ( -18.99709059511109288, -25.05170461721374053, 18.42518152272145571 ) ) ;
#24220 = CARTESIAN_POINT ( 'NONE',  ( 10.48966746473434064, -19.58931170878575756, -22.74071033439049572 ) ) ;
#24221 = CARTESIAN_POINT ( 'NONE',  ( -3.607749162633398843, 7.931741834401822899, 10.49999999999999822 ) ) ;
#24222 = CARTESIAN_POINT ( 'NONE',  ( 14.07857810331197257, 23.82131834651897861, -13.51868220414109700 ) ) ;
#24223 = ORIENTED_EDGE ( 'NONE', *, *, #437, .F. ) ;
#24224 = CARTESIAN_POINT ( 'NONE',  ( 26.47194016310583820, -16.78111321318651861, -14.73213283222064796 ) ) ;
#24225 = ORIENTED_EDGE ( 'NONE', *, *, #12866, .F. ) ;
#24227 = CARTESIAN_POINT ( 'NONE',  ( 8.118377661053324701, 10.47536095541698486, 11.00000000000000000 ) ) ;
#24226 = CARTESIAN_POINT ( 'NONE',  ( -13.82211424505259778, 24.42565547601927634, -13.46747677272994004 ) ) ;
#24228 = CARTESIAN_POINT ( 'NONE',  ( -14.47914568234718224, -23.13007937158521088, -15.30831667679490415 ) ) ;
#24229 = CARTESIAN_POINT ( 'NONE',  ( -16.84920187510344647, 29.09530251743286300, -5.000000000000000000 ) ) ;
#24230 = AXIS2_PLACEMENT_3D ( 'NONE', #27411, #14828, #5673 ) ;
#24231 = ORIENTED_EDGE ( 'NONE', *, *, #26393, .T. ) ;
#24232 = CARTESIAN_POINT ( 'NONE',  ( -32.70405218813849757, -11.20998461038165495, -11.11490927511992410 ) ) ;
#24233 = CARTESIAN_POINT ( 'NONE',  ( -15.12763912169749858, -26.45704430479512936, -7.358536573642846967 ) ) ;
#24234 = CARTESIAN_POINT ( 'NONE',  ( -7.530592408761008549, 11.28437794979203623, 7.000000000000000000 ) ) ;
#24235 = EDGE_LOOP ( 'NONE', ( #37227, #17869, #28982, #30471, #25089, #29439, #24213 ) ) ;
#24236 = CARTESIAN_POINT ( 'NONE',  ( 20.62929968266412928, 3.093903264742920101, -26.39664856447400965 ) ) ;
#24237 = CARTESIAN_POINT ( 'NONE',  ( -8.412270287199731911, 10.07085245822962349, 10.49999999999999822 ) ) ;
#24238 = AXIS2_PLACEMENT_3D ( 'NONE', #4469, #10767, #25593 ) ;
#24239 = CARTESIAN_POINT ( 'NONE',  ( -18.77248997590657709, -31.35432035705730414, 11.00000000000000000 ) ) ;
#24240 = VERTEX_POINT ( 'NONE', #32240 ) ;
#24241 = CARTESIAN_POINT ( 'NONE',  ( -26.55369869109904357, 0.2031603616629021614, -15.44166204089604832 ) ) ;
#24242 = ADVANCED_FACE ( 'NONE', ( #6834 ), #10099, .F. ) ;
#24243 = VERTEX_POINT ( 'NONE', #38329 ) ;
#24244 = CARTESIAN_POINT ( 'NONE',  ( 21.82419164594113070, 0.07435039598037769537, -23.77433660182619946 ) ) ;
#24245 = AXIS2_PLACEMENT_3D ( 'NONE', #22737, #17274, #8104 ) ;
#24246 = CARTESIAN_POINT ( 'NONE',  ( 31.37624276535957435, -18.11508220673916014, 18.42518152272108622 ) ) ;
#24247 = EDGE_LOOP ( 'NONE', ( #3676, #18650, #35898, #22784 ) ) ;
#24248 = EDGE_CURVE ( 'NONE', #35146, #11442, #38125, .T. ) ;
#24249 = CARTESIAN_POINT ( 'NONE',  ( -27.21597387510395194, 2.648795058466725916, -10.72652230008515772 ) ) ;
#24250 = CARTESIAN_POINT ( 'NONE',  ( 0.000000000000000000, 22.50000000000000355, 11.00000000000000178 ) ) ;
#24251 = LINE ( 'NONE', #9212, #31036 ) ;
#24252 = CIRCLE ( 'NONE', #2194, 1.000000000000000000 ) ;
#24253 = CARTESIAN_POINT ( 'NONE',  ( -37.48524466415686618, -10.08537157645187499, 11.00000000000012967 ) ) ;
#24254 = FACE_OUTER_BOUND ( 'NONE', #31559, .T. ) ;
#24255 = AXIS2_PLACEMENT_3D ( 'NONE', #39747, #5430, #21266 ) ;
#24256 = FACE_BOUND ( 'NONE', #12039, .T. ) ;
#24257 = CARTESIAN_POINT ( 'NONE',  ( 11.44473057578109199, 31.45924896672603310, 11.00000000000000000 ) ) ;
#24258 = ORIENTED_EDGE ( 'NONE', *, *, #33022, .F. ) ;
#24259 = CARTESIAN_POINT ( 'NONE',  ( -24.20609638677606412, 8.035638068618503382, -5.480463713371170442 ) ) ;
#24260 = DIRECTION ( 'NONE',  ( 0.000000000000000000, 0.000000000000000000, 1.000000000000000000 ) ) ;
#24261 = CARTESIAN_POINT ( 'NONE',  ( 0.000000000000000000, 22.50000000000000355, 6.000000000000000000 ) ) ;
#24262 = CARTESIAN_POINT ( 'NONE',  ( 25.11666564602450791, -26.04266884310358421, -6.744201284302634214 ) ) ;
#24263 = ADVANCED_FACE ( 'NONE', ( #28581 ), #10500, .F. ) ;
#24264 = DIRECTION ( 'NONE',  ( -0.5877852522924800205, -0.8090169943749424553, -0.000000000000000000 ) ) ;
#24265 = EDGE_CURVE ( 'NONE', #32832, #7299, #40132, .T. ) ;
#24266 = CARTESIAN_POINT ( 'NONE',  ( 15.34186426957387184, 27.04214388478009923, -5.472936367007620539 ) ) ;
#24267 = CARTESIAN_POINT ( 'NONE',  ( 4.250808094710701366E-14, -26.77689918168226058, 11.55979286843934872 ) ) ;
#24268 = ORIENTED_EDGE ( 'NONE', *, *, #16613, .T. ) ;
#24269 = AXIS2_PLACEMENT_3D ( 'NONE', #14764, #26749, #20670 ) ;
#24270 = CARTESIAN_POINT ( 'NONE',  ( -13.90277657046047288, 15.06583648262319031, -29.40017519746768926 ) ) ;
#24271 = CARTESIAN_POINT ( 'NONE',  ( -23.10579450714032745, -17.79557859931359332, 20.82122704794065982 ) ) ;
#24272 = LINE ( 'NONE', #5974, #4891 ) ;
#24273 = CARTESIAN_POINT ( 'NONE',  ( 11.09010279485205963, 17.49098561682555442, -27.44912391568058041 ) ) ;
#24274 = VERTEX_POINT ( 'NONE', #19436 ) ;
#24275 = CYLINDRICAL_SURFACE ( 'NONE', #17698, 0.4999999999999995559 ) ;
#24276 = ORIENTED_EDGE ( 'NONE', *, *, #14626, .T. ) ;
#24278 = CARTESIAN_POINT ( 'NONE',  ( -7.126083911573537044, 10.99048532364579245, 10.50000000000000000 ) ) ;
#24277 = CARTESIAN_POINT ( 'NONE',  ( -10.90492496769149433, 17.35893878472046126, -29.99999999999998934 ) ) ;
#24279 = CARTESIAN_POINT ( 'NONE',  ( -10.24267276777706215, -19.15822127202351055, -23.85172878415961506 ) ) ;
#24280 = CARTESIAN_POINT ( 'NONE',  ( 9.004335565032041799, 10.95724613078621879, 10.99999999999999822 ) ) ;
#24281 = CARTESIAN_POINT ( 'NONE',  ( -26.74262847843787938, -14.00387254376185453, -15.68192966552173928 ) ) ;
#24282 = VECTOR ( 'NONE', #4420, 1000.000000000000000 ) ;
#24283 = CARTESIAN_POINT ( 'NONE',  ( -9.368301651731773205, -22.13363141439098314, -17.67998840172026576 ) ) ;
#24284 = LINE ( 'NONE', #3538, #7290 ) ;
#24285 = CARTESIAN_POINT ( 'NONE',  ( 14.37559196849546161, 21.13036632534599235, -15.57174267854623473 ) ) ;
#24286 = ORIENTED_EDGE ( 'NONE', *, *, #18791, .F. ) ;
#24287 = CARTESIAN_POINT ( 'NONE',  ( 22.56375456310565042, 6.182170930846935697, -16.85945526150993956 ) ) ;
#24288 = PLANE ( 'NONE',  #4399 ) ;
#24289 = DIRECTION ( 'NONE',  ( 1.000000000000000000, 0.000000000000000000, 0.000000000000000000 ) ) ;
#24290 = LINE ( 'NONE', #30791, #33604 ) ;
#24291 = ORIENTED_EDGE ( 'NONE', *, *, #1172, .T. ) ;
#24292 = CARTESIAN_POINT ( 'NONE',  ( -21.92138948956064581, -0.6339311634017230634, -23.68985892038928398 ) ) ;
#24293 = ADVANCED_FACE ( 'NONE', ( #10704 ), #13136, .T. ) ;
#24294 = AXIS2_PLACEMENT_3D ( 'NONE', #12620, #12418, #25008 ) ;
#24295 = CARTESIAN_POINT ( 'NONE',  ( 20.48413544616686011, 0.8063757131868728445, -30.00000000000000000 ) ) ;
#24296 = DIRECTION ( 'NONE',  ( 0.000000000000000000, 0.000000000000000000, 1.000000000000000000 ) ) ;
#24297 = EDGE_CURVE ( 'NONE', #38258, #28430, #3794, .T. ) ;
#24298 = CARTESIAN_POINT ( 'NONE',  ( 25.98021325959767225, -4.875178728622389102, 20.50957957746029336 ) ) ;
#24299 = CARTESIAN_POINT ( 'NONE',  ( 12.05832241004688399, 18.99596958976722760, -21.04195414767209726 ) ) ;
#24300 = DIRECTION ( 'NONE',  ( 1.000000000000000000, 0.000000000000000000, 0.000000000000000000 ) ) ;
#24301 = CIRCLE ( 'NONE', #34077, 1.000000000000000000 ) ;
#24302 = ADVANCED_FACE ( 'NONE', ( #17008 ), #34664, .F. ) ;
#24303 = ORIENTED_EDGE ( 'NONE', *, *, #16154, .F. ) ;
#24304 = CARTESIAN_POINT ( 'NONE',  ( -8.007761790012255076, 9.776959832083379709, 7.000000000000000000 ) ) ;
#24305 = DIRECTION ( 'NONE',  ( -1.000000000000000000, 0.000000000000000000, 0.000000000000000000 ) ) ;
#24306 = DIRECTION ( 'NONE',  ( 1.000000000000000000, 0.000000000000000000, 0.000000000000000000 ) ) ;
#24307 = CARTESIAN_POINT ( 'NONE',  ( 3.860467995676855502, 37.87601681638416551, -6.280638966725057948 ) ) ;
#24308 = DIRECTION ( 'NONE',  ( 0.2079116908177663092, 0.9781476007338041345, -0.000000000000000000 ) ) ;
#24309 = DIRECTION ( 'NONE',  ( 0.8090169943749425663, -0.5877852522924797984, 0.000000000000000000 ) ) ;
#24310 = DIRECTION ( 'NONE',  ( -0.000000000000000000, -0.000000000000000000, -1.000000000000000000 ) ) ;
#24311 = EDGE_CURVE ( 'NONE', #36470, #7488, #23701, .T. ) ;
#24312 = CYLINDRICAL_SURFACE ( 'NONE', #21232, 1.000000000000000888 ) ;
#24313 = CARTESIAN_POINT ( 'NONE',  ( 10.44103466624280685, 32.57396620494213124, 7.000000000000000000 ) ) ;
#24314 = DIRECTION ( 'NONE',  ( -0.000000000000000000, -0.000000000000000000, -1.000000000000000000 ) ) ;
#24315 = ADVANCED_FACE ( 'NONE', ( #29996 ), #8257, .F. ) ;
#24316 = CIRCLE ( 'NONE', #39220, 1.000000000000007772 ) ;
#24317 = CARTESIAN_POINT ( 'NONE',  ( 14.90467518106525269, 28.31725849260483585, -4.999999999999998224 ) ) ;
#24318 = CARTESIAN_POINT ( 'NONE',  ( -10.78894649379783388, 21.72623886970244911, 13.00000000000000178 ) ) ;
#24319 = EDGE_LOOP ( 'NONE', ( #27124, #32219, #34638, #13664 ) ) ;
#24321 = PLANE ( 'NONE',  #29137 ) ;
#24320 = CARTESIAN_POINT ( 'NONE',  ( -17.38933059521489710, 14.62580955216105849, -17.95874418599646560 ) ) ;
#24322 = CARTESIAN_POINT ( 'NONE',  ( 16.00000000000000000, 22.50000000000000355, 13.00000000000000178 ) ) ;
#24323 = CARTESIAN_POINT ( 'NONE',  ( 13.02171807787146385, -23.09221996238842323, -15.44989160518525928 ) ) ;
#24324 = CARTESIAN_POINT ( 'NONE',  ( -13.76749719093327329, -17.52493337752909142, -23.41495867390861818 ) ) ;
#24325 = DIRECTION ( 'NONE',  ( 1.000000000000000000, 0.000000000000000000, 0.000000000000000000 ) ) ;
#24326 = CARTESIAN_POINT ( 'NONE',  ( 11.45955615606448319, 18.45868997252334864, -23.85003837067463550 ) ) ;
#24327 = ORIENTED_EDGE ( 'NONE', *, *, #30446, .T. ) ;
#24328 = VECTOR ( 'NONE', #20428, 1000.000000000000227 ) ;
#24329 = DIRECTION ( 'NONE',  ( -0.1470157664651938756, 0.6916548014802249567, 0.7071067811865492381 ) ) ;
#24330 = CARTESIAN_POINT ( 'NONE',  ( 3.992867117591230031, 8.524771480177552263, 9.500000000000000000 ) ) ;
#24331 = CIRCLE ( 'NONE', #10725, 0.5000000000000007772 ) ;
#24332 = CARTESIAN_POINT ( 'NONE',  ( -23.53733200146751869, -18.44805065072479877, -15.72207550959232947 ) ) ;
#24333 = CARTESIAN_POINT ( 'NONE',  ( -0.2650373451695003379, -20.49916026595607121, -30.00000000000000711 ) ) ;
#24334 = CARTESIAN_POINT ( 'NONE',  ( 14.92415143525127341, 24.85911683587750787, -10.66521362572363785 ) ) ;
#24335 = CARTESIAN_POINT ( 'NONE',  ( 22.21982769557913784, 11.10346373912405049, -4.999999999999997335 ) ) ;
#24336 = CYLINDRICAL_SURFACE ( 'NONE', #38765, 1.000000000000000000 ) ;
#24337 = CARTESIAN_POINT ( 'NONE',  ( -4.208561989267932901, 37.92874393496560970, -5.858868913340946172 ) ) ;
#24338 = ORIENTED_EDGE ( 'NONE', *, *, #12294, .T. ) ;
#24339 = CARTESIAN_POINT ( 'NONE',  ( -33.77851027019138286, -5.369403031741126320, -8.110867528180607522 ) ) ;
#24340 = CARTESIAN_POINT ( 'NONE',  ( -20.35904855840124128, 17.61891361913183474, 13.32518128616461084 ) ) ;
#24341 = EDGE_LOOP ( 'NONE', ( #1817, #2376, #4343 ) ) ;
#24342 = EDGE_CURVE ( 'NONE', #35146, #10152, #36099, .T. ) ;
#24343 = CARTESIAN_POINT ( 'NONE',  ( 1.974196316410860241, 7.629928981499271679, 7.202682876670048806 ) ) ;
#24344 = PLANE ( 'NONE',  #29073 ) ;
#24345 = CARTESIAN_POINT ( 'NONE',  ( -21.68533774883767862, 0.8527267334164467805, -23.86863619998306518 ) ) ;
#24346 = CARTESIAN_POINT ( 'NONE',  ( 34.54137992947591584, -13.89200096410145768, -7.989112350646218275 ) ) ;
#24347 = VECTOR ( 'NONE', #26625, 1000.000000000000000 ) ;
#24348 = ORIENTED_EDGE ( 'NONE', *, *, #33340, .T. ) ;
#24349 = DIRECTION ( 'NONE',  ( -0.000000000000000000, -0.000000000000000000, -1.000000000000000000 ) ) ;
#24350 = ORIENTED_EDGE ( 'NONE', *, *, #19552, .F. ) ;
#24351 = DIRECTION ( 'NONE',  ( -0.000000000000000000, -0.000000000000000000, -1.000000000000000000 ) ) ;
#24352 = AXIS2_PLACEMENT_3D ( 'NONE', #17596, #29965, #36275 ) ;
#24353 = CARTESIAN_POINT ( 'NONE',  ( -1.000000000000000000, 37.50000000000000711, 7.000000000000000000 ) ) ;
#24354 = AXIS2_PLACEMENT_3D ( 'NONE', #39293, #15114, #18171 ) ;
#24355 = VECTOR ( 'NONE', #33396, 1000.000000000000000 ) ;
#24356 = DIRECTION ( 'NONE',  ( 0.000000000000000000, 0.000000000000000000, 1.000000000000000000 ) ) ;
#24357 = ORIENTED_EDGE ( 'NONE', *, *, #8197, .F. ) ;
#24358 = CARTESIAN_POINT ( 'NONE',  ( 8.100578861132810005, 28.44816123811117592, 10.50000000000000178 ) ) ;
#24359 = DIRECTION ( 'NONE',  ( 0.6691306063588561281, -0.7431448254773961315, 0.000000000000000000 ) ) ;
#24360 = CARTESIAN_POINT ( 'NONE',  ( 3.831426523743819423, 25.75866349410729939, 22.99999999999999289 ) ) ;
#24361 = CARTESIAN_POINT ( 'NONE',  ( 30.18422347142476880, -23.20414393450525736, -5.000000000000001776 ) ) ;
#24362 = CARTESIAN_POINT ( 'NONE',  ( 19.54635772746084399, 15.94078878846792335, -5.481359321442739407 ) ) ;
#24363 = CARTESIAN_POINT ( 'NONE',  ( 7.501377273760488684, 19.07882637373012713, -29.27881224950820283 ) ) ;
#24364 = EDGE_LOOP ( 'NONE', ( #6180, #8411, #36036, #23008 ) ) ;
#24365 = CARTESIAN_POINT ( 'NONE',  ( -21.95856242959800042, 10.64870207983313577, -9.886801507649353837 ) ) ;
#24366 = CARTESIAN_POINT ( 'NONE',  ( -4.476907992048016816, 18.63850621467409496, 6.000000000000000000 ) ) ;
#24367 = CARTESIAN_POINT ( 'NONE',  ( 15.05947082473196197, -25.87448528531247760, -9.699063484119998080 ) ) ;
#24368 = DIRECTION ( 'NONE',  ( -0.4067366430757884399, 0.9135454576426061957, 0.000000000000000000 ) ) ;
#24369 = EDGE_CURVE ( 'NONE', #32508, #20904, #20694, .T. ) ;
#24370 = CARTESIAN_POINT ( 'NONE',  ( 23.06249103411542478, 13.31513540672987972, -4.999999999999992006 ) ) ;
#24371 = B_SPLINE_CURVE_WITH_KNOTS ( 'NONE', 3,
 ( #16677, #29058, #38400, #15520, #10575, #22958 ),
 .UNSPECIFIED., .F., .F.,
 ( 4, 2, 4 ),
 ( 0.000000000000000000, 0.5000000000000000000, 1.000000000000000000 ),
 .UNSPECIFIED. ) ;
#24372 = CARTESIAN_POINT ( 'NONE',  ( -11.01071465375284752, 17.44424455191658296, -28.07566285216567081 ) ) ;
#24373 = CARTESIAN_POINT ( 'NONE',  ( -15.32667431977992578, -18.29772241814856670, -21.07163874326107589 ) ) ;
#24374 = CARTESIAN_POINT ( 'NONE',  ( 8.268557591513960858, -18.75831942629880444, -30.00000000000000000 ) ) ;
#24375 = PLANE ( 'NONE',  #3009 ) ;
#24376 = EDGE_LOOP ( 'NONE', ( #33441, #17466, #10552, #33856 ) ) ;
#24377 = ORIENTED_EDGE ( 'NONE', *, *, #40127, .F. ) ;
#24378 = CARTESIAN_POINT ( 'NONE',  ( -8.856483827409315168, 29.59330869415324372, -13.96223684641979901 ) ) ;
#24379 = AXIS2_PLACEMENT_3D ( 'NONE', #19162, #22204, #13262 ) ;
#24380 = DIRECTION ( 'NONE',  ( -1.000000000000000000, 0.000000000000000000, 0.000000000000000000 ) ) ;
#24381 = DIRECTION ( 'NONE',  ( 1.000000000000000000, 0.000000000000000000, 0.000000000000000000 ) ) ;
#24382 = AXIS2_PLACEMENT_3D ( 'NONE', #10724, #38754, #32261 ) ;
#24383 = VECTOR ( 'NONE', #20331, 1000.000000000000114 ) ;
#24384 = DIRECTION ( 'NONE',  ( -0.000000000000000000, -0.000000000000000000, -1.000000000000000000 ) ) ;
#24385 = ORIENTED_EDGE ( 'NONE', *, *, #8372, .F. ) ;
#24386 = CARTESIAN_POINT ( 'NONE',  ( 23.93473260754475618, 0.4999434715730360357, -19.49809802192611841 ) ) ;
#24387 = DIRECTION ( 'NONE',  ( -0.8090169943749504489, -0.5877852522924690293, 0.000000000000000000 ) ) ;
#24388 = LINE ( 'NONE', #36781, #32302 ) ;
#24389 = ORIENTED_EDGE ( 'NONE', *, *, #25141, .F. ) ;
#24390 = CARTESIAN_POINT ( 'NONE',  ( -30.85287573504917802, -0.02542951706361920583, -5.946081676602823940 ) ) ;
#24391 = LINE ( 'NONE', #2859, #20931 ) ;
#24392 = ORIENTED_EDGE ( 'NONE', *, *, #4068, .F. ) ;
#24393 = CARTESIAN_POINT ( 'NONE',  ( 32.36939943392307129, -4.852295849567697772, -10.37643807136409890 ) ) ;
#24394 = ORIENTED_EDGE ( 'NONE', *, *, #13824, .T. ) ;
#24395 = CARTESIAN_POINT ( 'NONE',  ( 9.237168799396084040, 37.83823547837376111, 12.73282698324857520 ) ) ;
#24396 = ADVANCED_FACE ( 'NONE', ( #39734 ), #23900, .F. ) ;
#24397 = CARTESIAN_POINT ( 'NONE',  ( -17.62780868050356986, -18.45076755199228202, 20.82122704794079837 ) ) ;
#24398 = DIRECTION ( 'NONE',  ( -0.5877852522924691403, 0.8090169943749503378, 0.000000000000000000 ) ) ;
#24399 = CARTESIAN_POINT ( 'NONE',  ( -3.838817179443412275, 30.80979998870936498, 20.50957957746028981 ) ) ;
#24400 = DIRECTION ( 'NONE',  ( -0.1045284632676570929, -0.9945218953682730678, 0.000000000000000000 ) ) ;
#24401 = ORIENTED_EDGE ( 'NONE', *, *, #24863, .T. ) ;
#24402 = DIRECTION ( 'NONE',  ( 0.000000000000000000, 0.000000000000000000, -1.000000000000000000 ) ) ;
#24403 = FACE_OUTER_BOUND ( 'NONE', #31385, .T. ) ;
#24404 = AXIS2_PLACEMENT_3D ( 'NONE', #13825, #1440, #17298 ) ;
#24405 = CARTESIAN_POINT ( 'NONE',  ( 3.293556582578045067, 20.32739358238259442, -28.46901180915632779 ) ) ;
#24406 = VECTOR ( 'NONE', #15930, 1000.000000000000000 ) ;
#24407 = DIRECTION ( 'NONE',  ( 0.9781476007338036904, -0.2079116908177681133, 0.000000000000000000 ) ) ;
#24408 = DIRECTION ( 'NONE',  ( 1.000000000000000000, 0.000000000000000000, 0.000000000000000000 ) ) ;
#24409 = VECTOR ( 'NONE', #31212, 1000.000000000000114 ) ;
#24410 = EDGE_CURVE ( 'NONE', #37413, #12011, #20666, .T. ) ;
#24411 = CARTESIAN_POINT ( 'NONE',  ( 12.13886791120663489, -18.39813430154476492, -23.60940752486453675 ) ) ;
#24412 = FACE_OUTER_BOUND ( 'NONE', #4786, .T. ) ;
#24413 = CARTESIAN_POINT ( 'NONE',  ( -9.677076426724111613, 26.69573495723220091, 11.00000000000000000 ) ) ;
#24414 = CARTESIAN_POINT ( 'NONE',  ( 0.01803229776516698107, 30.37627742347970283, 13.00000000000000178 ) ) ;
#24415 = ORIENTED_EDGE ( 'NONE', *, *, #6638, .T. ) ;
#24416 = VERTEX_POINT ( 'NONE', #11911 ) ;
#24417 = CARTESIAN_POINT ( 'NONE',  ( -11.14607843802444087, 17.59829798962171310, -26.83237680307435369 ) ) ;
#24418 = CARTESIAN_POINT ( 'NONE',  ( -30.63324413334818885, -19.40199358733788415, 18.42518152272070964 ) ) ;
#24419 = CARTESIAN_POINT ( 'NONE',  ( 14.64890392409851572, -25.63402876358651383, -10.18232085067979220 ) ) ;
#24420 = EDGE_CURVE ( 'NONE', #27849, #24787, #36167, .T. ) ;
#24421 = CARTESIAN_POINT ( 'NONE',  ( 6.064564986133971658, 13.54338174056915456, 6.000000000000000000 ) ) ;
#24422 = ADVANCED_FACE ( 'NONE', ( #33064 ), #29694, .T. ) ;
#24423 = VERTEX_POINT ( 'NONE', #27150 ) ;
#24424 = ORIENTED_EDGE ( 'NONE', *, *, #31159, .F. ) ;
#24426 = FACE_OUTER_BOUND ( 'NONE', #9461, .T. ) ;
#24425 = CARTESIAN_POINT ( 'NONE',  ( -13.39899704888391518, 25.36066129426254534, -13.38256906110033029 ) ) ;
#24427 = CARTESIAN_POINT ( 'NONE',  ( -11.14796620122417536, -17.40538162519350252, -27.98683963314264034 ) ) ;
#24428 = DIRECTION ( 'NONE',  ( 1.000000000000000000, 0.000000000000000000, 0.000000000000000000 ) ) ;
#24429 = ORIENTED_EDGE ( 'NONE', *, *, #5443, .F. ) ;
#24430 = CARTESIAN_POINT ( 'NONE',  ( -34.29392370955937963, -11.77843072186552220, -8.881902778450617930 ) ) ;
#24431 = CARTESIAN_POINT ( 'NONE',  ( -14.04164913135559978, -25.01591397610629031, -11.60796646869975390 ) ) ;
#24432 = CARTESIAN_POINT ( 'NONE',  ( 14.06524961900339399, 27.71236540882591015, 7.500000000000000888 ) ) ;
#24433 = EDGE_LOOP ( 'NONE', ( #28458, #32438 ) ) ;
#24434 = CARTESIAN_POINT ( 'NONE',  ( 21.24802458993929832, 0.9742268056361320649, -25.03556984149153308 ) ) ;
#24435 = CARTESIAN_POINT ( 'NONE',  ( -8.593266739736662885, 16.38397459621564067, 10.50000000000000000 ) ) ;
#24436 = FACE_OUTER_BOUND ( 'NONE', #38775, .T. ) ;
#24437 = ORIENTED_EDGE ( 'NONE', *, *, #31962, .F. ) ;
#24438 = CARTESIAN_POINT ( 'NONE',  ( -28.97168722745774261, 0.006711083214636500045, -11.59031396894388699 ) ) ;
#24439 = ORIENTED_EDGE ( 'NONE', *, *, #370, .F. ) ;
#24440 = CARTESIAN_POINT ( 'NONE',  ( 24.20991175986098654, -0.1716401066519940843, -19.40784505169473206 ) ) ;
#24441 = AXIS2_PLACEMENT_3D ( 'NONE', #27078, #26676, #11242 ) ;
#24442 = CARTESIAN_POINT ( 'NONE',  ( 28.97703757779505551, -22.02226062111144955, 17.92354375535251165 ) ) ;
#24443 = ADVANCED_FACE ( 'NONE', ( #11115 ), #8055, .F. ) ;
#24444 = VERTEX_POINT ( 'NONE', #11712 ) ;
#24445 = CARTESIAN_POINT ( 'NONE',  ( -20.46803965419261218, 2.897456671940229711, -27.56527374437133204 ) ) ;
#24446 = ADVANCED_FACE ( 'NONE', ( #12697 ), #21250, .T. ) ;
#24447 = LINE ( 'NONE', #24052, #36493 ) ;
#24448 = DIRECTION ( 'NONE',  ( 0.000000000000000000, 0.000000000000000000, 1.000000000000000000 ) ) ;
#24449 = DIRECTION ( 'NONE',  ( -1.000000000000000000, 0.000000000000000000, 0.000000000000000000 ) ) ;
#24450 = CARTESIAN_POINT ( 'NONE',  ( -8.935776944912362296, 22.65328985282726393, 12.00000000000000000 ) ) ;
#24451 = CARTESIAN_POINT ( 'NONE',  ( 5.767236651883443699, 13.71142893291679421, 10.00000000000000000 ) ) ;
#24452 = FACE_OUTER_BOUND ( 'NONE', #27001, .T. ) ;
#24453 = ORIENTED_EDGE ( 'NONE', *, *, #37444, .T. ) ;
#24454 = CARTESIAN_POINT ( 'NONE',  ( -19.71604245095232955, 5.704143033173037836, -28.82764346654152732 ) ) ;
#24455 = CARTESIAN_POINT ( 'NONE',  ( 7.096882951594524869, 29.56287847632726695, 10.49999999999999467 ) ) ;
#24456 = LINE ( 'NONE', #33817, #5815 ) ;
#24457 = CARTESIAN_POINT ( 'NONE',  ( 22.12641700133371359, -25.78554156883743431, -9.427553252327385280 ) ) ;
#24458 = CARTESIAN_POINT ( 'NONE',  ( -12.67417846324126174, 14.47720745114824226, 7.000000000000000000 ) ) ;
#24459 = EDGE_CURVE ( 'NONE', #8130, #2159, #8298, .T. ) ;
#24460 = CARTESIAN_POINT ( 'NONE',  ( 13.65407654052588526, 23.65245025108414367, -14.44949798609442126 ) ) ;
#24461 = VECTOR ( 'NONE', #11308, 1000.000000000000000 ) ;
#24462 = CARTESIAN_POINT ( 'NONE',  ( 15.12590024503359842, -28.14827041158748244, 13.92931973827808534 ) ) ;
#24463 = ORIENTED_EDGE ( 'NONE', *, *, #34955, .F. ) ;
#24464 = CARTESIAN_POINT ( 'NONE',  ( -16.20952767024093077, 24.08095879529154004, -5.947967261773682957 ) ) ;
#24465 = CARTESIAN_POINT ( 'NONE',  ( -22.70288158165621084, -17.06695585772259705, 20.94377226548368753 ) ) ;
#24466 = DIRECTION ( 'NONE',  ( -1.000000000000000000, 0.000000000000000000, 0.000000000000000000 ) ) ;
#24467 = CARTESIAN_POINT ( 'NONE',  ( 11.09448639774211287, 17.48802892231923778, -27.44946313874878996 ) ) ;
#24468 = EDGE_LOOP ( 'NONE', ( #5847, #37268, #24424, #31924 ) ) ;
#24469 = DIRECTION ( 'NONE',  ( 0.000000000000000000, 0.000000000000000000, 1.000000000000000000 ) ) ;
#24470 = EDGE_LOOP ( 'NONE', ( #32032, #13926 ) ) ;
#24471 = AXIS2_PLACEMENT_3D ( 'NONE', #23344, #18057, #26990 ) ;
#24473 = CARTESIAN_POINT ( 'NONE',  ( -5.440908595777636414, 35.94977745735568675, 7.000000000000000000 ) ) ;
#24472 = CARTESIAN_POINT ( 'NONE',  ( -12.87226721047317035, 21.74635154274772120, -17.42485855766595648 ) ) ;
#24474 = CARTESIAN_POINT ( 'NONE',  ( -12.44633464221259622, -22.01977715156473536, -17.41908692410127912 ) ) ;
#24475 = CARTESIAN_POINT ( 'NONE',  ( -0.4999999999999991673, 33.00000000000000000, 11.00000000000000000 ) ) ;
#24476 = VECTOR ( 'NONE', #25104, 1000.000000000000227 ) ;
#24477 = CARTESIAN_POINT ( 'NONE',  ( -32.42739033151597283, -18.25660761601222148, -8.842418814747594169 ) ) ;
#24478 = CARTESIAN_POINT ( 'NONE',  ( -11.50551555847164664, -25.70084177611234466, -6.898850981578088515 ) ) ;
#24479 = CARTESIAN_POINT ( 'NONE',  ( -14.97277451176450924, 21.48159783397892397, 10.49999999999999822 ) ) ;
#24480 = CARTESIAN_POINT ( 'NONE',  ( 16.11351922548164950, 24.44051152376729519, -5.474194937227850666 ) ) ;
#24481 = ORIENTED_EDGE ( 'NONE', *, *, #30913, .T. ) ;
#24482 = CARTESIAN_POINT ( 'NONE',  ( 20.28232154407063348, 6.728145097213812598, -23.24529083297425558 ) ) ;
#24483 = DIRECTION ( 'NONE',  ( 0.8090169943749504489, 0.5877852522924690293, -0.000000000000000000 ) ) ;
#24484 = CARTESIAN_POINT ( 'NONE',  ( 18.72723793738837372, -3.339582153676996512, 23.00000000000000000 ) ) ;
#24485 = CARTESIAN_POINT ( 'NONE',  ( -12.30736835487442704, 14.81698729810789672, 9.000000000000001776 ) ) ;
#24486 = ORIENTED_EDGE ( 'NONE', *, *, #24789, .T. ) ;
#24487 = CARTESIAN_POINT ( 'NONE',  ( -21.88088975564236449, -0.2942360282749391653, -23.72980161136129240 ) ) ;
#24488 = CARTESIAN_POINT ( 'NONE',  ( 25.24508218390874603, 0.3179225735388317431, -17.43064974027972980 ) ) ;
#24489 = FACE_OUTER_BOUND ( 'NONE', #33822, .T. ) ;
#24490 = CARTESIAN_POINT ( 'NONE',  ( 25.35679574134477932, -6.615406304682780458, 20.82122704794150181 ) ) ;
#24491 = DIRECTION ( 'NONE',  ( -0.8090169943749505599, -0.5877852522924689183, 0.000000000000000000 ) ) ;
#24492 = EDGE_CURVE ( 'NONE', #20144, #3653, #18020, .T. ) ;
#24493 = LINE ( 'NONE', #27546, #7613 ) ;
#24494 = VECTOR ( 'NONE', #15894, 999.9999999999997726 ) ;
#24495 = CIRCLE ( 'NONE', #16083, 1.000000000000000888 ) ;
#24496 = ORIENTED_EDGE ( 'NONE', *, *, #29099, .T. ) ;
#24497 = LINE ( 'NONE', #11915, #14559 ) ;
#24498 = VECTOR ( 'NONE', #38284, 999.9999999999998863 ) ;
#24499 = CIRCLE ( 'NONE', #15429, 6.000000000000001776 ) ;
#24500 = DIRECTION ( 'NONE',  ( -0.1470157664651888241, 0.6916548014802291755, -0.7071067811865460184 ) ) ;
#24501 = CARTESIAN_POINT ( 'NONE',  ( -10.18324708981896087, 16.78440424842446532, 6.000000000000000000 ) ) ;
#24502 = CARTESIAN_POINT ( 'NONE',  ( 3.060806728840579805, 29.89625055151331168, -15.70096931457847234 ) ) ;
#24503 = CARTESIAN_POINT ( 'NONE',  ( -5.383930013064101239, 36.46347792550319866, 10.49999999999999822 ) ) ;
#24504 = CARTESIAN_POINT ( 'NONE',  ( 14.86556419889026337, 20.43481210330100595, 10.49999999999999289 ) ) ;
#24505 = DIRECTION ( 'NONE',  ( 1.000000000000000000, 6.938893903907210234E-15, 0.000000000000000000 ) ) ;
#24506 = CARTESIAN_POINT ( 'NONE',  ( 6.404490139165913476, 34.42612703509930583, 9.500000000000000000 ) ) ;
#24507 = CARTESIAN_POINT ( 'NONE',  ( 7.064564986133971658, 13.54338174056915456, 6.000000000000000000 ) ) ;
#24508 = EDGE_CURVE ( 'NONE', #6906, #24961, #12178, .T. ) ;
#24509 = DIRECTION ( 'NONE',  ( 0.000000000000000000, 0.000000000000000000, 1.000000000000000000 ) ) ;
#24510 = CARTESIAN_POINT ( 'NONE',  ( 13.56443329977971857, 24.98013321944925735, -13.41769806874402171 ) ) ;
#24511 = CARTESIAN_POINT ( 'NONE',  ( 9.529746168869746015, 10.91601215036168959, 7.382773698552464126 ) ) ;
#24512 = VERTEX_POINT ( 'NONE', #33662 ) ;
#24514 = CARTESIAN_POINT ( 'NONE',  ( 14.47283171447379502, 21.48159823030310989, 9.500000000000000000 ) ) ;
#24513 = CARTESIAN_POINT ( 'NONE',  ( -16.42692940787602751, 16.16190383186714996, -17.88839106487290209 ) ) ;
#24515 = CARTESIAN_POINT ( 'NONE',  ( 10.70158575030369796, 30.79011836036717753, 9.500000000000000000 ) ) ;
#24516 = EDGE_CURVE ( 'NONE', #22721, #34828, #30021, .T. ) ;
#24517 = CARTESIAN_POINT ( 'NONE',  ( 13.03491049794189216, -23.09316184486432277, -15.44851748533687008 ) ) ;
#24518 = CARTESIAN_POINT ( 'NONE',  ( -16.05099854162948603, -21.51520587089331471, -17.05908743538380890 ) ) ;
#24519 = FACE_OUTER_BOUND ( 'NONE', #10965, .T. ) ;
#24520 = CARTESIAN_POINT ( 'NONE',  ( 14.52648563089041645, 24.98748751028934834, -11.59782509437098419 ) ) ;
#24521 = VECTOR ( 'NONE', #25009, 1000.000000000000227 ) ;
#24522 = ORIENTED_EDGE ( 'NONE', *, *, #7144, .T. ) ;
#24523 = CARTESIAN_POINT ( 'NONE',  ( -4.000124606132347438, 8.490627681068769306, 10.49999999999999822 ) ) ;
#24524 = CARTESIAN_POINT ( 'NONE',  ( 14.48927117870123027, -30.61587158504688233, 11.00000000000000000 ) ) ;
#24525 = CARTESIAN_POINT ( 'NONE',  ( -26.12394372346507865, -27.06777822797208088, 14.53008259254010959 ) ) ;
#24526 = CIRCLE ( 'NONE', #20618, 22.50000000000000355 ) ;
#24527 = CIRCLE ( 'NONE', #6987, 1.000000000000000888 ) ;
#24528 = EDGE_CURVE ( 'NONE', #888, #21822, #24493, .T. ) ;
#24529 = CARTESIAN_POINT ( 'NONE',  ( -29.02322137993849438, -24.14915179229603837, -5.438517818996884579 ) ) ;
#24530 = CARTESIAN_POINT ( 'NONE',  ( -0.2994915553838167210, -21.65328977690111145, -21.17874425746205702 ) ) ;
#24531 = CARTESIAN_POINT ( 'NONE',  ( 13.49234167325138145, 21.73580331833325019, -16.48722854393279391 ) ) ;
#24532 = CARTESIAN_POINT ( 'NONE',  ( 20.40580192547206551, 12.55472529160778983, -11.88336945610312689 ) ) ;
#24533 = CYLINDRICAL_SURFACE ( 'NONE', #9567, 1.000000000000000888 ) ;
#24534 = B_SPLINE_CURVE_WITH_KNOTS ( 'NONE', 3,
 ( #2005, #20888, #11139, #20489 ),
 .UNSPECIFIED., .F., .F.,
 ( 4, 4 ),
 ( 0.000000000000000000, 0.06666641432897602026 ),
 .UNSPECIFIED. ) ;
#24535 = CARTESIAN_POINT ( 'NONE',  ( -5.286117828675410024, 37.24231109432135867, -7.131154415093411636 ) ) ;
#24536 = VECTOR ( 'NONE', #23252, 1000.000000000000000 ) ;
#24537 = ORIENTED_EDGE ( 'NONE', *, *, #38029, .F. ) ;
#24538 = CARTESIAN_POINT ( 'NONE',  ( -28.89557855833852074, -5.358265633141725992, -14.97716460387147919 ) ) ;
#24539 = AXIS2_PLACEMENT_3D ( 'NONE', #30494, #605, #22327 ) ;
#24540 = CARTESIAN_POINT ( 'NONE',  ( -28.79337657216479585, 4.963436916928034570, 11.00000000000544276 ) ) ;
#24541 = EDGE_LOOP ( 'NONE', ( #13991, #5987, #18663, #23236 ) ) ;
#24542 = FACE_OUTER_BOUND ( 'NONE', #22879, .T. ) ;
#24543 = CARTESIAN_POINT ( 'NONE',  ( 9.331903152615748098, 11.35703883385568780, 7.000000000000000000 ) ) ;
#24544 = ADVANCED_FACE ( 'NONE', ( #12502 ), #27941, .F. ) ;
#24545 = CARTESIAN_POINT ( 'NONE',  ( -29.58401177971029838, 0.6647329222074543909, -8.776217634601312767 ) ) ;
#24546 = EDGE_CURVE ( 'NONE', #35208, #27705, #37288, .T. ) ;
#24547 = CARTESIAN_POINT ( 'NONE',  ( 34.31971835247910718, -13.79709225594373834, -8.423480077211841888 ) ) ;
#24548 = EDGE_CURVE ( 'NONE', #9704, #37413, #34442, .T. ) ;
#24549 = ORIENTED_EDGE ( 'NONE', *, *, #3911, .F. ) ;
#24550 = DIRECTION ( 'NONE',  ( 0.000000000000000000, 0.000000000000000000, 1.000000000000000000 ) ) ;
#24551 = EDGE_LOOP ( 'NONE', ( #18831, #14323, #27733, #7323 ) ) ;
#24552 = LINE ( 'NONE', #17872, #23606 ) ;
#24553 = DIRECTION ( 'NONE',  ( 1.000000000000000000, 0.000000000000000000, 0.000000000000000000 ) ) ;
#24554 = VECTOR ( 'NONE', #37975, 1000.000000000000000 ) ;
#24555 = AXIS2_PLACEMENT_3D ( 'NONE', #12045, #3100, #19942 ) ;
#24556 = LINE ( 'NONE', #27996, #32429 ) ;
#24557 = ORIENTED_EDGE ( 'NONE', *, *, #3090, .F. ) ;
#24558 = CARTESIAN_POINT ( 'NONE',  ( -4.066748194678229567, 36.38340522611666472, -9.294197595149157110 ) ) ;
#24559 = CARTESIAN_POINT ( 'NONE',  ( -20.23296131041716706, 28.12381335138030636, 0.000000000000000000 ) ) ;
#24560 = DIRECTION ( 'NONE',  ( -1.000000000000000000, 0.000000000000000000, 0.000000000000000000 ) ) ;
#24561 = CIRCLE ( 'NONE', #13537, 1.000000000000000888 ) ;
#24562 = DIRECTION ( 'NONE',  ( 0.000000000000000000, 0.000000000000000000, -1.000000000000000000 ) ) ;
#24563 = CARTESIAN_POINT ( 'NONE',  ( 16.64356867624101000, -11.98442300389733717, -30.00000000000002487 ) ) ;
#24564 = ADVANCED_FACE ( 'NONE', ( #18998 ), #6593, .F. ) ;
#24565 = CARTESIAN_POINT ( 'NONE',  ( 19.45606358795933843, 15.84753467433722562, -7.419582043610376765 ) ) ;
#24566 = CARTESIAN_POINT ( 'NONE',  ( 13.33950791723536611, 29.76583335417164733, -9.070794986034909968 ) ) ;
#24567 = VERTEX_POINT ( 'NONE', #31389 ) ;
#24568 = CARTESIAN_POINT ( 'NONE',  ( -20.17546868353657885, 9.912285996584582648, -18.01224743220988955 ) ) ;
#24569 = CARTESIAN_POINT ( 'NONE',  ( 4.817371740575539185, 23.83900317890011067, 23.00000000000000000 ) ) ;
#24570 = EDGE_CURVE ( 'NONE', #15697, #20746, #6962, .T. ) ;
#24571 = CARTESIAN_POINT ( 'NONE',  ( 13.18019970074355385, -23.10295469650971256, -15.43347796454282062 ) ) ;
#24572 = DIRECTION ( 'NONE',  ( -1.000000000000000000, 0.000000000000000000, 0.000000000000000000 ) ) ;
#24573 = CARTESIAN_POINT ( 'NONE',  ( -16.77267017469753085, -29.13948811618693924, -13.79123840944732748 ) ) ;
#24574 = CARTESIAN_POINT ( 'NONE',  ( -14.72251014768929167, 25.44185296451583866, -10.65018569441744134 ) ) ;
#24575 = CARTESIAN_POINT ( 'NONE',  ( -18.83446081530439642, -22.42967529457653342, -14.99109861493270834 ) ) ;
#24576 = CARTESIAN_POINT ( 'NONE',  ( 11.67685997438431045, -23.90497018467267765, -13.60458191810863049 ) ) ;
#24577 = CARTESIAN_POINT ( 'NONE',  ( 11.48173768534035943, 32.16538668264416145, 10.49999999999999822 ) ) ;
#24578 = ORIENTED_EDGE ( 'NONE', *, *, #31412, .F. ) ;
#24579 = ORIENTED_EDGE ( 'NONE', *, *, #14965, .F. ) ;
#24580 = CARTESIAN_POINT ( 'NONE',  ( -8.116341641279710473, 24.50416309976997908, -18.90493885958451159 ) ) ;
#24581 = CARTESIAN_POINT ( 'NONE',  ( 0.9938779058054629800, 37.09261900150649893, 10.49999999999999822 ) ) ;
#24582 = FACE_OUTER_BOUND ( 'NONE', #318, .T. ) ;
#24583 = AXIS2_PLACEMENT_3D ( 'NONE', #38432, #19951, #4507 ) ;
#24584 = AXIS2_PLACEMENT_3D ( 'NONE', #36904, #30615, #33671 ) ;
#24585 = CARTESIAN_POINT ( 'NONE',  ( -9.359089477944888102, 11.31962006718894109, 10.49999999999999822 ) ) ;
#24586 = EDGE_LOOP ( 'NONE', ( #9155, #5885, #28288 ) ) ;
#24587 = CARTESIAN_POINT ( 'NONE',  ( 28.31319793978629917, 0.1723095648249480527, -12.55177946987335424 ) ) ;
#24588 = LINE ( 'NONE', #25185, #37530 ) ;
#24589 = DIRECTION ( 'NONE',  ( 1.000000000000000000, 0.000000000000000000, 0.000000000000000000 ) ) ;
#24590 = CIRCLE ( 'NONE', #1248, 1.000000000000000000 ) ;
#24591 = B_SPLINE_SURFACE_WITH_KNOTS ( 'NONE', 1, 3, ( 
 ( #4363, #32616, #1323, #35657, #16161, #28547, #721, #28945, #4160, #13505 ),
 ( #25893, #38292, #25488, #34848, #10463, #35249, #7406, #26095, #38493, #8825 ) ),
 .UNSPECIFIED., .F., .F., .F.,
 ( 2, 2 ),
 ( 4, 2, 2, 2, 4 ),
 ( 0.000000000000000000, 1.000000000000000000 ),
 ( 1.875797233020303878, 2.268496314719027129, 2.661195396417750381, 3.053894478116473632, 3.446593559815196883 ),
 .UNSPECIFIED. ) ;
#24592 = ORIENTED_EDGE ( 'NONE', *, *, #14579, .T. ) ;
#24593 = CARTESIAN_POINT ( 'NONE',  ( -30.74133289564772298, 0.02125651492519025493, -6.417068207764520693 ) ) ;
#24594 = DIRECTION ( 'NONE',  ( 1.000000000000000000, 0.000000000000000000, 0.000000000000000000 ) ) ;
#24595 = ORIENTED_EDGE ( 'NONE', *, *, #3320, .T. ) ;
#24596 = CARTESIAN_POINT ( 'NONE',  ( 33.05307263222019287, -5.890996608547069080, -9.885471256058895761 ) ) ;
#24597 = ORIENTED_EDGE ( 'NONE', *, *, #6164, .F. ) ;
#24598 = CARTESIAN_POINT ( 'NONE',  ( -7.450289500751556382, 38.62958991718460311, 13.32518128616595376 ) ) ;
#24599 = EDGE_CURVE ( 'NONE', #34935, #13116, #15426, .T. ) ;
#24600 = CARTESIAN_POINT ( 'NONE',  ( 4.311100837790133051E-14, -15.38567963534269900, 20.94377226548378701 ) ) ;
#24601 = CYLINDRICAL_SURFACE ( 'NONE', #3972, 0.5000000000000006661 ) ;
#24602 = CARTESIAN_POINT ( 'NONE',  ( -3.426866961292544644, 32.67295397237167975, 19.99202127657103034 ) ) ;
#24603 = DIRECTION ( 'NONE',  ( 0.000000000000000000, 0.000000000000000000, 1.000000000000000000 ) ) ;
#24604 = EDGE_LOOP ( 'NONE', ( #31405, #15735 ) ) ;
#24605 = LINE ( 'NONE', #31301, #26139 ) ;
#24606 = CARTESIAN_POINT ( 'NONE',  ( 13.26584437371809777, 27.13525491562438319, 12.00000000000000000 ) ) ;
#24607 = DIRECTION ( 'NONE',  ( 0.000000000000000000, 0.000000000000000000, 1.000000000000000000 ) ) ;
#24608 = DIRECTION ( 'NONE',  ( 1.000000000000000000, 0.000000000000000000, 0.000000000000000000 ) ) ;
#24610 = VECTOR ( 'NONE', #12128, 1000.000000000000000 ) ;
#24609 = CARTESIAN_POINT ( 'NONE',  ( 6.272699779124576658, 32.10004986042342523, -12.94969384604119433 ) ) ;
#24611 = CYLINDRICAL_SURFACE ( 'NONE', #24382, 18.00000000000000000 ) ;
#24612 = CARTESIAN_POINT ( 'NONE',  ( 17.27603859610683301, -25.39141712192287059, -11.41356120857962431 ) ) ;
#24613 = CARTESIAN_POINT ( 'NONE',  ( 7.713869163865849643, 10.18146832927074996, 10.49999999999999822 ) ) ;
#24614 = AXIS2_PLACEMENT_3D ( 'NONE', #6304, #12804, #3661 ) ;
#24615 = LINE ( 'NONE', #24211, #34573 ) ;
#24616 = CARTESIAN_POINT ( 'NONE',  ( 2.544902299099474519, 8.122308845603164684, 10.99387789255784398 ) ) ;
#24617 = ORIENTED_EDGE ( 'NONE', *, *, #19505, .F. ) ;
#24618 = CARTESIAN_POINT ( 'NONE',  ( -15.30065312247323028, 26.49437699940635937, -7.357947398261144301 ) ) ;
#24619 = CARTESIAN_POINT ( 'NONE',  ( -30.57450045107738035, -0.3656520783173805578, 16.87380292611442201 ) ) ;
#24620 = CARTESIAN_POINT ( 'NONE',  ( 13.92138958099786450, -24.59342578875250140, -12.55492369404029951 ) ) ;
#24621 = CARTESIAN_POINT ( 'NONE',  ( -3.494943660522439099, 10.76222879119470832, 12.00000000000000000 ) ) ;
#24622 = ORIENTED_EDGE ( 'NONE', *, *, #18293, .F. ) ;
#24623 = ORIENTED_EDGE ( 'NONE', *, *, #7160, .F. ) ;
#24624 = CARTESIAN_POINT ( 'NONE',  ( -9.436104724621630524, 18.21145219648997227, -29.31522508094131751 ) ) ;
#24625 = CARTESIAN_POINT ( 'NONE',  ( -20.57926088536441966, -27.21289976561331514, -4.999999999999997335 ) ) ;
#24626 = CARTESIAN_POINT ( 'NONE',  ( -19.48557158514985588, -11.25000000000002309, 0.000000000000000000 ) ) ;
#24627 = ORIENTED_EDGE ( 'NONE', *, *, #8680, .F. ) ;
#24628 = CARTESIAN_POINT ( 'NONE',  ( -28.18824097937255146, -7.837830145184667252, -15.82023872818571064 ) ) ;
#24629 = CARTESIAN_POINT ( 'NONE',  ( -12.49708442935645358, -22.55589311136183284, -16.45579901909083276 ) ) ;
#24630 = CARTESIAN_POINT ( 'NONE',  ( 38.42882785865584339, -4.479089857566261657, 11.00000000000000000 ) ) ;
#24631 = ORIENTED_EDGE ( 'NONE', *, *, #22434, .T. ) ;
#24632 = CARTESIAN_POINT ( 'NONE',  ( 20.47800464711415813, 1.727324350805305109, -28.73678694931549060 ) ) ;
#24633 = CARTESIAN_POINT ( 'NONE',  ( 6.811226782241714517, 35.33967249274190436, 9.500000000000000000 ) ) ;
#24634 = CARTESIAN_POINT ( 'NONE',  ( 13.05736835487433289, 16.11602540378438420, 7.000000000000000000 ) ) ;
#24635 = ORIENTED_EDGE ( 'NONE', *, *, #22803, .F. ) ;
#24636 = CARTESIAN_POINT ( 'NONE',  ( -23.33365362593783487, 0.5068941057029301422, -20.53583360551006010 ) ) ;
#24637 = ORIENTED_EDGE ( 'NONE', *, *, #9384, .T. ) ;
#24638 = CARTESIAN_POINT ( 'NONE',  ( 32.13235714270949472, -1.817784623349015360, -7.301148604131005193 ) ) ;
#24639 = VECTOR ( 'NONE', #26096, 1000.000000000000000 ) ;
#24640 = CARTESIAN_POINT ( 'NONE',  ( 4.811402195336492049, -19.97410447909037146, -30.00000000000001066 ) ) ;
#24641 = CARTESIAN_POINT ( 'NONE',  ( 29.39157470508798298, -22.49273609621582182, 17.42190598798393353 ) ) ;
#24642 = EDGE_CURVE ( 'NONE', #20723, #14246, #9573, .T. ) ;
#24643 = ORIENTED_EDGE ( 'NONE', *, *, #11864, .F. ) ;
#24644 = CARTESIAN_POINT ( 'NONE',  ( -22.20364817425843285, 3.543267544546572889, -20.85647020598273471 ) ) ;
#24645 = CIRCLE ( 'NONE', #22053, 15.00000000000000000 ) ;
#24646 = CARTESIAN_POINT ( 'NONE',  ( -10.16122020288868733, 33.53402030034415304, 7.000000000000000000 ) ) ;
#24647 = CARTESIAN_POINT ( 'NONE',  ( 7.577540944421576441, 33.15743037285414374, 12.00000000000000000 ) ) ;
#24648 = DIRECTION ( 'NONE',  ( 0.000000000000000000, 0.000000000000000000, 1.000000000000000000 ) ) ;
#24649 = EDGE_CURVE ( 'NONE', #29357, #25284, #17388, .T. ) ;
#24650 = DIRECTION ( 'NONE',  ( 0.8660254037844364872, -0.5000000000000038858, 0.000000000000000000 ) ) ;
#24651 = EDGE_CURVE ( 'NONE', #20746, #15697, #1127, .T. ) ;
#24652 = FACE_BOUND ( 'NONE', #23068, .T. ) ;
#24653 = CARTESIAN_POINT ( 'NONE',  ( 28.53381226737487708, 4.748233269553930214, 13.32518128616595909 ) ) ;
#24654 = VERTEX_POINT ( 'NONE', #31192 ) ;
#24655 = CARTESIAN_POINT ( 'NONE',  ( -23.77417876032645694, 7.953466752255449634, -9.369785356547680522 ) ) ;
#24656 = CARTESIAN_POINT ( 'NONE',  ( 5.458865582155095986, 18.48521636184714012, 6.000000000000000000 ) ) ;
#24657 = LINE ( 'NONE', #24855, #13612 ) ;
#24658 = CARTESIAN_POINT ( 'NONE',  ( 24.21359695930263101, -26.57684320323437532, -5.446510658207939670 ) ) ;
#24659 = DIRECTION ( 'NONE',  ( 1.000000000000000000, 0.000000000000000000, 0.000000000000000000 ) ) ;
#24660 = CARTESIAN_POINT ( 'NONE',  ( 12.51893876027292940, 21.25235172184055443, -18.42282389506313223 ) ) ;
#24661 = ORIENTED_EDGE ( 'NONE', *, *, #29498, .F. ) ;
#24662 = CARTESIAN_POINT ( 'NONE',  ( -12.44972444764569453, 16.77980448052251106, -26.34956027326842687 ) ) ;
#24663 = CARTESIAN_POINT ( 'NONE',  ( -27.76392016787528760, -12.00403709334065461, 20.69868183039782039 ) ) ;
#24664 = ADVANCED_FACE ( 'NONE', ( #12306 ), #3357, .T. ) ;
#24665 = EDGE_CURVE ( 'NONE', #34232, #16528, #316, .T. ) ;
#24666 = CARTESIAN_POINT ( 'NONE',  ( -16.99999999999999645, 22.50000000000000355, 11.00000000000000178 ) ) ;
#24667 = CARTESIAN_POINT ( 'NONE',  ( 11.91014968976024235, 19.36310277583015349, -21.62019219126923275 ) ) ;
#24668 = ORIENTED_EDGE ( 'NONE', *, *, #25017, .F. ) ;
#24669 = CARTESIAN_POINT ( 'NONE',  ( -16.00000000000000000, 22.50000000000000355, 6.000000000000000000 ) ) ;
#24670 = AXIS2_PLACEMENT_3D ( 'NONE', #13957, #39342, #17222 ) ;
#24671 = EDGE_LOOP ( 'NONE', ( #26269, #17300, #9343, #20831, #30893, #7091, #38119 ) ) ;
#24673 = FACE_OUTER_BOUND ( 'NONE', #17401, .T. ) ;
#24672 = CARTESIAN_POINT ( 'NONE',  ( -15.30029427371034600, 27.09079015021717396, -5.942535154850186352 ) ) ;
#24674 = CARTESIAN_POINT ( 'NONE',  ( -15.38607054502407756, -26.33262433206096986, -8.289753305509513837 ) ) ;
#24675 = LINE ( 'NONE', #30781, #14616 ) ;
#24676 = CARTESIAN_POINT ( 'NONE',  ( -31.78065895063095780, -15.41279462978935832, -11.07266024125810056 ) ) ;
#24677 = CARTESIAN_POINT ( 'NONE',  ( -9.122435668794345531, -19.14094883146207593, -25.10522684686861439 ) ) ;
#24678 = CARTESIAN_POINT ( 'NONE',  ( -14.76265446396242176, 21.90695576875699757, 10.49999999999999467 ) ) ;
#24679 = CARTESIAN_POINT ( 'NONE',  ( 13.13796970620712656, 19.50823006588858632, -19.62116264178829184 ) ) ;
#24680 = EDGE_LOOP ( 'NONE', ( #15925, #20650, #39194, #38062 ) ) ;
#24681 = CARTESIAN_POINT ( 'NONE',  ( 26.68456133973351641, 4.675186248811364464, -5.953666022845518491 ) ) ;
#24682 = CARTESIAN_POINT ( 'NONE',  ( -11.11016527260153630, 31.83082137946488643, 7.500000000000004441 ) ) ;
#24683 = DIRECTION ( 'NONE',  ( 1.000000000000000000, 0.000000000000000000, 0.000000000000000000 ) ) ;
#24684 = DIRECTION ( 'NONE',  ( 0.000000000000000000, 0.000000000000000000, 1.000000000000000000 ) ) ;
#24685 = VERTEX_POINT ( 'NONE', #18610 ) ;
#24686 = CARTESIAN_POINT ( 'NONE',  ( -20.55327584008562170, -0.1442271758602391429, -28.67149428179880744 ) ) ;
#24687 = CARTESIAN_POINT ( 'NONE',  ( 29.17685817419758365, -0.2385013389979390996, -11.56797761538647329 ) ) ;
#24688 = VECTOR ( 'NONE', #3708, 999.9999999999998863 ) ;
#24689 = CARTESIAN_POINT ( 'NONE',  ( -5.644276917315528941, 36.40655018617697891, 10.49999999999999467 ) ) ;
#24690 = CARTESIAN_POINT ( 'NONE',  ( 23.50870743262586160, -18.52420134090368720, 20.69868183039761789 ) ) ;
#24691 = AXIS2_PLACEMENT_3D ( 'NONE', #11920, #35906, #30418 ) ;
#24692 = VERTEX_POINT ( 'NONE', #28734 ) ;
#24693 = EDGE_CURVE ( 'NONE', #9581, #29091, #19194, .T. ) ;
#24694 = CARTESIAN_POINT ( 'NONE',  ( 27.08779848459123585, 7.221796966026769127, -13.42901749168596304 ) ) ;
#24695 = CARTESIAN_POINT ( 'NONE',  ( -13.94482798346716201, 26.50521816028930644, 7.000000000000000000 ) ) ;
#24696 = ORIENTED_EDGE ( 'NONE', *, *, #9154, .T. ) ;
#24697 = VECTOR ( 'NONE', #7510, 999.9999999999998863 ) ;
#24698 = CARTESIAN_POINT ( 'NONE',  ( 2.525645716490524606, 8.212903943950921715, 11.00000000000000000 ) ) ;
#24699 = CARTESIAN_POINT ( 'NONE',  ( -27.36225479881674616, 10.16098284219160597, 22.99999999999999645 ) ) ;
#24700 = LINE ( 'NONE', #25098, #22907 ) ;
#24701 = CARTESIAN_POINT ( 'NONE',  ( 2.721668488675992759, 37.91170157744703317, -7.120364383801717878 ) ) ;
#24702 = CARTESIAN_POINT ( 'NONE',  ( 0.000000000000000000, 22.50000000000000355, 7.000000000000000000 ) ) ;
#24703 = DIRECTION ( 'NONE',  ( 0.000000000000000000, 0.000000000000000000, -1.000000000000000000 ) ) ;
#24704 = DIRECTION ( 'NONE',  ( 1.000000000000000000, 0.000000000000000000, 0.000000000000000000 ) ) ;
#24705 = DIRECTION ( 'NONE',  ( 1.000000000000000000, 0.000000000000000000, 0.000000000000000000 ) ) ;
#24706 = CARTESIAN_POINT ( 'NONE',  ( 11.89076109989491314, 31.64473967131989340, 7.202682876670051471 ) ) ;
#24707 = FILL_AREA_STYLE_COLOUR ( '', #11940 ) ;
#24708 = CARTESIAN_POINT ( 'NONE',  ( 10.18918489279338147, 17.95568076346413733, -28.02701222315408813 ) ) ;
#24709 = DIRECTION ( 'NONE',  ( 1.000000000000000000, 0.000000000000000000, 0.000000000000000000 ) ) ;
#24710 = ORIENTED_EDGE ( 'NONE', *, *, #18685, .T. ) ;
#24712 = DIRECTION ( 'NONE',  ( -0.04273212933194531216, -0.8153776007405577619, 0.5773502691896226224 ) ) ;
#24711 = CARTESIAN_POINT ( 'NONE',  ( -17.77270048994293106, 18.00536303972542029, -10.82195543332399978 ) ) ;
#24713 = CARTESIAN_POINT ( 'NONE',  ( 4.881458130820872654, -28.77689918168226768, 11.00000000000000178 ) ) ;
#24714 = CARTESIAN_POINT ( 'NONE',  ( 9.504747149499191750, -18.16341882422712573, -29.34820719226206975 ) ) ;
#24715 = EDGE_CURVE ( 'NONE', #880, #6684, #14115, .T. ) ;
#24716 = CARTESIAN_POINT ( 'NONE',  ( -14.22557620116472421, -18.08049471867423819, -22.27683892693457679 ) ) ;
#24717 = CARTESIAN_POINT ( 'NONE',  ( 30.17922767059877032, -0.7536324250949817394, 17.42190598798393353 ) ) ;
#24718 = CARTESIAN_POINT ( 'NONE',  ( 14.01964074023701379, 23.95961702490197709, -13.51097757283367429 ) ) ;
#24719 = ORIENTED_EDGE ( 'NONE', *, *, #2018, .F. ) ;
#24720 = DIRECTION ( 'NONE',  ( -0.000000000000000000, -0.000000000000000000, -1.000000000000000000 ) ) ;
#24721 = CARTESIAN_POINT ( 'NONE',  ( -13.60973832552192775, -24.10531655226265357, -13.51781039733256229 ) ) ;
#24722 = CARTESIAN_POINT ( 'NONE',  ( -15.20016916874712365, -27.86040092368495280, 14.53008259254011136 ) ) ;
#24723 = CARTESIAN_POINT ( 'NONE',  ( -15.77773026942784185, -13.10308996503666101, -29.22635037987518913 ) ) ;
#24724 = CARTESIAN_POINT ( 'NONE',  ( -0.3788947411688599609, -24.40711055506037397, -9.394763118258644852 ) ) ;
#24725 = CARTESIAN_POINT ( 'NONE',  ( 15.34816150809986013, 25.71129999911718755, -8.302060856640464337 ) ) ;
#24726 = CARTESIAN_POINT ( 'NONE',  ( 19.07176576169624838, 8.856411245019137013, -24.40134652798608172 ) ) ;
#24727 = PLANE ( 'NONE',  #4358 ) ;
#24728 = AXIS2_PLACEMENT_3D ( 'NONE', #9325, #34699, #18667 ) ;
#24729 = CARTESIAN_POINT ( 'NONE',  ( -4.949370363199405709, 34.62182401653869590, -11.09161847530103984 ) ) ;
#24730 = ORIENTED_EDGE ( 'NONE', *, *, #34199, .F. ) ;
#24731 = CARTESIAN_POINT ( 'NONE',  ( -20.04600691274970714, -4.289688609580842638, -30.00000000000000000 ) ) ;
#24732 = CARTESIAN_POINT ( 'NONE',  ( -25.55085611915244570, 8.900480655597387880, 12.73282698325014550 ) ) ;
#24733 = EDGE_LOOP ( 'NONE', ( #39426, #9501, #34294, #29723 ) ) ;
#24734 = FACE_OUTER_BOUND ( 'NONE', #36243, .T. ) ;
#24735 = DIRECTION ( 'NONE',  ( -0.9510565162951541973, -0.3090169943749456194, 0.000000000000000000 ) ) ;
#24736 = CARTESIAN_POINT ( 'NONE',  ( -20.49737880956387670, 1.361707026421257183, -28.72413233336064664 ) ) ;
#24737 = EDGE_CURVE ( 'NONE', #2507, #32523, #29344, .T. ) ;
#24738 = CARTESIAN_POINT ( 'NONE',  ( 29.79256524754709901, -11.96324064677705401, -13.83857493703202657 ) ) ;
#24739 = EDGE_CURVE ( 'NONE', #3978, #36251, #13697, .T. ) ;
#24740 = AXIS2_PLACEMENT_3D ( 'NONE', #17120, #26647, #1671 ) ;
#24741 = ORIENTED_EDGE ( 'NONE', *, *, #6160, .T. ) ;
#24742 = FACE_OUTER_BOUND ( 'NONE', #8216, .T. ) ;
#24743 = VERTEX_POINT ( 'NONE', #20007 ) ;
#24744 = CARTESIAN_POINT ( 'NONE',  ( -7.126083911573537044, 10.99048532364579245, 9.500000000000000000 ) ) ;
#24745 = CARTESIAN_POINT ( 'NONE',  ( 4.591666147298500533, 15.32946292166668556, 7.000000000000000000 ) ) ;
#24746 = EDGE_CURVE ( 'NONE', #11507, #31582, #38127, .T. ) ;
#24747 = CARTESIAN_POINT ( 'NONE',  ( -18.00000000000000000, 22.50000000000001066, 3.000000000000000000 ) ) ;
#24748 = VERTEX_POINT ( 'NONE', #7194 ) ;
#24749 = CARTESIAN_POINT ( 'NONE',  ( -2.264496061979761166, 20.62872948969808817, -27.72085884865996164 ) ) ;
#24750 = DIRECTION ( 'NONE',  ( -1.000000000000000000, -1.224646799147353947E-16, 0.000000000000000000 ) ) ;
#24751 = DIRECTION ( 'NONE',  ( -0.5877852522924796874, -0.8090169943749426773, 0.000000000000000000 ) ) ;
#24752 = AXIS2_PLACEMENT_3D ( 'NONE', #2059, #36182, #33142 ) ;
#24753 = CARTESIAN_POINT ( 'NONE',  ( -7.713869163866016621, 10.18146832927085121, 10.50000000000000711 ) ) ;
#24754 = CARTESIAN_POINT ( 'NONE',  ( 27.47508384939705550, -22.51065662569030223, -10.20476834957493395 ) ) ;
#24755 = CARTESIAN_POINT ( 'NONE',  ( 19.54882725460437598, 14.50357661510694385, -10.87434924481359921 ) ) ;
#24756 = CARTESIAN_POINT ( 'NONE',  ( 10.77366068177361491, 25.64106453496501103, -16.05906032174032916 ) ) ;
#24757 = VERTEX_POINT ( 'NONE', #1516 ) ;
#24758 = CARTESIAN_POINT ( 'NONE',  ( -20.68145323613758180, 13.65869002226675910, -6.453259564398977410 ) ) ;
#24759 = CARTESIAN_POINT ( 'NONE',  ( -14.84160187385925589, 20.32586711127000711, 7.500000000000004441 ) ) ;
#24760 = CARTESIAN_POINT ( 'NONE',  ( 11.27261089013053308, -20.45316121506556684, -20.52991339251368075 ) ) ;
#24761 = B_SPLINE_CURVE_WITH_KNOTS ( 'NONE', 3,
 ( #2696, #33192, #39860, #21381, #10188, #28272 ),
 .UNSPECIFIED., .F., .F.,
 ( 4, 2, 4 ),
 ( 0.000000000000000000, 0.5000000000000000000, 1.000000000000000000 ),
 .UNSPECIFIED. ) ;
#24762 = DIRECTION ( 'NONE',  ( 1.000000000000000000, 0.000000000000000000, 0.000000000000000000 ) ) ;
#24763 = EDGE_CURVE ( 'NONE', #34172, #15434, #16964, .T. ) ;
#24764 = EDGE_CURVE ( 'NONE', #5911, #32217, #5677, .T. ) ;
#24765 = CARTESIAN_POINT ( 'NONE',  ( 17.81784622497951176, -13.85677843414110555, -30.00000000000001421 ) ) ;
#24766 = CARTESIAN_POINT ( 'NONE',  ( -10.81260707898136708, 32.90853150812170469, 10.49999999999999822 ) ) ;
#24767 = ADVANCED_FACE ( 'NONE', ( #22432 ), #22232, .T. ) ;
#24768 = CARTESIAN_POINT ( 'NONE',  ( -11.86970878780117467, 19.40623504760773699, -21.61272265936945658 ) ) ;
#24769 = CONICAL_SURFACE ( 'NONE', #7241, 1.000000000000000888, 0.7853981633974552734 ) ;
#24770 = CARTESIAN_POINT ( 'NONE',  ( -19.68546449317618752, -22.09548208296689609, -14.94786901843714588 ) ) ;
#24771 = CARTESIAN_POINT ( 'NONE',  ( 10.56601941806194667, -25.32872364259939246, -8.337176484249591013 ) ) ;
#24772 = FACE_OUTER_BOUND ( 'NONE', #14807, .T. ) ;
#24773 = EDGE_LOOP ( 'NONE', ( #11807, #18009, #4528, #24792 ) ) ;
#24774 = CARTESIAN_POINT ( 'NONE',  ( -10.00978049950840365, 33.59848884444493677, -8.937983356255100986 ) ) ;
#24775 = CARTESIAN_POINT ( 'NONE',  ( 0.5000000000000000000, 37.39061994947686429, 10.82238861112342043 ) ) ;
#24776 = CARTESIAN_POINT ( 'NONE',  ( -14.36830325120615548, 20.48707633493503621, 7.000000000000000000 ) ) ;
#24777 = CARTESIAN_POINT ( 'NONE',  ( -9.156995300982224251, 10.74712803024086938, 10.82238861112329609 ) ) ;
#24778 = ORIENTED_EDGE ( 'NONE', *, *, #23651, .T. ) ;
#24779 = CARTESIAN_POINT ( 'NONE',  ( 20.52560773323338950, 0.8855934539933489891, -28.70794251307378531 ) ) ;
#24780 = CARTESIAN_POINT ( 'NONE',  ( -8.559512017365658920, 19.71884705062586107, 6.000000000000000000 ) ) ;
#24781 = VECTOR ( 'NONE', #1458, 1000.000000000000000 ) ;
#24782 = DIRECTION ( 'NONE',  ( -0.000000000000000000, -0.000000000000000000, -1.000000000000000000 ) ) ;
#24783 = ORIENTED_EDGE ( 'NONE', *, *, #38159, .F. ) ;
#24784 = CARTESIAN_POINT ( 'NONE',  ( -25.18774962667799855, 0.4227707108053092577, -17.44299664577632214 ) ) ;
#24785 = LINE ( 'NONE', #9558, #34555 ) ;
#24786 = ADVANCED_FACE ( 'NONE', ( #26085 ), #13290, .T. ) ;
#24787 = VERTEX_POINT ( 'NONE', #19801 ) ;
#24788 = CARTESIAN_POINT ( 'NONE',  ( 33.33943358355180919, -6.927885457322644491, -9.856513271172966384 ) ) ;
#24789 = EDGE_CURVE ( 'NONE', #21042, #4736, #14765, .T. ) ;
#24790 = AXIS2_PLACEMENT_3D ( 'NONE', #40112, #37473, #3341 ) ;
#24791 = EDGE_CURVE ( 'NONE', #29047, #36540, #28382, .T. ) ;
#24792 = ORIENTED_EDGE ( 'NONE', *, *, #2842, .F. ) ;
#24793 = CARTESIAN_POINT ( 'NONE',  ( -1.926143243141299921, 40.30103163374180752, 12.73282698324853079 ) ) ;
#24794 = CARTESIAN_POINT ( 'NONE',  ( 4.290760370981760375E-14, -17.87737810982027398, 20.50957957746029336 ) ) ;
#24795 = CARTESIAN_POINT ( 'NONE',  ( -1.400691654708310585, 37.43445890845833901, 7.000000000000000000 ) ) ;
#24796 = CARTESIAN_POINT ( 'NONE',  ( 1.073573824165682256, 32.41755745572909575, 20.25080042701565830 ) ) ;
#24797 = EDGE_CURVE ( 'NONE', #18928, #34264, #34887, .T. ) ;
#24798 = CARTESIAN_POINT ( 'NONE',  ( 7.935770203493858865, 22.34671014717335780, 6.000000000000000000 ) ) ;
#24799 = EDGE_LOOP ( 'NONE', ( #20176, #29312, #23966, #30145, #38883, #675, #5747 ) ) ;
#24800 = CONICAL_SURFACE ( 'NONE', #30671, 1.000000000000013101, 0.7853981633974566057 ) ;
#24801 = CARTESIAN_POINT ( 'NONE',  ( 3.938766756526715263, 8.166638875703695177, 10.49999999999999822 ) ) ;
#24802 = CARTESIAN_POINT ( 'NONE',  ( 10.20374679324142342, 33.03312760923203939, 10.49999999999999645 ) ) ;
#24803 = DIRECTION ( 'NONE',  ( 0.3090169943749465631, -0.9510565162951538642, 0.000000000000000000 ) ) ;
#24804 = CARTESIAN_POINT ( 'NONE',  ( -7.312041872459064784, 25.58773265502866678, 12.00000000000000000 ) ) ;
#24805 = CARTESIAN_POINT ( 'NONE',  ( 9.133087869482302779, 35.68701272469542829, -4.999999999999999112 ) ) ;
#24806 = CYLINDRICAL_SURFACE ( 'NONE', #16614, 0.4999999999999995559 ) ;
#24807 = AXIS2_PLACEMENT_3D ( 'NONE', #33239, #23675, #11884 ) ;
#24808 = CARTESIAN_POINT ( 'NONE',  ( 11.58194518081183944, -17.66261609970828061, -26.04779429940238700 ) ) ;
#24809 = CARTESIAN_POINT ( 'NONE',  ( -9.776449189803978257, 11.12328344838602767, 7.150945465624456432 ) ) ;
#24810 = LINE ( 'NONE', #30317, #6037 ) ;
#24811 = FACE_OUTER_BOUND ( 'NONE', #16347, .T. ) ;
#24812 = ADVANCED_FACE ( 'NONE', ( #4150 ), #25685, .T. ) ;
#24813 = VERTEX_POINT ( 'NONE', #25291 ) ;
#24814 = CARTESIAN_POINT ( 'NONE',  ( -11.84249978353584964, 18.76146840030286711, -22.76060117347688561 ) ) ;
#24815 = CONICAL_SURFACE ( 'NONE', #22838, 1.000000000000004441, 0.7853981633974528309 ) ;
#24816 = CARTESIAN_POINT ( 'NONE',  ( -28.17486335743007686, -23.56478353225083922, 17.42190598798394774 ) ) ;
#24817 = CARTESIAN_POINT ( 'NONE',  ( 14.73164756419078536, -25.80301381421831763, -9.711130863355320386 ) ) ;
#24818 = CARTESIAN_POINT ( 'NONE',  ( 2.485571585149743523, -11.24999999999995737, 10.00000000000000000 ) ) ;
#24819 = ORIENTED_EDGE ( 'NONE', *, *, #34244, .F. ) ;
#24820 = VERTEX_POINT ( 'NONE', #28536 ) ;
#24821 = CARTESIAN_POINT ( 'NONE',  ( -14.26477007067611247, 27.22168516859696297, -10.08655638140778343 ) ) ;
#24822 = CARTESIAN_POINT ( 'NONE',  ( -19.86157376375091488, -26.35897367172421468, -9.048130445010871270 ) ) ;
#24823 = FACE_BOUND ( 'NONE', #15988, .T. ) ;
#24824 = ORIENTED_EDGE ( 'NONE', *, *, #14701, .F. ) ;
#24825 = CARTESIAN_POINT ( 'NONE',  ( -34.75757652648396601, -9.699577992749013333, -8.031966576075948439 ) ) ;
#24826 = PRODUCT_DEFINITION_CONTEXT ( 'detailed design', #14524, 'design' ) ;
#24827 = CARTESIAN_POINT ( 'NONE',  ( -9.318012453479679991, -18.39830250787939292, -28.09118640345915452 ) ) ;
#24828 = CONICAL_SURFACE ( 'NONE', #7303, 0.4999999999999955036, 0.7853981633974447263 ) ;
#24829 = DIRECTION ( 'NONE',  ( 1.000000000000000000, 0.000000000000000000, 0.000000000000000000 ) ) ;
#24830 = ORIENTED_EDGE ( 'NONE', *, *, #21507, .F. ) ;
#24831 = CARTESIAN_POINT ( 'NONE',  ( 30.66646233963074053, 0.1658458930697631339, -5.946129198316283393 ) ) ;
#24832 = CARTESIAN_POINT ( 'NONE',  ( -11.48173768534023154, 32.16538668264431777, 7.000000000000000000 ) ) ;
#24833 = CARTESIAN_POINT ( 'NONE',  ( -2.494943660522439099, 10.76222879119470832, 12.00000000000000000 ) ) ;
#24834 = EDGE_LOOP ( 'NONE', ( #30054, #17708, #17049, #20685 ) ) ;
#24835 = CARTESIAN_POINT ( 'NONE',  ( -30.37298050052526577, -0.02580378418990478956, -8.296495627326031297 ) ) ;
#24836 = ORIENTED_EDGE ( 'NONE', *, *, #19189, .T. ) ;
#24837 = CARTESIAN_POINT ( 'NONE',  ( 20.74370561925601564, -0.3015135946092845076, -27.37350676080033196 ) ) ;
#24838 = AXIS2_PLACEMENT_3D ( 'NONE', #26510, #17385, #8623 ) ;
#24839 = CARTESIAN_POINT ( 'NONE',  ( -6.026386652613112460, -19.60672597950843965, -29.99999999999999289 ) ) ;
#24840 = CARTESIAN_POINT ( 'NONE',  ( 20.56996978659388731, -26.19496882840791940, 17.42190598798392642 ) ) ;
#24841 = ADVANCED_FACE ( 'NONE', ( #37686 ), #35446, .F. ) ;
#24842 = ORIENTED_EDGE ( 'NONE', *, *, #39274, .F. ) ;
#24843 = CARTESIAN_POINT ( 'NONE',  ( -20.27261486981255700, 4.299876162282100012, -27.04395481629711995 ) ) ;
#24844 = DIRECTION ( 'NONE',  ( -0.5000000000000041078, -0.8660254037844362651, 0.000000000000000000 ) ) ;
#24845 = FACE_OUTER_BOUND ( 'NONE', #15677, .T. ) ;
#24846 = AXIS2_PLACEMENT_3D ( 'NONE', #17761, #36242, #39271 ) ;
#24847 = DIRECTION ( 'NONE',  ( 1.000000000000000000, 0.000000000000000000, 0.000000000000000000 ) ) ;
#24848 = CARTESIAN_POINT ( 'NONE',  ( -0.5000000000000005551, 32.50000000000000000, 10.49999999999999645 ) ) ;
#24849 = AXIS2_PLACEMENT_3D ( 'NONE', #17639, #17231, #5620 ) ;
#24850 = CYLINDRICAL_SURFACE ( 'NONE', #10618, 1.000000000000000888 ) ;
#24851 = VECTOR ( 'NONE', #5220, 1000.000000000000000 ) ;
#24852 = CARTESIAN_POINT ( 'NONE',  ( 17.15083734909311630, 27.26712758906529643, 12.73282698324853257 ) ) ;
#24853 = CARTESIAN_POINT ( 'NONE',  ( -19.73431017332725901, 6.432349763256766551, -26.55950874972816678 ) ) ;
#24854 = CARTESIAN_POINT ( 'NONE',  ( 10.77090408390491127, 15.39748370681878775, 12.00000000000000000 ) ) ;
#24855 = CARTESIAN_POINT ( 'NONE',  ( 8.238488885696289898, 24.65111619403943877, 7.000000000000000000 ) ) ;
#24856 = CARTESIAN_POINT ( 'NONE',  ( 15.61542113695269762, -16.24202176434524958, -23.22363185398829089 ) ) ;
#24857 = DIRECTION ( 'NONE',  ( 0.000000000000000000, 0.000000000000000000, 1.000000000000000000 ) ) ;
#24858 = CARTESIAN_POINT ( 'NONE',  ( 15.32268921037612586, 27.10638078547256669, -4.999999999999999112 ) ) ;
#24859 = AXIS2_PLACEMENT_3D ( 'NONE', #7514, #20526, #32524 ) ;
#24860 = EDGE_LOOP ( 'NONE', ( #31624, #34972, #9716, #6888 ) ) ;
#24861 = CARTESIAN_POINT ( 'NONE',  ( -16.22408403259154852, 24.10865257618694102, -5.000000000000000000 ) ) ;
#24862 = CARTESIAN_POINT ( 'NONE',  ( -26.56332897235036228, -4.302820985780034135, 20.25080042701566541 ) ) ;
#24863 = EDGE_CURVE ( 'NONE', #27538, #18534, #15481, .T. ) ;
#24864 = AXIS2_PLACEMENT_3D ( 'NONE', #35542, #17063, #7500 ) ;
#24865 = FACE_OUTER_BOUND ( 'NONE', #24376, .T. ) ;
#24866 = CARTESIAN_POINT ( 'NONE',  ( 15.25901309658000748, 26.31556895002759688, -7.828263233713028235 ) ) ;
#24867 = ORIENTED_EDGE ( 'NONE', *, *, #22185, .F. ) ;
#24868 = DIRECTION ( 'NONE',  ( 0.000000000000000000, 0.000000000000000000, 1.000000000000000000 ) ) ;
#24869 = VERTEX_POINT ( 'NONE', #3951 ) ;
#24871 = CARTESIAN_POINT ( 'NONE',  ( -3.211402178667006169, 32.38366924255629442, 6.000000000000000000 ) ) ;
#24870 = CARTESIAN_POINT ( 'NONE',  ( -11.55131371627300751, 19.04040767486820940, -22.71169724931953482 ) ) ;
#24872 = CARTESIAN_POINT ( 'NONE',  ( -11.33073861718174236, -20.44271155232068793, -20.52225160477277299 ) ) ;
#24873 = CARTESIAN_POINT ( 'NONE',  ( 5.348106467989403257, 35.16482219193073178, 13.00000000000000178 ) ) ;
#24874 = ORIENTED_EDGE ( 'NONE', *, *, #27020, .T. ) ;
#24875 = CARTESIAN_POINT ( 'NONE',  ( -32.12531547378703323, -14.37956203216488049, -11.07915535210666924 ) ) ;
#24876 = CARTESIAN_POINT ( 'NONE',  ( -13.73743966556329887, -26.04782550432431165, -7.836754151373586552 ) ) ;
#24877 = DIRECTION ( 'NONE',  ( 1.000000000000000000, 0.000000000000000000, 0.000000000000000000 ) ) ;
#24878 = CARTESIAN_POINT ( 'NONE',  ( 15.30794202828028361, 22.03102559147765405, -12.64584791074079284 ) ) ;
#24879 = EDGE_LOOP ( 'NONE', ( #33106, #33270, #24231, #16205 ) ) ;
#24880 = CARTESIAN_POINT ( 'NONE',  ( 22.62389337662363076, 5.347323980972150892, -17.84045304431403522 ) ) ;
#24881 = CARTESIAN_POINT ( 'NONE',  ( 8.312035131040566682, 19.41226734497195849, 12.00000000000000000 ) ) ;
#24882 = CARTESIAN_POINT ( 'NONE',  ( -5.440908595777636414, 35.94977745735568675, 11.00000000000000000 ) ) ;
#24883 = ADVANCED_FACE ( 'NONE', ( #4354 ), #29145, .F. ) ;
#24884 = CARTESIAN_POINT ( 'NONE',  ( -3.813962023474485985, 32.29559562678527129, 10.00000000000000000 ) ) ;
#24885 = EDGE_LOOP ( 'NONE', ( #21980, #39410, #23129, #3135 ) ) ;
#24886 = CARTESIAN_POINT ( 'NONE',  ( -29.84605808524375803, -0.2300388918764082746, -10.15910822650677048 ) ) ;
#24887 = CARTESIAN_POINT ( 'NONE',  ( 24.67091124240074862, 0.2026903286398813175, -18.42105149346458859 ) ) ;
#24888 = FACE_OUTER_BOUND ( 'NONE', #4147, .T. ) ;
#24889 = AXIS2_PLACEMENT_3D ( 'NONE', #39091, #17782, #2128 ) ;
#24890 = CARTESIAN_POINT ( 'NONE',  ( 27.68412949013584168, -10.20944236609925859, 20.69868183039781329 ) ) ;
#24891 = ORIENTED_EDGE ( 'NONE', *, *, #37458, .T. ) ;
#24892 = B_SPLINE_CURVE_WITH_KNOTS ( 'NONE', 3,
 ( #3265, #224, #36996, #33949 ),
 .UNSPECIFIED., .F., .F.,
 ( 4, 4 ),
 ( 0.000000000000000000, 1.000000000000000000 ),
 .UNSPECIFIED. ) ;
#24893 = CARTESIAN_POINT ( 'NONE',  ( -7.289639608743041066, -27.06962010326280321, -5.000000000000000000 ) ) ;
#24894 = AXIS2_PLACEMENT_3D ( 'NONE', #579, #15618, #10318 ) ;
#24895 = CARTESIAN_POINT ( 'NONE',  ( -10.44103466624267185, 32.57396620494226624, 11.00000000000000000 ) ) ;
#24896 = ORIENTED_EDGE ( 'NONE', *, *, #32515, .T. ) ;
#24897 = EDGE_CURVE ( 'NONE', #39323, #38584, #21255, .T. ) ;
#24898 = LINE ( 'NONE', #40134, #36596 ) ;
#24899 = AXIS2_PLACEMENT_3D ( 'NONE', #5063, #1621, #32708 ) ;
#24900 = CARTESIAN_POINT ( 'NONE',  ( -4.817371740575532080, 23.83900317890012843, 23.00000000000000000 ) ) ;
#24901 = CYLINDRICAL_SURFACE ( 'NONE', #214, 21.00000000000002842 ) ;
#24902 = CARTESIAN_POINT ( 'NONE',  ( 2.625031239634822100, 36.35909348746493919, -9.730352021840648291 ) ) ;
#24903 = LINE ( 'NONE', #37694, #28897 ) ;
#24904 = LINE ( 'NONE', #34646, #16923 ) ;
#24905 = CARTESIAN_POINT ( 'NONE',  ( 2.806807826039672715, 9.295007390093600108, 7.000000000000000000 ) ) ;
#24906 = DIRECTION ( 'NONE',  ( 0.9781476007338069101, 0.2079116908177532641, 0.000000000000000000 ) ) ;
#24907 = CARTESIAN_POINT ( 'NONE',  ( -1.204925152852743375, 12.02153850147729486, 10.50000000000000000 ) ) ;
#24908 = LINE ( 'NONE', #9476, #39191 ) ;
#24909 = CARTESIAN_POINT ( 'NONE',  ( 15.04722313270411327, 27.70573751427465226, -6.401096178813311610 ) ) ;
#24910 = CARTESIAN_POINT ( 'NONE',  ( -10.14060191828654212, 25.26915018278947755, 10.50000000000000000 ) ) ;
#24911 = ORIENTED_EDGE ( 'NONE', *, *, #16815, .F. ) ;
#24913 = DIRECTION ( 'NONE',  ( 1.000000000000000000, 0.000000000000000000, 0.000000000000000000 ) ) ;
#24912 = CARTESIAN_POINT ( 'NONE',  ( -18.38703319206937081, 17.23187950328362916, -9.851216774087896866 ) ) ;
#24914 = CIRCLE ( 'NONE', #932, 0.5000000000000000000 ) ;
#24915 = CARTESIAN_POINT ( 'NONE',  ( 13.24038105676655341, 15.43301270189216190, 10.49999999999999822 ) ) ;
#24916 = EDGE_CURVE ( 'NONE', #23691, #16497, #26442, .T. ) ;
#24917 = CARTESIAN_POINT ( 'NONE',  ( 14.75481277935874935, -25.65575037643989376, -10.18041772782883214 ) ) ;
#24918 = CARTESIAN_POINT ( 'NONE',  ( -22.54724872518345080, -26.68010991916779062, -7.210959810203029896 ) ) ;
#24919 = CARTESIAN_POINT ( 'NONE',  ( 15.42079449665415680, 26.76609254708107244, -5.000000000000002665 ) ) ;
#24920 = CARTESIAN_POINT ( 'NONE',  ( 15.22764080799647068, 26.42222000209493160, -7.827247944502371269 ) ) ;
#24921 = B_SPLINE_SURFACE_WITH_KNOTS ( 'NONE', 1, 3, ( 
 ( #1446, #19526, #4084, #26223, #1048, #16896, #19937, #32124, #4290, #23178 ),
 ( #35576, #36379, #14641, #11597, #17705, #23983, #8346, #39415, #27033, #8543 ) ),
 .UNSPECIFIED., .F., .F., .F.,
 ( 2, 2 ),
 ( 4, 2, 2, 2, 4 ),
 ( 0.000000000000000000, 1.000000000000000000 ),
 ( -1.183199640139722675, -0.7905005584409985353, -0.3978014767422745068, -0.005102395043550450593, 0.3875966866551736056 ),
 .UNSPECIFIED. ) ;
#24922 = ORIENTED_EDGE ( 'NONE', *, *, #16084, .T. ) ;
#24923 = DIRECTION ( 'NONE',  ( -0.8090169943749426773, 0.5877852522924796874, 0.000000000000000000 ) ) ;
#24924 = PRODUCT_RELATED_PRODUCT_CATEGORY ( 'part', '', ( #939 ) ) ;
#24925 = CARTESIAN_POINT ( 'NONE',  ( -14.99825077041236909, -26.12718959772186267, -8.768476732925005734 ) ) ;
#24926 = CARTESIAN_POINT ( 'NONE',  ( -27.83556507003000391, -26.34944855520640061, 14.53008259253985379 ) ) ;
#24927 = CARTESIAN_POINT ( 'NONE',  ( -18.37535949686024495, -13.48922921807925590, -23.01936354672100293 ) ) ;
#24928 = CARTESIAN_POINT ( 'NONE',  ( -0.3658111510020998769, -23.95295762298067643, -11.88201142430637880 ) ) ;
#24929 = CARTESIAN_POINT ( 'NONE',  ( 11.19848097534155684, 17.17100607549662072, -30.00000000000000355 ) ) ;
#24930 = EDGE_CURVE ( 'NONE', #10849, #7392, #19304, .T. ) ;
#24931 = CARTESIAN_POINT ( 'NONE',  ( 21.72105953519021782, 10.88454294244725062, -10.38293942656555480 ) ) ;
#24932 = CARTESIAN_POINT ( 'NONE',  ( 8.633502029282041690, 11.46765470489692795, 9.500000000000000000 ) ) ;
#24933 = EDGE_CURVE ( 'NONE', #35208, #30083, #14102, .T. ) ;
#24934 = ORIENTED_EDGE ( 'NONE', *, *, #33963, .T. ) ;
#24935 = CARTESIAN_POINT ( 'NONE',  ( -21.03490419256541344, -2.515787243126888395, -25.94069391000374836 ) ) ;
#24936 = CARTESIAN_POINT ( 'NONE',  ( -11.11100267139899778, 25.58833710556205077, 19.66345542862528717 ) ) ;
#24937 = ORIENTED_EDGE ( 'NONE', *, *, #1727, .T. ) ;
#24938 = CARTESIAN_POINT ( 'NONE',  ( 5.440908595777814050, 35.94977745735560859, 7.500000000000000888 ) ) ;
#24939 = CARTESIAN_POINT ( 'NONE',  ( -11.94134295108997890, 16.18301270189233421, 7.000000000000000000 ) ) ;
#24940 = CARTESIAN_POINT ( 'NONE',  ( -30.22364946210556624, 0.6259246664836076723, -5.946350832945448417 ) ) ;
#24941 = CARTESIAN_POINT ( 'NONE',  ( 23.14110463828941278, -7.760064457001075056, -20.81805854442341541 ) ) ;
#24942 = CARTESIAN_POINT ( 'NONE',  ( 28.15028875895061944, -26.91874057850925439, 12.73282698324841888 ) ) ;
#24943 = ORIENTED_EDGE ( 'NONE', *, *, #5045, .T. ) ;
#24944 = ADVANCED_FACE ( 'NONE', ( #11265 ), #4967, .T. ) ;
#24945 = CARTESIAN_POINT ( 'NONE',  ( 0.01803229776516698107, 30.37627742347970283, 6.000000000000000000 ) ) ;
#24946 = VERTEX_POINT ( 'NONE', #33418 ) ;
#24947 = EDGE_CURVE ( 'NONE', #26077, #10398, #38893, .T. ) ;
#24948 = DIRECTION ( 'NONE',  ( 0.000000000000000000, 0.000000000000000000, 1.000000000000000000 ) ) ;
#24949 = DIRECTION ( 'NONE',  ( 0.000000000000000000, 0.000000000000000000, 1.000000000000000000 ) ) ;
#24950 = CIRCLE ( 'NONE', #30151, 1.000000000000000888 ) ;
#24951 = DIRECTION ( 'NONE',  ( 0.000000000000000000, 0.000000000000000000, 1.000000000000000000 ) ) ;
#24952 = VERTEX_POINT ( 'NONE', #14713 ) ;
#24953 = CARTESIAN_POINT ( 'NONE',  ( -3.020371057517535984, 37.41995014423672217, -7.977523484556464872 ) ) ;
#24954 = CARTESIAN_POINT ( 'NONE',  ( 3.863783140547853712E-14, -86.77689918168233874, 0.000000000000000000 ) ) ;
#24955 = DIRECTION ( 'NONE',  ( -0.7071067811865546782, 0.000000000000000000, -0.7071067811865403563 ) ) ;
#24956 = CIRCLE ( 'NONE', #26258, 1.000000000000000000 ) ;
#24957 = CARTESIAN_POINT ( 'NONE',  ( 6.557822374958316658, 35.99981354310111215, 11.00000000000000000 ) ) ;
#24958 = PLANE ( 'NONE',  #20989 ) ;
#24959 = CARTESIAN_POINT ( 'NONE',  ( 8.712215903382341864, 20.44729472759973632, -23.46250027292118290 ) ) ;
#24960 = VECTOR ( 'NONE', #11219, 1000.000000000000000 ) ;
#24961 = VERTEX_POINT ( 'NONE', #23851 ) ;
#24962 = CARTESIAN_POINT ( 'NONE',  ( -20.62288446763035665, 13.61555273158426083, -7.427349022565545411 ) ) ;
#24963 = CARTESIAN_POINT ( 'NONE',  ( 15.33540832684242616, 35.51988609203954894, 23.00000000000000711 ) ) ;
#24964 = CARTESIAN_POINT ( 'NONE',  ( 15.68314276670921359, -26.79173994879206688, -5.000000000000000888 ) ) ;
#24965 = DIRECTION ( 'NONE',  ( -0.000000000000000000, -0.000000000000000000, -1.000000000000000000 ) ) ;
#24966 = CARTESIAN_POINT ( 'NONE',  ( 14.26301124034561774, 24.54581302918253627, -12.54423936124191741 ) ) ;
#24967 = CARTESIAN_POINT ( 'NONE',  ( -26.31271763591404422, -28.25584584496042240, -5.000000000000000888 ) ) ;
#24968 = EDGE_CURVE ( 'NONE', #37600, #31884, #26636, .T. ) ;
#24969 = CARTESIAN_POINT ( 'NONE',  ( 11.07315816304239320, 31.12468366354660532, 10.50000000000000000 ) ) ;
#24970 = CARTESIAN_POINT ( 'NONE',  ( -15.28113052511585224, 26.56228617015612414, -7.356869252458130504 ) ) ;
#24971 = CARTESIAN_POINT ( 'NONE',  ( -14.67729291545832560, -14.63692594569341310, -27.79627455608592967 ) ) ;
#24972 = CARTESIAN_POINT ( 'NONE',  ( 8.752986035078182070, -18.86042647000214956, -26.90452173386816526 ) ) ;
#24973 = CARTESIAN_POINT ( 'NONE',  ( 11.05718465110185988, 17.26235906992462787, -30.00000000000000000 ) ) ;
#24974 = CARTESIAN_POINT ( 'NONE',  ( 31.64736106748093647, -21.41673248936808349, -6.278375262888240549 ) ) ;
#24975 = DIRECTION ( 'NONE',  ( 0.000000000000000000, 0.000000000000000000, 1.000000000000000000 ) ) ;
#24976 = VERTEX_POINT ( 'NONE', #20813 ) ;
#24977 = CARTESIAN_POINT ( 'NONE',  ( -8.406664792321896229, 25.38477432831364311, -17.87301269380117930 ) ) ;
#24978 = DIRECTION ( 'NONE',  ( 0.000000000000000000, 0.000000000000000000, 1.000000000000000000 ) ) ;
#24979 = DIRECTION ( 'NONE',  ( 0.000000000000000000, 0.000000000000000000, 1.000000000000000000 ) ) ;
#24980 = AXIS2_PLACEMENT_3D ( 'NONE', #28468, #643, #22566 ) ;
#24981 = PLANE ( 'NONE',  #39024 ) ;
#24982 = EDGE_LOOP ( 'NONE', ( #10791, #24392 ) ) ;
#24983 = CARTESIAN_POINT ( 'NONE',  ( 21.27582338407567519, 0.7799646396183672614, -25.01502835885500176 ) ) ;
#24984 = CARTESIAN_POINT ( 'NONE',  ( -14.21391437420826165, 30.04769070240181250, -4.999999999999998224 ) ) ;
#24985 = CARTESIAN_POINT ( 'NONE',  ( -5.644276917315533382, 36.40655018617698602, 7.000000000000000000 ) ) ;
#24986 = ORIENTED_EDGE ( 'NONE', *, *, #10015, .F. ) ;
#24987 = VECTOR ( 'NONE', #20834, 1000.000000000000000 ) ;
#24988 = CARTESIAN_POINT ( 'NONE',  ( -20.69269121772957121, 0.8588170339218694771, -27.44912421251707713 ) ) ;
#24989 = CARTESIAN_POINT ( 'NONE',  ( -9.331903152615899089, 11.35703883385581037, 10.50000000000000533 ) ) ;
#24990 = ORIENTED_EDGE ( 'NONE', *, *, #26697, .T. ) ;
#24991 = CARTESIAN_POINT ( 'NONE',  ( 33.82615122060476409, -6.056122843722836713, -8.538783554659925557 ) ) ;
#24992 = AXIS2_PLACEMENT_3D ( 'NONE', #23960, #2428, #5467 ) ;
#24993 = CIRCLE ( 'NONE', #20538, 16.00000000000000000 ) ;
#24994 = VERTEX_POINT ( 'NONE', #17171 ) ;
#24995 = CARTESIAN_POINT ( 'NONE',  ( -7.508063977623400831, 38.75471409550113577, 12.73282698324837980 ) ) ;
#24996 = DIRECTION ( 'NONE',  ( -0.6691306063588671194, -0.7431448254773862505, 0.000000000000000000 ) ) ;
#24997 = CARTESIAN_POINT ( 'NONE',  ( -1.160189012974344180, 37.45561938550757475, 7.203056206335832101 ) ) ;
#24998 = ADVANCED_FACE ( 'NONE', ( #11069 ), #26498, .F. ) ;
#24999 = CARTESIAN_POINT ( 'NONE',  ( -8.768078002823385120, 24.93711404285670596, 20.50957957746029692 ) ) ;
#25000 = PLANE ( 'NONE',  #33074 ) ;
#25001 = ORIENTED_EDGE ( 'NONE', *, *, #31603, .F. ) ;
#25002 = CARTESIAN_POINT ( 'NONE',  ( 3.503793317224327630, 8.420815634768672453, 11.00000000000000355 ) ) ;
#25003 = CARTESIAN_POINT ( 'NONE',  ( -12.69445121025463763, 16.09979585365689658, -29.99999999999999289 ) ) ;
#25004 = DIRECTION ( 'NONE',  ( 0.000000000000000000, 0.000000000000000000, 1.000000000000000000 ) ) ;
#25005 = CARTESIAN_POINT ( 'NONE',  ( -2.587667106213709101, 35.31811204475769728, 6.000000000000000000 ) ) ;
#25006 = CARTESIAN_POINT ( 'NONE',  ( 7.569476015651482648, 29.31452674637723277, -14.85894962403729203 ) ) ;
#25007 = CARTESIAN_POINT ( 'NONE',  ( 13.87647862417395572, -21.94196052813751052, -17.25938925699875881 ) ) ;
#25008 = DIRECTION ( 'NONE',  ( 1.000000000000000000, 0.000000000000000000, 0.000000000000000000 ) ) ;
#25009 = DIRECTION ( 'NONE',  ( 0.1045284632676436176, -0.9945218953682742891, 0.000000000000000000 ) ) ;
#25010 = EDGE_CURVE ( 'NONE', #21446, #23552, #39489, .T. ) ;
#25011 = EDGE_LOOP ( 'NONE', ( #10098, #2831, #27142, #15319 ) ) ;
#25012 = VECTOR ( 'NONE', #16159, 1000.000000000000114 ) ;
#25013 = CARTESIAN_POINT ( 'NONE',  ( -11.20417644663015366, 17.31670387387610432, -28.08716411289236703 ) ) ;
#25014 = AXIS2_PLACEMENT_3D ( 'NONE', #22973, #29677, #35376 ) ;
#25015 = CARTESIAN_POINT ( 'NONE',  ( -31.14237565978616118, -19.77424633423363787, 17.92354375535212796 ) ) ;
#25016 = CARTESIAN_POINT ( 'NONE',  ( 12.90216916962276983, -23.08619710550532744, -15.45772932541511580 ) ) ;
#25017 = EDGE_CURVE ( 'NONE', #11791, #15766, #18052, .T. ) ;
#25018 = CARTESIAN_POINT ( 'NONE',  ( -4.458872323573595864, 26.51478363815348160, 6.000000000000000000 ) ) ;
#25019 = ORIENTED_EDGE ( 'NONE', *, *, #36090, .T. ) ;
#25020 = ORIENTED_EDGE ( 'NONE', *, *, #36452, .T. ) ;
#25021 = CARTESIAN_POINT ( 'NONE',  ( -12.65668046281904502, 25.53506749916461871, -14.26639179336292784 ) ) ;
#25022 = CARTESIAN_POINT ( 'NONE',  ( -11.63144283470464480, -16.96580988189544570, -28.62035570873908341 ) ) ;
#25023 = FACE_BOUND ( 'NONE', #15660, .T. ) ;
#25024 = ORIENTED_EDGE ( 'NONE', *, *, #12633, .F. ) ;
#25025 = EDGE_CURVE ( 'NONE', #13640, #15240, #38156, .T. ) ;
#25026 = CARTESIAN_POINT ( 'NONE',  ( -31.89533340862117683, -9.891971453653612301, -12.04687614664414674 ) ) ;
#25027 = CARTESIAN_POINT ( 'NONE',  ( -10.73556218567333254, -20.01456250315406393, -21.62972654522360827 ) ) ;
#25028 = CARTESIAN_POINT ( 'NONE',  ( 0.5000000000000000000, 37.44611345180490503, 10.76099332938163755 ) ) ;
#25029 = ORIENTED_EDGE ( 'NONE', *, *, #13699, .T. ) ;
#25030 = CARTESIAN_POINT ( 'NONE',  ( 20.94835144443074881, 1.007079124089848232, -26.24203246979738324 ) ) ;
#25031 = DIRECTION ( 'NONE',  ( 1.000000000000000000, 0.000000000000000000, 0.000000000000000000 ) ) ;
#25032 = DIRECTION ( 'NONE',  ( 1.000000000000000000, 0.000000000000000000, 0.000000000000000000 ) ) ;
#25033 = ORIENTED_EDGE ( 'NONE', *, *, #33755, .F. ) ;
#25034 = CARTESIAN_POINT ( 'NONE',  ( -20.69701185487514294, 0.7957416167526897288, -27.44504335574468001 ) ) ;
#25035 = ORIENTED_EDGE ( 'NONE', *, *, #290, .T. ) ;
#25036 = CARTESIAN_POINT ( 'NONE',  ( 32.28014819601976626, -2.247453943413153077, -7.746584525066519511 ) ) ;
#25037 = CARTESIAN_POINT ( 'NONE',  ( 18.33518551373228789, -9.195211339103170900, -30.00000000000004263 ) ) ;
#25038 = CARTESIAN_POINT ( 'NONE',  ( 34.68832217153572373, -7.625465254387286507, 16.87380292611443267 ) ) ;
#25039 = ORIENTED_EDGE ( 'NONE', *, *, #21909, .T. ) ;
#25040 = CARTESIAN_POINT ( 'NONE',  ( -26.05480634030368137, 4.388949531393018688, -10.28550515634381668 ) ) ;
#25041 = VECTOR ( 'NONE', #35165, 1000.000000000000114 ) ;
#25042 = EDGE_CURVE ( 'NONE', #14313, #6492, #30152, .T. ) ;
#25043 = LINE ( 'NONE', #16300, #31214 ) ;
#25044 = ADVANCED_FACE ( 'NONE', ( #26699 ), #8964, .T. ) ;
#25045 = CARTESIAN_POINT ( 'NONE',  ( 3.833852081710590110, 25.75497152300995296, 21.00000000000000355 ) ) ;
#25046 = AXIS2_PLACEMENT_3D ( 'NONE', #4828, #33079, #5229 ) ;
#25047 = VECTOR ( 'NONE', #30437, 1000.000000000000114 ) ;
#25048 = DIRECTION ( 'NONE',  ( 1.000000000000000000, 0.000000000000000000, 0.000000000000000000 ) ) ;
#25049 = VECTOR ( 'NONE', #24164, 1000.000000000000114 ) ;
#25050 = CYLINDRICAL_SURFACE ( 'NONE', #11731, 0.5000000000000000000 ) ;
#25051 = FACE_BOUND ( 'NONE', #1358, .T. ) ;
#25052 = CARTESIAN_POINT ( 'NONE',  ( -16.72075857324140102, 7.444561356925720297, 7.000000000000000000 ) ) ;
#25053 = CARTESIAN_POINT ( 'NONE',  ( -23.47028999752262735, 7.894751856600318973, -10.85062483233681974 ) ) ;
#25054 = CARTESIAN_POINT ( 'NONE',  ( 0.5000000000000002220, 36.50000000000000711, 10.00000000000000000 ) ) ;
#25055 = DIRECTION ( 'NONE',  ( 0.6691306063588670083, 0.7431448254773863615, 0.000000000000000000 ) ) ;
#25056 = CARTESIAN_POINT ( 'NONE',  ( 17.36693989509100788, -19.17194112829468366, -18.88888385720245822 ) ) ;
#25057 = CARTESIAN_POINT ( 'NONE',  ( -11.89031881743725805, 33.20608791387860492, 13.00000000000000178 ) ) ;
#25058 = EDGE_CURVE ( 'NONE', #33648, #5046, #27112, .T. ) ;
#25059 = CARTESIAN_POINT ( 'NONE',  ( 12.25371331340743097, 20.67270376835447365, -19.46752873204117051 ) ) ;
#25060 = ORIENTED_EDGE ( 'NONE', *, *, #34499, .F. ) ;
#25061 = CARTESIAN_POINT ( 'NONE',  ( -14.53679685137945832, 21.79695616867457630, -14.57185096994714080 ) ) ;
#25062 = CARTESIAN_POINT ( 'NONE',  ( -26.64268929643286299, -15.38216383723055714, 20.69868183039780973 ) ) ;
#25063 = EDGE_CURVE ( 'NONE', #38335, #37600, #3125, .T. ) ;
#25064 = CARTESIAN_POINT ( 'NONE',  ( -2.036571916123810055, 8.108948098542073879, 7.000000000000000000 ) ) ;
#25065 = CARTESIAN_POINT ( 'NONE',  ( 12.15864794129231186, 19.89114798110919580, -20.54594864371944141 ) ) ;
#25066 = ORIENTED_EDGE ( 'NONE', *, *, #18470, .F. ) ;
#25067 = FACE_OUTER_BOUND ( 'NONE', #5257, .T. ) ;
#25068 = ORIENTED_EDGE ( 'NONE', *, *, #39297, .F. ) ;
#25070 = CARTESIAN_POINT ( 'NONE',  ( 1.932616070714738177, 8.598021898908950078, 10.50000000000000000 ) ) ;
#25069 = CARTESIAN_POINT ( 'NONE',  ( -15.07291816638977622, 26.61547165230870959, -8.284995957625287843 ) ) ;
#25071 = CARTESIAN_POINT ( 'NONE',  ( -15.53477848226612679, -26.63013453484452597, -6.884701492020882441 ) ) ;
#25072 = DIRECTION ( 'NONE',  ( 1.000000000000000000, 0.000000000000000000, 0.000000000000000000 ) ) ;
#25073 = CIRCLE ( 'NONE', #1068, 0.5000000000000004441 ) ;
#25074 = ORIENTED_EDGE ( 'NONE', *, *, #4112, .T. ) ;
#25075 = CARTESIAN_POINT ( 'NONE',  ( -34.90754895111634681, -15.66705718490307753, -5.436414939066039231 ) ) ;
#25076 = CARTESIAN_POINT ( 'NONE',  ( -10.06357074363348580, -20.17046618015623238, -21.70867519228511000 ) ) ;
#25077 = CYLINDRICAL_SURFACE ( 'NONE', #15706, 0.5000000000000004441 ) ;
#25078 = CARTESIAN_POINT ( 'NONE',  ( 16.49060731112116684, 23.31193391774742807, -5.000000000000002665 ) ) ;
#25079 = ORIENTED_EDGE ( 'NONE', *, *, #30691, .F. ) ;
#25080 = CARTESIAN_POINT ( 'NONE',  ( 21.49663310311013120, 5.283455890831983304, -20.99229874812046504 ) ) ;
#25081 = VECTOR ( 'NONE', #33976, 1000.000000000000114 ) ;
#25082 = CARTESIAN_POINT ( 'NONE',  ( 1.871201846650637046, 31.30332840660451765, 13.00000000000000178 ) ) ;
#25083 = CARTESIAN_POINT ( 'NONE',  ( -13.30736835491669368, 15.59574623945408511, 10.49999999999999822 ) ) ;
#25084 = CARTESIAN_POINT ( 'NONE',  ( -15.52302998184525507, -20.83641103980755460, -18.06021460543220414 ) ) ;
#25085 = ORIENTED_EDGE ( 'NONE', *, *, #31935, .T. ) ;
#25086 = CARTESIAN_POINT ( 'NONE',  ( -20.50193171233730993, 0.1922071591807820723, -29.99999999999999645 ) ) ;
#25087 = CARTESIAN_POINT ( 'NONE',  ( 30.81151147059108908, -0.3616763097095250790, -7.812778536805358165 ) ) ;
#25088 = CARTESIAN_POINT ( 'NONE',  ( 27.09004689510926056, -14.60731774717147680, 20.69868183039781329 ) ) ;
#25089 = ORIENTED_EDGE ( 'NONE', *, *, #30545, .F. ) ;
#25090 = CARTESIAN_POINT ( 'NONE',  ( -35.36940577612494963, -20.42053594592268695, -14.51648065752878480 ) ) ;
#25091 = DIRECTION ( 'NONE',  ( 0.000000000000000000, 0.000000000000000000, 1.000000000000000000 ) ) ;
#25092 = EDGE_LOOP ( 'NONE', ( #1109, #11985, #9404, #27391 ) ) ;
#25093 = EDGE_CURVE ( 'NONE', #28064, #11050, #19983, .T. ) ;
#25094 = DIRECTION ( 'NONE',  ( 0.07391278520356926729, 0.7032331762534078656, -0.7071067811865435759 ) ) ;
#25095 = AXIS2_PLACEMENT_3D ( 'NONE', #12783, #29583, #19843 ) ;
#25096 = CIRCLE ( 'NONE', #30305, 0.5000000000000004441 ) ;
#25097 = DIRECTION ( 'NONE',  ( 1.000000000000000000, 0.000000000000000000, 0.000000000000000000 ) ) ;
#25098 = CARTESIAN_POINT ( 'NONE',  ( -2.140527761532693418, 7.619874298175171035, 7.000000000000000000 ) ) ;
#25099 = CARTESIAN_POINT ( 'NONE',  ( 0.8413128747587147460, 20.74004676862665519, -27.70638048767625605 ) ) ;
#25100 = FACE_OUTER_BOUND ( 'NONE', #33766, .T. ) ;
#25101 = DIRECTION ( 'NONE',  ( 1.000000000000000000, 0.000000000000000000, 0.000000000000000000 ) ) ;
#25102 = DIRECTION ( 'NONE',  ( 0.000000000000000000, 0.000000000000000000, 1.000000000000000000 ) ) ;
#25103 = B_SPLINE_CURVE_WITH_KNOTS ( 'NONE', 3,
 ( #22371, #13432, #31727, #25826, #22574, #1256 ),
 .UNSPECIFIED., .F., .F.,
 ( 4, 2, 4 ),
 ( 0.000000000000000000, 0.5000000000000000000, 1.000000000000000000 ),
 .UNSPECIFIED. ) ;
#25104 = DIRECTION ( 'NONE',  ( -0.8910065241883629028, 0.4539904997395564079, 3.261825160244155287E-15 ) ) ;
#25105 = DIRECTION ( 'NONE',  ( -1.000000000000000000, 0.000000000000000000, 0.000000000000000000 ) ) ;
#25106 = LINE ( 'NONE', #12910, #20358 ) ;
#25107 = CARTESIAN_POINT ( 'NONE',  ( 13.83999196091766848, 25.56421401852912112, -12.46077667759507790 ) ) ;
#25108 = AXIS2_PLACEMENT_3D ( 'NONE', #3963, #28948, #925 ) ;
#25109 = DIRECTION ( 'NONE',  ( -1.000000000000000000, 0.000000000000000000, 0.000000000000000000 ) ) ;
#25110 = EDGE_LOOP ( 'NONE', ( #23776, #2489, #38132, #2249, #31527, #31135 ) ) ;
#25112 = CARTESIAN_POINT ( 'NONE',  ( -8.410254037844435260, 17.06698729810786475, 10.50000000000000000 ) ) ;
#25111 = CARTESIAN_POINT ( 'NONE',  ( -14.95315193416318245, 14.07753665216654682, -28.83165291678060882 ) ) ;
#25113 = CARTESIAN_POINT ( 'NONE',  ( -75.15099915297791711, 43.38844959084113384, 3.000000000000000000 ) ) ;
#25114 = CARTESIAN_POINT ( 'NONE',  ( 9.675278753175428292, -18.44830207160445923, -26.83172255620764446 ) ) ;
#25115 = CARTESIAN_POINT ( 'NONE',  ( -21.63262549566270465, -25.67952849192365861, -9.885633078860415424 ) ) ;
#25116 = CARTESIAN_POINT ( 'NONE',  ( 15.41782702884244571, 26.77676039938714325, -5.000000000000000000 ) ) ;
#25117 = CARTESIAN_POINT ( 'NONE',  ( 14.92826937204305793, 25.82090953808645040, -9.707752144388164695 ) ) ;
#25118 = ORIENTED_EDGE ( 'NONE', *, *, #4151, .F. ) ;
#25119 = FACE_OUTER_BOUND ( 'NONE', #10586, .T. ) ;
#25120 = CARTESIAN_POINT ( 'NONE',  ( -15.39818770356525768, -26.71945962344603487, -5.474181265265219309 ) ) ;
#25121 = CARTESIAN_POINT ( 'NONE',  ( -37.24966284334341537, -10.92205745603902045, 13.32518128616676911 ) ) ;
#25122 = CARTESIAN_POINT ( 'NONE',  ( -16.15747483659607298, -12.61697622026560772, -29.22209380604542872 ) ) ;
#25123 = CARTESIAN_POINT ( 'NONE',  ( -2.594368725792287833, -24.77623966133340261, -5.966968964887910509 ) ) ;
#25124 = CARTESIAN_POINT ( 'NONE',  ( 15.11376219116451836, 24.32797801075062338, -10.67731718876905234 ) ) ;
#25125 = CARTESIAN_POINT ( 'NONE',  ( 19.97175965172673529, 9.167974992394606559, -20.10623141010908910 ) ) ;
#25126 = DIRECTION ( 'NONE',  ( 0.5000000000000039968, 0.8660254037844363761, 0.000000000000000000 ) ) ;
#25127 = EDGE_CURVE ( 'NONE', #13873, #5508, #24251, .T. ) ;
#25128 = ORIENTED_EDGE ( 'NONE', *, *, #35344, .F. ) ;
#25129 = CARTESIAN_POINT ( 'NONE',  ( -33.99706561663532511, -4.510256399178081743, -5.000000000000002665 ) ) ;
#25130 = VECTOR ( 'NONE', #6142, 1000.000000000000000 ) ;
#25131 = TOROIDAL_SURFACE ( 'NONE', #5669, 1.000000000000000000, 0.5000000000000000000 ) ;
#25132 = CARTESIAN_POINT ( 'NONE',  ( -21.05742987670793909, 12.15751280775709020, 16.87380292611441490 ) ) ;
#25133 = ORIENTED_EDGE ( 'NONE', *, *, #26546, .F. ) ;
#25134 = CARTESIAN_POINT ( 'NONE',  ( 19.48557158514988075, -11.24999999999998224, 6.000000000000000000 ) ) ;
#25135 = CARTESIAN_POINT ( 'NONE',  ( 23.43672666297240426, -8.137589884419345054, 23.00000000000000355 ) ) ;
#25136 = AXIS2_PLACEMENT_3D ( 'NONE', #19593, #31985, #16351 ) ;
#25137 = CARTESIAN_POINT ( 'NONE',  ( -21.64275424889105182, 1.072163566031019144, -23.89394571961734570 ) ) ;
#25138 = CARTESIAN_POINT ( 'NONE',  ( 33.31245343632154032, -12.22087107712299847, -10.20715524599960311 ) ) ;
#25140 = CIRCLE ( 'NONE', #29054, 0.5000000000000004441 ) ;
#25139 = CARTESIAN_POINT ( 'NONE',  ( 36.21549415350893497, -5.268335738863441975, 13.32518128616590225 ) ) ;
#25141 = EDGE_CURVE ( 'NONE', #22096, #10782, #30370, .T. ) ;
#25142 = VERTEX_POINT ( 'NONE', #30557 ) ;
#25143 = ORIENTED_EDGE ( 'NONE', *, *, #9740, .T. ) ;
#25144 = CARTESIAN_POINT ( 'NONE',  ( -9.343266739736645121, 17.68301270189229868, 11.00000000000000000 ) ) ;
#25145 = CARTESIAN_POINT ( 'NONE',  ( -14.97283171447380390, 21.48159823030330884, 7.000000000000000000 ) ) ;
#25146 = LINE ( 'NONE', #18464, #17529 ) ;
#25147 = ORIENTED_EDGE ( 'NONE', *, *, #3943, .F. ) ;
#25148 = EDGE_CURVE ( 'NONE', #25142, #6401, #4560, .T. ) ;
#25149 = CARTESIAN_POINT ( 'NONE',  ( -3.068187625016429276, 38.20266742920320269, -5.436115964257634658 ) ) ;
#25150 = CARTESIAN_POINT ( 'NONE',  ( -5.982165713378355676, 28.55918256678905820, 7.000000000000000000 ) ) ;
#25151 = CARTESIAN_POINT ( 'NONE',  ( -19.48557158514985588, -11.25000000000002309, 6.000000000000000000 ) ) ;
#25152 = ADVANCED_FACE ( 'NONE', ( #5956 ), #21792, .T. ) ;
#25153 = CIRCLE ( 'NONE', #3840, 0.4999999999999998890 ) ;
#25154 = DIRECTION ( 'NONE',  ( 0.6916548014802255118, 0.1470157664652010365, -0.7071067811865469066 ) ) ;
#25155 = DIRECTION ( 'NONE',  ( 1.000000000000000000, 0.000000000000000000, 0.000000000000000000 ) ) ;
#25156 = DIRECTION ( 'NONE',  ( 1.000000000000000000, 0.000000000000000000, 0.000000000000000000 ) ) ;
#25157 = AXIS2_PLACEMENT_3D ( 'NONE', #39820, #30888, #10 ) ;
#25158 = CARTESIAN_POINT ( 'NONE',  ( 8.094548601407083765, 18.84590462288236878, -29.99999999999999289 ) ) ;
#25159 = AXIS2_PLACEMENT_3D ( 'NONE', #12686, #37276, #22031 ) ;
#25160 = ORIENTED_EDGE ( 'NONE', *, *, #5935, .T. ) ;
#25161 = CARTESIAN_POINT ( 'NONE',  ( -20.35271757330227516, 13.41710386861673854, -9.887965968330341582 ) ) ;
#25162 = CARTESIAN_POINT ( 'NONE',  ( -2.166144593658632544, 42.50000000000004974, 11.00000000000000000 ) ) ;
#25163 = CARTESIAN_POINT ( 'NONE',  ( 11.95392418477062257, -21.48168688891967193, -18.44634885117927325 ) ) ;
#25164 = DIRECTION ( 'NONE',  ( 1.000000000000000000, 0.000000000000000000, 0.000000000000000000 ) ) ;
#25165 = CARTESIAN_POINT ( 'NONE',  ( 11.26454620336414791, 18.07348392246389324, -25.00831616619147724 ) ) ;
#25166 = AXIS2_PLACEMENT_3D ( 'NONE', #17064, #30252, #24145 ) ;
#25167 = CARTESIAN_POINT ( 'NONE',  ( -13.28992586503615669, -18.25382200079944539, -20.55760979252988463 ) ) ;
#25168 = CARTESIAN_POINT ( 'NONE',  ( -5.068835528549854530, 13.82204480395809476, 10.50000000000000533 ) ) ;
#25169 = VECTOR ( 'NONE', #20943, 999.9999999999998863 ) ;
#25170 = CARTESIAN_POINT ( 'NONE',  ( -24.08910206099691464, -25.46756753362905812, -8.938104685036856623 ) ) ;
#25171 = CARTESIAN_POINT ( 'NONE',  ( 12.85889123487801555, -25.78048515081998104, -8.316609656120787619 ) ) ;
#25172 = CARTESIAN_POINT ( 'NONE',  ( 13.32213502064756483, 22.03573321722581113, -16.46143111696509465 ) ) ;
#25173 = CARTESIAN_POINT ( 'NONE',  ( 19.24076220952862926, -13.86809943524113997, -21.86721313143632983 ) ) ;
#25174 = EDGE_CURVE ( 'NONE', #13016, #10646, #5074, .T. ) ;
#25175 = FACE_OUTER_BOUND ( 'NONE', #27394, .T. ) ;
#25176 = LINE ( 'NONE', #37368, #17031 ) ;
#25177 = ADVANCED_FACE ( 'NONE', ( #24845 ), #21596, .F. ) ;
#25178 = VERTEX_POINT ( 'NONE', #34000 ) ;
#25179 = CARTESIAN_POINT ( 'NONE',  ( -7.551239285968937232, 22.78181879830267675, -21.00978300683897615 ) ) ;
#25180 = DIRECTION ( 'NONE',  ( 0.9945218953682742891, 0.1045284632676437425, 0.000000000000000000 ) ) ;
#25181 = CARTESIAN_POINT ( 'NONE',  ( -13.63396663385394803, 16.24580510161721847, 7.000000000000000000 ) ) ;
#25182 = DIRECTION ( 'NONE',  ( 0.7431448254773862505, -0.6691306063588670083, -0.000000000000000000 ) ) ;
#25183 = ORIENTED_EDGE ( 'NONE', *, *, #36473, .F. ) ;
#25184 = CARTESIAN_POINT ( 'NONE',  ( 20.96668529434488448, 0.8362590005558052653, -26.22736366994790913 ) ) ;
#25185 = CARTESIAN_POINT ( 'NONE',  ( 1.229431105722923023, 20.49260818092372460, 6.000000000000000000 ) ) ;
#25186 = DIRECTION ( 'NONE',  ( -0.3090169943749573322, -0.9510565162951504226, 0.000000000000000000 ) ) ;
#25187 = ORIENTED_EDGE ( 'NONE', *, *, #12593, .F. ) ;
#25188 = CARTESIAN_POINT ( 'NONE',  ( -30.86332187973009056, -0.0005132856539961011327, -5.474190270091115806 ) ) ;
#25189 = CARTESIAN_POINT ( 'NONE',  ( -20.57926082973601822, -27.21289976943432265, -5.455544558421332013 ) ) ;
#25190 = VERTEX_POINT ( 'NONE', #40081 ) ;
#25191 = CARTESIAN_POINT ( 'NONE',  ( 20.42343116704461892, -4.183005399031937799, -27.14234199482063659 ) ) ;
#25192 = AXIS2_PLACEMENT_3D ( 'NONE', #21396, #10916, #38936 ) ;
#25193 = ORIENTED_EDGE ( 'NONE', *, *, #10162, .F. ) ;
#25194 = CARTESIAN_POINT ( 'NONE',  ( -15.69117760686815721, 30.83412033666087737, 13.32518128616588093 ) ) ;
#25195 = AXIS2_PLACEMENT_3D ( 'NONE', #2813, #18263, #9715 ) ;
#25196 = CARTESIAN_POINT ( 'NONE',  ( -3.211402178667006169, 32.38366924255629442, 6.000000000000000000 ) ) ;
#25197 = FACE_OUTER_BOUND ( 'NONE', #16531, .T. ) ;
#25198 = ADVANCED_FACE ( 'NONE', ( #18360 ), #32310, .T. ) ;
#25199 = CARTESIAN_POINT ( 'NONE',  ( 4.159699369156109938, 34.84843100105947400, 18.87996532025784902 ) ) ;
#25200 = VECTOR ( 'NONE', #17258, 1000.000000000000000 ) ;
#25201 = DIRECTION ( 'NONE',  ( -0.000000000000000000, -0.000000000000000000, -1.000000000000000000 ) ) ;
#25202 = ORIENTED_EDGE ( 'NONE', *, *, #6067, .T. ) ;
#25203 = CARTESIAN_POINT ( 'NONE',  ( -3.914034194965524183, 30.06176806842423943, 9.000000000000001776 ) ) ;
#25204 = CARTESIAN_POINT ( 'NONE',  ( -20.31755536841790288, -2.811235405436151247, -30.00000000000001066 ) ) ;
#25205 = CARTESIAN_POINT ( 'NONE',  ( 19.48557158514975285, -11.24999999999995737, 10.00000000000000000 ) ) ;
#25206 = FACE_OUTER_BOUND ( 'NONE', #5554, .T. ) ;
#25207 = CARTESIAN_POINT ( 'NONE',  ( 17.48494887651980534, 18.07252522714370002, -11.80118198379806316 ) ) ;
#25208 = CARTESIAN_POINT ( 'NONE',  ( 5.618065306669937975, 21.88280708645027772, -23.17586028251368546 ) ) ;
#25209 = CARTESIAN_POINT ( 'NONE',  ( 11.81349784526102908, -17.96894529079195379, -24.79472172074744307 ) ) ;
#25210 = CARTESIAN_POINT ( 'NONE',  ( 0.5415361484146482551, 27.50000000000004974, 20.99999999999999289 ) ) ;
#25211 = CARTESIAN_POINT ( 'NONE',  ( 9.363324537585983265, 32.27640801132196913, 9.500000000000000000 ) ) ;
#25212 = AXIS2_PLACEMENT_3D ( 'NONE', #16839, #1192, #32683 ) ;
#25213 = VERTEX_POINT ( 'NONE', #2914 ) ;
#25215 = VECTOR ( 'NONE', #20882, 999.9999999999998863 ) ;
#25214 = CARTESIAN_POINT ( 'NONE',  ( -10.99360060711668474, 17.30291464612033181, -29.34855223075900454 ) ) ;
#25216 = CARTESIAN_POINT ( 'NONE',  ( -33.56035593554165075, -14.08372035823108526, 17.92354375535250810 ) ) ;
#25217 = CARTESIAN_POINT ( 'NONE',  ( 15.12799067885430659, -26.57699633146447482, -6.417320784827945879 ) ) ;
#25218 = CYLINDRICAL_SURFACE ( 'NONE', #23742, 0.5000000000000007772 ) ;
#25219 = ADVANCED_FACE ( 'NONE', ( #12256 ), #27302, .T. ) ;
#25220 = ORIENTED_EDGE ( 'NONE', *, *, #33755, .T. ) ;
#25221 = ORIENTED_EDGE ( 'NONE', *, *, #1200, .F. ) ;
#25222 = CIRCLE ( 'NONE', #28466, 6.000000000000003553 ) ;
#25223 = CARTESIAN_POINT ( 'NONE',  ( -14.41188954600920447, 29.53590640632083719, -5.000000000000000000 ) ) ;
#25224 = CARTESIAN_POINT ( 'NONE',  ( -11.76462635582750593, -17.13989212898560410, -27.28828191877128972 ) ) ;
#25225 = FACE_BOUND ( 'NONE', #10954, .T. ) ;
#25226 = CARTESIAN_POINT ( 'NONE',  ( -23.24156206836136818, -7.249540115697041820, -20.84616574791856891 ) ) ;
#25227 = CARTESIAN_POINT ( 'NONE',  ( -9.609681352058309756, -18.47898454444922933, -26.83723954853537919 ) ) ;
#25228 = CARTESIAN_POINT ( 'NONE',  ( -5.082607396026893376, 23.58034083595207875, 6.000000000000000000 ) ) ;
#25229 = ORIENTED_EDGE ( 'NONE', *, *, #27179, .F. ) ;
#25230 = CARTESIAN_POINT ( 'NONE',  ( 30.64962079249725946, 0.2186612821100236415, -5.474121491177763588 ) ) ;
#25231 = CARTESIAN_POINT ( 'NONE',  ( 13.49038105676655164, 15.86602540378438064, 7.000000000000000000 ) ) ;
#25232 = CARTESIAN_POINT ( 'NONE',  ( 2.525645716490518389, 8.212903943950921715, 7.499999999999990230 ) ) ;
#25233 = ORIENTED_EDGE ( 'NONE', *, *, #17076, .F. ) ;
#25234 = CARTESIAN_POINT ( 'NONE',  ( -27.76379728900110777, 0.1559794775103171827, -13.51035586821201129 ) ) ;
#25235 = VERTEX_POINT ( 'NONE', #6156 ) ;
#25236 = CARTESIAN_POINT ( 'NONE',  ( 20.64647571109192370, -0.6209930936118700506, -28.00345359345995888 ) ) ;
#25237 = CARTESIAN_POINT ( 'NONE',  ( -11.48173768534023154, 32.16538668264431777, 10.49999999999999822 ) ) ;
#25238 = CARTESIAN_POINT ( 'NONE',  ( 30.17922767059609512, -0.7536324250923613910, 17.42190598798392998 ) ) ;
#25239 = ORIENTED_EDGE ( 'NONE', *, *, #17590, .F. ) ;
#25240 = CARTESIAN_POINT ( 'NONE',  ( 4.591666147298500533, 15.32946292166668556, 9.000000000000001776 ) ) ;
#25241 = EDGE_CURVE ( 'NONE', #10259, #24976, #18558, .T. ) ;
#25242 = CARTESIAN_POINT ( 'NONE',  ( 1.848241319495468993, 27.98666583367186078, 21.00000000000000355 ) ) ;
#25243 = VECTOR ( 'NONE', #29511, 1000.000000000000227 ) ;
#25244 = CIRCLE ( 'NONE', #33708, 1.000000000000000000 ) ;
#25245 = DIRECTION ( 'NONE',  ( 0.1045284632676564129, 0.9945218953682731788, 0.000000000000000000 ) ) ;
#25246 = ADVANCED_FACE ( 'NONE', ( #34395 ), #30948, .T. ) ;
#25247 = EDGE_CURVE ( 'NONE', #33201, #33096, #18707, .T. ) ;
#25248 = PLANE ( 'NONE',  #5231 ) ;
#25249 = B_SPLINE_SURFACE_WITH_KNOTS ( 'NONE', 1, 3, ( 
 ( #16032, #31671, #18146, #19272, #33785, #30330, #10137, #6478, #27279, #37570 ),
 ( #33586, #18883, #15834, #27471, #3437, #5739, #31471, #14890, #34523, #24227 ) ),
 .UNSPECIFIED., .F., .F., .F.,
 ( 2, 2 ),
 ( 4, 2, 2, 2, 4 ),
 ( 0.000000000000000000, 1.000000000000000000 ),
 ( 4.237807397716039759, 4.630506479414762566, 5.023205561113485373, 5.415904642812208181, 5.808603724510930100 ),
 .UNSPECIFIED. ) ;
#25250 = ADVANCED_FACE ( 'NONE', ( #12453 ), #31416, .F. ) ;
#25251 = FACE_BOUND ( 'NONE', #29174, .T. ) ;
#25252 = DIRECTION ( 'NONE',  ( 0.000000000000000000, 0.000000000000000000, 1.000000000000000000 ) ) ;
#25253 = CARTESIAN_POINT ( 'NONE',  ( -19.30609231752467991, 7.879336912585563013, -25.47724169212735390 ) ) ;
#25254 = CARTESIAN_POINT ( 'NONE',  ( 14.20597032484196376, -14.79219592438034780, -29.25104138637490436 ) ) ;
#25255 = CARTESIAN_POINT ( 'NONE',  ( 0.5000000000000003331, 36.00000000000000711, 7.000000000000000000 ) ) ;
#25256 = CARTESIAN_POINT ( 'NONE',  ( 10.89810581091218111, 17.51759729559895717, -28.06894606240402013 ) ) ;
#25257 = ORIENTED_EDGE ( 'NONE', *, *, #32788, .T. ) ;
#25258 = CARTESIAN_POINT ( 'NONE',  ( -12.82984808660655318, 16.00373636590108362, -29.38416646348882111 ) ) ;
#25259 = CARTESIAN_POINT ( 'NONE',  ( -19.19127776371468030, -19.55740820284875880, 20.69868183039799092 ) ) ;
#25260 = CARTESIAN_POINT ( 'NONE',  ( 10.26940745284089829, 33.04623494220481206, 10.49999999999999822 ) ) ;
#25261 = CARTESIAN_POINT ( 'NONE',  ( 15.44165670342503205, 26.69129292160669920, -5.000000000000000000 ) ) ;
#25262 = ORIENTED_EDGE ( 'NONE', *, *, #34900, .F. ) ;
#25263 = LINE ( 'NONE', #22017, #861 ) ;
#25264 = ADVANCED_FACE ( 'NONE', ( #32091 ), #26473, .T. ) ;
#25265 = ORIENTED_EDGE ( 'NONE', *, *, #22401, .F. ) ;
#25267 = CARTESIAN_POINT ( 'NONE',  ( 7.851720845715640884, 9.718492148735345282, 7.202682876670055023 ) ) ;
#25266 = CARTESIAN_POINT ( 'NONE',  ( -10.85292483170471023, 17.44571412242369490, -28.70057752128876771 ) ) ;
#25268 = EDGE_CURVE ( 'NONE', #28022, #8314, #29051, .T. ) ;
#25269 = CARTESIAN_POINT ( 'NONE',  ( -15.61601735593368012, -26.74911251005942603, -5.944523841747975546 ) ) ;
#25270 = DIRECTION ( 'NONE',  ( -0.9135454576426059736, -0.4067366430757887730, 0.000000000000000000 ) ) ;
#25271 = ADVANCED_FACE ( 'NONE', ( #14808 ), #34251, .T. ) ;
#25272 = AXIS2_PLACEMENT_3D ( 'NONE', #16772, #17386, #29761 ) ;
#25273 = VERTEX_POINT ( 'NONE', #23952 ) ;
#25274 = CARTESIAN_POINT ( 'NONE',  ( -19.01544318679556511, -9.256926599663669819, -26.26492384747328757 ) ) ;
#25275 = CARTESIAN_POINT ( 'NONE',  ( -14.02798880308901275, -26.11055631809762900, -7.834863257364764522 ) ) ;
#25276 = CARTESIAN_POINT ( 'NONE',  ( -13.94482798346716201, 26.50521816028930644, 7.499999999999993783 ) ) ;
#25277 = CARTESIAN_POINT ( 'NONE',  ( 12.50874981011069664, 16.57754095322059484, -26.94891225080305830 ) ) ;
#25278 = VERTEX_POINT ( 'NONE', #5460 ) ;
#25279 = CARTESIAN_POINT ( 'NONE',  ( 24.28730508192998983, 4.587782948896792057, -14.73921855142076076 ) ) ;
#25280 = DIRECTION ( 'NONE',  ( 0.000000000000000000, 0.000000000000000000, 1.000000000000000000 ) ) ;
#25281 = DIRECTION ( 'NONE',  ( 0.000000000000000000, 0.000000000000000000, -1.000000000000000000 ) ) ;
#25282 = DIRECTION ( 'NONE',  ( 1.000000000000000000, 0.000000000000000000, 0.000000000000000000 ) ) ;
#25283 = CIRCLE ( 'NONE', #7762, 16.00000000000001066 ) ;
#25284 = VERTEX_POINT ( 'NONE', #2225 ) ;
#25285 = CARTESIAN_POINT ( 'NONE',  ( -27.40511294215596649, -0.1367760914176404108, -14.43413953572169817 ) ) ;
#25286 = CARTESIAN_POINT ( 'NONE',  ( 20.62252632493563098, 0.6248223115394143656, -28.06621906308379266 ) ) ;
#25287 = CARTESIAN_POINT ( 'NONE',  ( 21.42135062927563993, -21.87239811599182460, 19.99202127657103745 ) ) ;
#25288 = ORIENTED_EDGE ( 'NONE', *, *, #6049, .F. ) ;
#25289 = CARTESIAN_POINT ( 'NONE',  ( -11.41987377193683528, -19.41918266173334828, -20.90349153980999475 ) ) ;
#25290 = ADVANCED_FACE ( 'NONE', ( #26391 ), #4856, .F. ) ;
#25291 = CARTESIAN_POINT ( 'NONE',  ( 14.98890121934609532, -28.67928442654220333, 2.999999999999999112 ) ) ;
#25292 = EDGE_CURVE ( 'NONE', #28965, #11507, #29241, .T. ) ;
#25293 = VERTEX_POINT ( 'NONE', #29441 ) ;
#25294 = CARTESIAN_POINT ( 'NONE',  ( 10.09922753093620962, -27.41777246569289517, -5.000000000000000000 ) ) ;
#25295 = B_SPLINE_CURVE_WITH_KNOTS ( 'NONE', 3,
 ( #14783, #36321, #24713, #18232, #33873, #12129 ),
 .UNSPECIFIED., .F., .F.,
 ( 4, 2, 4 ),
 ( 0.000000000000000000, 0.5000000000000000000, 1.000000000000000000 ),
 .UNSPECIFIED. ) ;
#25296 = AXIS2_PLACEMENT_3D ( 'NONE', #16472, #21606, #278 ) ;
#25297 = DIRECTION ( 'NONE',  ( 1.000000000000000000, 0.000000000000000000, 0.000000000000000000 ) ) ;
#25298 = CARTESIAN_POINT ( 'NONE',  ( 20.20214925878792656, 14.56229221523759598, -4.999999999999995559 ) ) ;
#25299 = CARTESIAN_POINT ( 'NONE',  ( 2.098354962282032776, 20.79632631842905610, -26.98459398919786523 ) ) ;
#25300 = CARTESIAN_POINT ( 'NONE',  ( 12.30736835487432579, 14.81698729810772619, 7.000000000000000000 ) ) ;
#25301 = DIRECTION ( 'NONE',  ( 0.2876062384759450752, -0.6459741880212618304, -0.7071067811865399122 ) ) ;
#25302 = FACE_OUTER_BOUND ( 'NONE', #22749, .T. ) ;
#25303 = AXIS2_PLACEMENT_3D ( 'NONE', #31394, #25483, #25690 ) ;
#25304 = FACE_OUTER_BOUND ( 'NONE', #35655, .T. ) ;
#25305 = CARTESIAN_POINT ( 'NONE',  ( -3.503793317224517700, 8.420815634768727520, 9.000000000000001776 ) ) ;
#25306 = CARTESIAN_POINT ( 'NONE',  ( 14.68376815913365085, 27.36567026352939891, -8.715261669753955331 ) ) ;
#25307 = CARTESIAN_POINT ( 'NONE',  ( -8.410254037844435260, 17.06698729810786475, 10.50000000000000178 ) ) ;
#25308 = ORIENTED_EDGE ( 'NONE', *, *, #15748, .T. ) ;
#25310 = DIRECTION ( 'NONE',  ( 0.000000000000000000, 0.000000000000000000, 1.000000000000000000 ) ) ;
#25309 = CARTESIAN_POINT ( 'NONE',  ( -15.66915680351796070, 13.81629364357497458, -25.43784811616387032 ) ) ;
#25311 = CARTESIAN_POINT ( 'NONE',  ( 12.88757880222261321, 15.63670317852378489, 10.99387789255783510 ) ) ;
#25312 = CARTESIAN_POINT ( 'NONE',  ( 10.51168368352045057, -19.58291515952883444, -22.73802084914789390 ) ) ;
#25313 = CARTESIAN_POINT ( 'NONE',  ( 6.688300058587269170, 16.47782454277055564, 12.00000000000000000 ) ) ;
#25314 = CARTESIAN_POINT ( 'NONE',  ( 11.30648189521332725, 18.04080162384157759, -25.01410076809225913 ) ) ;
#25315 = CARTESIAN_POINT ( 'NONE',  ( 15.41110799979362511, 26.80090896191098793, -5.000000000000000000 ) ) ;
#25316 = EDGE_LOOP ( 'NONE', ( #20380, #34114, #10995 ) ) ;
#25317 = CARTESIAN_POINT ( 'NONE',  ( -12.92003364848273783, -23.08707941010340647, -15.45656058803134059 ) ) ;
#25318 = CARTESIAN_POINT ( 'NONE',  ( -36.55626306615705090, -16.65168930787910284, 12.73282698324876350 ) ) ;
#25319 = AXIS2_PLACEMENT_3D ( 'NONE', #37545, #15806, #12161 ) ;
#25320 = CARTESIAN_POINT ( 'NONE',  ( -30.72590368136143724, -21.21574487496830841, -8.410142833198055001 ) ) ;
#25321 = CARTESIAN_POINT ( 'NONE',  ( -1.830947598378612096, -20.80176537255082891, -25.50661662362668736 ) ) ;
#25322 = CARTESIAN_POINT ( 'NONE',  ( 14.08529064057289482, 22.72790877343337712, -14.51632245905989649 ) ) ;
#25323 = ORIENTED_EDGE ( 'NONE', *, *, #24528, .F. ) ;
#25324 = CARTESIAN_POINT ( 'NONE',  ( 18.60021360422396342, 8.694919316221673355, -28.85921347423368388 ) ) ;
#25325 = CARTESIAN_POINT ( 'NONE',  ( 11.48173768534036121, 32.16538668264416145, 10.49999999999999822 ) ) ;
#25326 = CARTESIAN_POINT ( 'NONE',  ( 4.960307196185259393, 37.22510528292774268, 16.87380292611441845 ) ) ;
#25327 = ORIENTED_EDGE ( 'NONE', *, *, #26611, .F. ) ;
#25328 = CARTESIAN_POINT ( 'NONE',  ( -20.47084386718785609, -3.078924522425823707, -27.88626578634149666 ) ) ;
#25329 = CARTESIAN_POINT ( 'NONE',  ( -21.86831431663999936, 12.62567715743360530, 15.72805884748939498 ) ) ;
#25330 = ORIENTED_EDGE ( 'NONE', *, *, #31146, .T. ) ;
#25331 = CARTESIAN_POINT ( 'NONE',  ( 24.51396478725026640, -11.15767879383070138, 20.99999999999999645 ) ) ;
#25332 = LINE ( 'NONE', #9709, #31685 ) ;
#25333 = VECTOR ( 'NONE', #6310, 1000.000000000000000 ) ;
#25334 = CARTESIAN_POINT ( 'NONE',  ( -20.80015496576257661, 2.182957871452693599, -26.33707758174465496 ) ) ;
#25335 = CARTESIAN_POINT ( 'NONE',  ( 26.75366824387117148, -10.76373612552858638, -16.67183740961663929 ) ) ;
#25336 = CARTESIAN_POINT ( 'NONE',  ( 18.85757713438717786, -29.00601609346521670, 13.32518128616639785 ) ) ;
#25337 = VERTEX_POINT ( 'NONE', #33311 ) ;
#25338 = VERTEX_POINT ( 'NONE', #17272 ) ;
#25339 = CARTESIAN_POINT ( 'NONE',  ( -1.000000000000000000, 37.50000000000000711, 11.00000000000000000 ) ) ;
#25340 = CARTESIAN_POINT ( 'NONE',  ( 14.97283171447379146, 21.48159823030311344, 11.00000000000000000 ) ) ;
#25341 = AXIS2_PLACEMENT_3D ( 'NONE', #30561, #30358, #18362 ) ;
#25342 = DIRECTION ( 'NONE',  ( -1.000000000000000000, 0.000000000000000000, 0.000000000000000000 ) ) ;
#25343 = VERTEX_POINT ( 'NONE', #39586 ) ;
#25344 = CARTESIAN_POINT ( 'NONE',  ( -2.329603726064299885, 28.90242561963931678, -16.64147633399780446 ) ) ;
#25345 = VECTOR ( 'NONE', #8872, 999.9999999999998863 ) ;
#25346 = CARTESIAN_POINT ( 'NONE',  ( 8.118377661053333583, 10.47536095541699197, 11.00000000000000000 ) ) ;
#25347 = DIRECTION ( 'NONE',  ( -0.1045284632676436315, 0.9945218953682742891, 0.000000000000000000 ) ) ;
#25348 = DIRECTION ( 'NONE',  ( 0.1470157664652037011, 0.6916548014802281763, -0.7071067811865437980 ) ) ;
#25349 = DIRECTION ( 'NONE',  ( 0.000000000000000000, 0.000000000000000000, -1.000000000000000000 ) ) ;
#25350 = LINE ( 'NONE', #34507, #10625 ) ;
#25351 = CARTESIAN_POINT ( 'NONE',  ( 9.546848429036838724, 20.70351224251990274, -22.40024640956508151 ) ) ;
#25352 = ORIENTED_EDGE ( 'NONE', *, *, #159, .T. ) ;
#25353 = CARTESIAN_POINT ( 'NONE',  ( -18.43601137689102742, 10.05164828422247503, -24.41288531576839205 ) ) ;
#25354 = CARTESIAN_POINT ( 'NONE',  ( -7.064571727552472424, 31.45661825943146894, 12.00000000000000000 ) ) ;
#25355 = CARTESIAN_POINT ( 'NONE',  ( 13.43826639690882985, -23.62933372394671139, -14.47033993370646598 ) ) ;
#25356 = CARTESIAN_POINT ( 'NONE',  ( -9.303655249773278513, 10.73386218874833808, 7.000000000000000000 ) ) ;
#25357 = VECTOR ( 'NONE', #28800, 1000.000000000000000 ) ;
#25358 = CARTESIAN_POINT ( 'NONE',  ( 14.50167871676907616, 25.05847836359596315, -11.59245320002316504 ) ) ;
#25359 = CARTESIAN_POINT ( 'NONE',  ( 31.47283671532267846, -25.12609584734865464, -14.45070082761209207 ) ) ;
#25360 = CARTESIAN_POINT ( 'NONE',  ( 0.5000000000000005551, 33.00000000000000000, 10.50000000000000000 ) ) ;
#25361 = CARTESIAN_POINT ( 'NONE',  ( -24.69306225852445991, -24.64882393665288518, -9.807970858657039770 ) ) ;
#25362 = CARTESIAN_POINT ( 'NONE',  ( 6.225823723043348856, -25.00732421141256978, -6.924410079875567448 ) ) ;
#25363 = CARTESIAN_POINT ( 'NONE',  ( 14.10414194694077494, 23.76207731977601156, -13.52159713385365869 ) ) ;
#25364 = CARTESIAN_POINT ( 'NONE',  ( 30.82101031815450654, -22.25462399755607379, -6.702141387976242370 ) ) ;
#25365 = EDGE_CURVE ( 'NONE', #12173, #33298, #33625, .T. ) ;
#25366 = CARTESIAN_POINT ( 'NONE',  ( 13.52529089031629184, 27.94609563178149614, 10.49999999999999822 ) ) ;
#25367 = DIRECTION ( 'NONE',  ( -0.000000000000000000, -0.000000000000000000, -1.000000000000000000 ) ) ;
#25368 = EDGE_LOOP ( 'NONE', ( #28081, #20003, #28453 ) ) ;
#25369 = CARTESIAN_POINT ( 'NONE',  ( -5.884614315209530488, 19.64670892508010169, -29.25345033631867153 ) ) ;
#25370 = FACE_OUTER_BOUND ( 'NONE', #18411, .T. ) ;
#25371 = CARTESIAN_POINT ( 'NONE',  ( 14.97009266215792067, 21.42933399866928923, 10.49999999999999112 ) ) ;
#25372 = ORIENTED_EDGE ( 'NONE', *, *, #18248, .F. ) ;
#25373 = CARTESIAN_POINT ( 'NONE',  ( 23.33050994933525146, 0.5154748466008040042, -20.53702464707256681 ) ) ;
#25374 = EDGE_CURVE ( 'NONE', #26679, #2909, #14610, .T. ) ;
#25375 = AXIS2_PLACEMENT_3D ( 'NONE', #1066, #20366, #26039 ) ;
#25376 = CARTESIAN_POINT ( 'NONE',  ( 4.096822963000107620, 8.035697679810645866, 10.50000000000000000 ) ) ;
#25377 = DIRECTION ( 'NONE',  ( 0.9945218953682742891, 0.1045284632676437564, 0.000000000000000000 ) ) ;
#25378 = EDGE_CURVE ( 'NONE', #9588, #40031, #4404, .T. ) ;
#25379 = ORIENTED_EDGE ( 'NONE', *, *, #35032, .F. ) ;
#25380 = CARTESIAN_POINT ( 'NONE',  ( -29.77291926438935477, 0.07581751844958646569, -9.709798205980805008 ) ) ;
#25381 = CARTESIAN_POINT ( 'NONE',  ( -11.44473057578096942, 31.45924896672619298, 7.500000000000004441 ) ) ;
#25382 = ORIENTED_EDGE ( 'NONE', *, *, #14385, .F. ) ;
#25383 = CARTESIAN_POINT ( 'NONE',  ( 34.70961424076313051, -8.320133917892743369, -7.618081809658795223 ) ) ;
#25384 = ORIENTED_EDGE ( 'NONE', *, *, #23839, .T. ) ;
#25385 = CARTESIAN_POINT ( 'NONE',  ( -15.93459161340889096, 30.96344742789386828, 12.14047268033069393 ) ) ;
#25386 = DIRECTION ( 'NONE',  ( 0.000000000000000000, 0.000000000000000000, 1.000000000000000000 ) ) ;
#25387 = DIRECTION ( 'NONE',  ( -0.000000000000000000, -0.000000000000000000, 1.000000000000000000 ) ) ;
#25388 = CARTESIAN_POINT ( 'NONE',  ( -1.072992850107295468E-13, 35.53022820328502718, 18.87996532025784546 ) ) ;
#25389 = CARTESIAN_POINT ( 'NONE',  ( -4.984135866956332706, 36.15314577889358105, 9.500000000000000000 ) ) ;
#25390 = ORIENTED_EDGE ( 'NONE', *, *, #35971, .T. ) ;
#25391 = CARTESIAN_POINT ( 'NONE',  ( 3.585007771387210607, 8.038731668389077711, 10.82238861112335471 ) ) ;
#25392 = CARTESIAN_POINT ( 'NONE',  ( -20.30900398262955520, 3.084420529719719362, -30.00000000000000000 ) ) ;
#25393 = EDGE_CURVE ( 'NONE', #28064, #11564, #14797, .T. ) ;
#25394 = CYLINDRICAL_SURFACE ( 'NONE', #22758, 1.000000000000000000 ) ;
#25395 = EDGE_CURVE ( 'NONE', #8749, #36443, #5995, .T. ) ;
#25396 = DIRECTION ( 'NONE',  ( -0.000000000000000000, -0.000000000000000000, -1.000000000000000000 ) ) ;
#25397 = CARTESIAN_POINT ( 'NONE',  ( 15.58421666608182399, 16.80577185948362029, -18.86466076104356659 ) ) ;
#25398 = CARTESIAN_POINT ( 'NONE',  ( 6.528576035962029955, 25.38036280295423808, -18.79159262674204456 ) ) ;
#25399 = VECTOR ( 'NONE', #19912, 1000.000000000000114 ) ;
#25400 = ORIENTED_EDGE ( 'NONE', *, *, #6887, .T. ) ;
#25401 = AXIS2_PLACEMENT_3D ( 'NONE', #15608, #19052, #28391 ) ;
#25402 = CARTESIAN_POINT ( 'NONE',  ( 16.24958219909836288, -26.89404583347094047, -5.938197498648205119 ) ) ;
#25403 = CARTESIAN_POINT ( 'NONE',  ( 4.817371740575539185, 23.83900317890011422, 20.99999999999999645 ) ) ;
#25404 = CARTESIAN_POINT ( 'NONE',  ( -4.724378136954611840, 12.76962061027129458, 13.00000000000000178 ) ) ;
#25405 = VERTEX_POINT ( 'NONE', #11563 ) ;
#25406 = CARTESIAN_POINT ( 'NONE',  ( -11.05465679327823558, 17.41536169098398545, -28.07828314278957293 ) ) ;
#25407 = CARTESIAN_POINT ( 'NONE',  ( -18.95257105546425791, -26.31232633481670646, 17.42190598798432077 ) ) ;
#25408 = CARTESIAN_POINT ( 'NONE',  ( 9.496368407746681228, -18.31046244359924202, -28.08151151955017255 ) ) ;
#25409 = CIRCLE ( 'NONE', #7902, 1.000000000000000000 ) ;
#25410 = CARTESIAN_POINT ( 'NONE',  ( 3.118671991557230516, 37.17221401100731981, 13.00000000000000178 ) ) ;
#25411 = ORIENTED_EDGE ( 'NONE', *, *, #35765, .F. ) ;
#25412 = VERTEX_POINT ( 'NONE', #29642 ) ;
#25413 = CARTESIAN_POINT ( 'NONE',  ( -8.333876625047521358, 18.93681600531247611, -27.92366777036197334 ) ) ;
#25414 = CARTESIAN_POINT ( 'NONE',  ( -6.407695755496608747, 35.66262363504867494, 10.99999999999999467 ) ) ;
#25415 = EDGE_CURVE ( 'NONE', #16860, #7168, #26596, .T. ) ;
#25416 = FACE_BOUND ( 'NONE', #27688, .T. ) ;
#25417 = CARTESIAN_POINT ( 'NONE',  ( -35.24538222971869317, -9.860299811780501855, -6.734244107179631733 ) ) ;
#25418 = CARTESIAN_POINT ( 'NONE',  ( -15.26244400023809078, -26.61077467321880974, -6.417168005406195697 ) ) ;
#25419 = LINE ( 'NONE', #19329, #5363 ) ;
#25420 = VERTEX_POINT ( 'NONE', #39186 ) ;
#25421 = CARTESIAN_POINT ( 'NONE',  ( 23.88555579540136620, 0.6173852234973284947, -19.51149964275768411 ) ) ;
#25422 = CARTESIAN_POINT ( 'NONE',  ( 14.94435605704140357, 25.81679485013957631, -9.707589803872810563 ) ) ;
#25423 = DIRECTION ( 'NONE',  ( 0.000000000000000000, 0.000000000000000000, 1.000000000000000000 ) ) ;
#25424 = VERTEX_POINT ( 'NONE', #14408 ) ;
#25425 = CARTESIAN_POINT ( 'NONE',  ( -21.28292253093711750, 0.7291719054457980187, -25.00947294987627600 ) ) ;
#25426 = ORIENTED_EDGE ( 'NONE', *, *, #11912, .F. ) ;
#25427 = CARTESIAN_POINT ( 'NONE',  ( 32.75437695154221274, -2.309567439508531717, -5.000000000000000000 ) ) ;
#25428 = CARTESIAN_POINT ( 'NONE',  ( -2.006248926576237324, -20.44716014466324694, -30.00000000000000711 ) ) ;
#25429 = CARTESIAN_POINT ( 'NONE',  ( 32.48135758214254309, -20.75321993593874126, 16.30093088680188984 ) ) ;
#25430 = ORIENTED_EDGE ( 'NONE', *, *, #162, .F. ) ;
#25431 = CARTESIAN_POINT ( 'NONE',  ( 7.559505275947156377, 25.28115294937476065, 12.00000000000000000 ) ) ;
#25432 = CARTESIAN_POINT ( 'NONE',  ( -4.002244506128481483, 26.73020382270282269, 21.00000000000009237 ) ) ;
#25433 = DIRECTION ( 'NONE',  ( -0.000000000000000000, -0.000000000000000000, -1.000000000000000000 ) ) ;
#25434 = ADVANCED_FACE ( 'NONE', ( #2421 ), #11162, .F. ) ;
#25435 = CIRCLE ( 'NONE', #16348, 15.00000000000000000 ) ;
#25436 = CARTESIAN_POINT ( 'NONE',  ( -7.611215932167762155, 18.68301270189229513, 9.000000000000001776 ) ) ;
#25437 = EDGE_CURVE ( 'NONE', #1824, #4212, #35577, .T. ) ;
#25438 = FACE_BOUND ( 'NONE', #4362, .T. ) ;
#25439 = CARTESIAN_POINT ( 'NONE',  ( 17.28285333400761914, 27.30382183500914550, 12.14047268033097460 ) ) ;
#25440 = CARTESIAN_POINT ( 'NONE',  ( -22.74231906068476050, 9.811850412294511159, -8.402255488763186619 ) ) ;
#25441 = CARTESIAN_POINT ( 'NONE',  ( 21.92413472738710212, -26.98779261574284760, -6.338459772264864789 ) ) ;
#25442 = CARTESIAN_POINT ( 'NONE',  ( -3.295881626406750087, 9.398963235502531433, 9.500000000000000000 ) ) ;
#25443 = CARTESIAN_POINT ( 'NONE',  ( 15.34417538557263683, 26.94339626938088372, -5.944057201105769295 ) ) ;
#25444 = EDGE_LOOP ( 'NONE', ( #37918, #7042, #36045, #7577 ) ) ;
#25445 = CARTESIAN_POINT ( 'NONE',  ( -11.71642904664754070, 16.82516707186347915, -29.36357973296176027 ) ) ;
#25446 = AXIS2_PLACEMENT_3D ( 'NONE', #35408, #38654, #29910 ) ;
#25447 = CARTESIAN_POINT ( 'NONE',  ( -18.04765032505036970, -21.12132759291239381, 20.25080042701569027 ) ) ;
#25448 = CARTESIAN_POINT ( 'NONE',  ( -3.503793317224518145, 8.420815634768723967, 7.000000000000000000 ) ) ;
#25449 = CARTESIAN_POINT ( 'NONE',  ( 12.41725554300025713, 20.45587985069801107, -19.50104749346444422 ) ) ;
#25450 = ORIENTED_EDGE ( 'NONE', *, *, #12294, .F. ) ;
#25451 = CARTESIAN_POINT ( 'NONE',  ( 30.99684195017841404, -17.08716579088729759, -11.06784137463484008 ) ) ;
#25452 = DIRECTION ( 'NONE',  ( 1.000000000000000000, 0.000000000000000000, 0.000000000000000000 ) ) ;
#25453 = ORIENTED_EDGE ( 'NONE', *, *, #26135, .F. ) ;
#25455 = CARTESIAN_POINT ( 'NONE',  ( 8.188662802687307618, 9.932154366953152902, 7.455539900862802050 ) ) ;
#25454 = CARTESIAN_POINT ( 'NONE',  ( -14.79267235827050619, 26.23776883278636518, -9.685074664482419493 ) ) ;
#25456 = CARTESIAN_POINT ( 'NONE',  ( -15.57329205153430429, -25.98394400221819467, -9.671856144017159096 ) ) ;
#25457 = EDGE_CURVE ( 'NONE', #24423, #7663, #36856, .T. ) ;
#25458 = CARTESIAN_POINT ( 'NONE',  ( -12.68475447279705648, 27.14725768220950286, 10.50000000000000000 ) ) ;
#25459 = CIRCLE ( 'NONE', #6667, 0.5000000000000004441 ) ;
#25460 = ORIENTED_EDGE ( 'NONE', *, *, #10388, .T. ) ;
#25461 = CARTESIAN_POINT ( 'NONE',  ( -18.15436357158603897, -9.522238560471439683, -30.00000000000001421 ) ) ;
#25462 = CARTESIAN_POINT ( 'NONE',  ( -10.56852682390984199, -20.57919107763412114, -20.61136777398266062 ) ) ;
#25463 = CARTESIAN_POINT ( 'NONE',  ( 7.468455364333221880, 29.89744377950669474, 11.00000000000000000 ) ) ;
#25464 = CARTESIAN_POINT ( 'NONE',  ( 12.66487866387964978, 16.11973886863585648, -30.00000000000000711 ) ) ;
#25465 = ORIENTED_EDGE ( 'NONE', *, *, #34498, .F. ) ;
#25466 = CARTESIAN_POINT ( 'NONE',  ( 19.82221245355347605, 5.923645454667767041, -27.10773064487408845 ) ) ;
#25467 = CARTESIAN_POINT ( 'NONE',  ( 11.69134295108989186, 15.74999999999995204, 7.000000000000000000 ) ) ;
#25468 = AXIS2_PLACEMENT_3D ( 'NONE', #38631, #1871, #20948 ) ;
#25469 = CARTESIAN_POINT ( 'NONE',  ( -2.518583951651248931, 7.712953814960721743, 7.499999999999997335 ) ) ;
#25470 = DIRECTION ( 'NONE',  ( 1.000000000000000000, 0.000000000000000000, 0.000000000000000000 ) ) ;
#25471 = VERTEX_POINT ( 'NONE', #15405 ) ;
#25472 = CARTESIAN_POINT ( 'NONE',  ( -20.71452086892951172, 0.5024582651441130698, -27.42597503545741944 ) ) ;
#25473 = CARTESIAN_POINT ( 'NONE',  ( 29.10019562751751820, -0.1449826646537783481, -11.57629332465059235 ) ) ;
#25474 = AXIS2_PLACEMENT_3D ( 'NONE', #25823, #28472, #6530 ) ;
#25475 = CARTESIAN_POINT ( 'NONE',  ( 26.84751477640508810, -17.98144108585584178, 20.25080042701592120 ) ) ;
#25476 = ORIENTED_EDGE ( 'NONE', *, *, #31611, .F. ) ;
#25477 = CARTESIAN_POINT ( 'NONE',  ( -17.81784622497958281, -13.85677843414106292, -30.00000000000001421 ) ) ;
#25478 = DIRECTION ( 'NONE',  ( 0.000000000000000000, 0.000000000000000000, 1.000000000000000000 ) ) ;
#25479 = ORIENTED_EDGE ( 'NONE', *, *, #31240, .T. ) ;
#25480 = CYLINDRICAL_SURFACE ( 'NONE', #31393, 1.000000000000000888 ) ;
#25481 = EDGE_CURVE ( 'NONE', #25659, #36019, #3214, .T. ) ;
#25482 = CIRCLE ( 'NONE', #17078, 1.000000000000000000 ) ;
#25483 = DIRECTION ( 'NONE',  ( 0.000000000000000000, 0.000000000000000000, 1.000000000000000000 ) ) ;
#25484 = CARTESIAN_POINT ( 'NONE',  ( 28.92287456541829371, 1.976372635698110614, -4.999999999999999112 ) ) ;
#25485 = CARTESIAN_POINT ( 'NONE',  ( 6.045822647813611006, 36.95161842508870365, -7.135958126947899771 ) ) ;
#25486 = CARTESIAN_POINT ( 'NONE',  ( 3.295881626406585774, 9.398963235502479918, 7.000000000000000000 ) ) ;
#25487 = ORIENTED_EDGE ( 'NONE', *, *, #27020, .F. ) ;
#25488 = CARTESIAN_POINT ( 'NONE',  ( -6.713764256189716839, 35.89999254728751055, 10.49999999999999822 ) ) ;
#25489 = AXIS2_PLACEMENT_3D ( 'NONE', #18777, #31167, #291 ) ;
#25490 = LINE ( 'NONE', #24905, #11021 ) ;
#25491 = CARTESIAN_POINT ( 'NONE',  ( 30.14285136919114549, -23.17491017602459280, -5.860341728232943304 ) ) ;
#25492 = CARTESIAN_POINT ( 'NONE',  ( -7.824485034907247893, 10.87986945260456473, 7.500000000000000888 ) ) ;
#25493 = CARTESIAN_POINT ( 'NONE',  ( -3.587667106213709101, 35.31811204475769728, 12.00000000000000000 ) ) ;
#25494 =( LENGTH_UNIT ( ) NAMED_UNIT ( * ) SI_UNIT ( .MILLI., .METRE. ) );
#25495 = CARTESIAN_POINT ( 'NONE',  ( 14.90518469689150827, 26.75391244360456966, -8.740800605981732474 ) ) ;
#25496 = CARTESIAN_POINT ( 'NONE',  ( 5.068835528549737290, 13.82204480395803081, 10.49999999999999822 ) ) ;
#25497 = ORIENTED_EDGE ( 'NONE', *, *, #31412, .T. ) ;
#25498 = AXIS2_PLACEMENT_3D ( 'NONE', #37785, #28244, #12605 ) ;
#25500 = DIRECTION ( 'NONE',  ( 0.000000000000000000, 0.000000000000000000, 1.000000000000000000 ) ) ;
#25499 = CARTESIAN_POINT ( 'NONE',  ( -15.89936984974615619, 18.38899797113655055, -15.74513658678639061 ) ) ;
#25501 = CARTESIAN_POINT ( 'NONE',  ( 13.14565515434632026, 15.48770272715369956, 10.82238861112334938 ) ) ;
#25502 = CARTESIAN_POINT ( 'NONE',  ( 15.45091137245021429, -26.73300375246232008, -5.474195469181999840 ) ) ;
#25503 = DIRECTION ( 'NONE',  ( -0.000000000000000000, -0.000000000000000000, -1.000000000000000000 ) ) ;
#25504 = CARTESIAN_POINT ( 'NONE',  ( 15.29638078504309817, 26.50914737159216372, -7.357895937986722146 ) ) ;
#25505 = EDGE_LOOP ( 'NONE', ( #13594, #15396, #29791, #39472 ) ) ;
#25506 = CARTESIAN_POINT ( 'NONE',  ( 13.48417877264113685, 22.82990984439727811, -15.44940169434631727 ) ) ;
#25507 = ORIENTED_EDGE ( 'NONE', *, *, #5023, .T. ) ;
#25508 = CARTESIAN_POINT ( 'NONE',  ( 14.38243823352023476, 26.25560849141422182, 10.49999999999999822 ) ) ;
#25509 = CARTESIAN_POINT ( 'NONE',  ( -15.37403055690315590, -26.58998761537970168, -6.888177748688296020 ) ) ;
#25510 = ADVANCED_FACE ( 'NONE', ( #3406 ), #18658, .T. ) ;
#25511 = CIRCLE ( 'NONE', #14505, 1.000000000000000000 ) ;
#25512 = CARTESIAN_POINT ( 'NONE',  ( -24.59814121633841566, -28.40949844211078812, 12.73282698324864626 ) ) ;
#25513 = CARTESIAN_POINT ( 'NONE',  ( -25.72242270509724449, -17.76379069224040563, -14.74151087500952073 ) ) ;
#25514 = CARTESIAN_POINT ( 'NONE',  ( -3.881175749157317334, -22.08623497455011631, -19.01312672737709519 ) ) ;
#25515 = CARTESIAN_POINT ( 'NONE',  ( 15.58265619670584989, 25.25374846204108081, -7.834539407195180161 ) ) ;
#25517 = EDGE_CURVE ( 'NONE', #25273, #34673, #40182, .T. ) ;
#25516 = EDGE_LOOP ( 'NONE', ( #32875, #2871, #22581, #13989 ) ) ;
#25518 = CARTESIAN_POINT ( 'NONE',  ( 22.26700180465959633, 9.975047470158974861, -10.37867134500859301 ) ) ;
#25519 = CARTESIAN_POINT ( 'NONE',  ( 18.68939205906152523, 29.94303747981216901, 11.00000000000000000 ) ) ;
#25520 = CARTESIAN_POINT ( 'NONE',  ( -4.960307196185540057, 37.22510528292767873, 16.87380292611441845 ) ) ;
#25521 = VERTEX_POINT ( 'NONE', #33712 ) ;
#25522 = CARTESIAN_POINT ( 'NONE',  ( -33.65402088194174723, -4.443209378264873166, -7.242161384985005945 ) ) ;
#25523 = AXIS2_PLACEMENT_3D ( 'NONE', #4626, #17027, #10932 ) ;
#25524 = EDGE_CURVE ( 'NONE', #2211, #12521, #39981, .T. ) ;
#25525 = CARTESIAN_POINT ( 'NONE',  ( -17.58821720676843370, 10.15456193889213665, 19.66345542862528362 ) ) ;
#25526 = ORIENTED_EDGE ( 'NONE', *, *, #19039, .F. ) ;
#25527 = CARTESIAN_POINT ( 'NONE',  ( -19.48557158514998022, -11.24999999999982414, 3.000000000000000000 ) ) ;
#25528 = AXIS2_PLACEMENT_3D ( 'NONE', #1618, #38383, #7706 ) ;
#25529 = CARTESIAN_POINT ( 'NONE',  ( 12.80736835487433289, 15.68301270189216545, 7.000000000000000000 ) ) ;
#25530 = CARTESIAN_POINT ( 'NONE',  ( 30.43074936207083780, -13.30772945900434756, -12.90888064005893909 ) ) ;
#25531 = CARTESIAN_POINT ( 'NONE',  ( 34.04990527597812644, -21.89993885138089524, 12.14047268033092308 ) ) ;
#25532 = TOROIDAL_SURFACE ( 'NONE', #8023, 1.000000000000000000, 0.5000000000000000000 ) ;
#25533 = ORIENTED_EDGE ( 'NONE', *, *, #35457, .T. ) ;
#25534 = ORIENTED_EDGE ( 'NONE', *, *, #3954, .T. ) ;
#25535 = DIRECTION ( 'NONE',  ( -0.8090169943749426773, 0.5877852522924797984, 0.000000000000000000 ) ) ;
#25536 = CARTESIAN_POINT ( 'NONE',  ( -15.41813410374787807, 26.77565562682181266, -5.000000000000003553 ) ) ;
#25537 = EDGE_CURVE ( 'NONE', #9089, #17047, #22576, .T. ) ;
#25538 = EDGE_CURVE ( 'NONE', #32074, #9588, #29752, .T. ) ;
#25539 = DIRECTION ( 'NONE',  ( 1.000000000000000000, 0.000000000000000000, 0.000000000000000000 ) ) ;
#25540 = ORIENTED_EDGE ( 'NONE', *, *, #22527, .F. ) ;
#25541 = CIRCLE ( 'NONE', #7354, 15.00000000000000000 ) ;
#25542 = CARTESIAN_POINT ( 'NONE',  ( -0.4275284198932905455, 22.02762823501048217, -24.21675859296236055 ) ) ;
#25543 = CARTESIAN_POINT ( 'NONE',  ( -14.01196168477328641, 27.85442546840040734, 7.455539900862793168 ) ) ;
#25544 = DIRECTION ( 'NONE',  ( -0.6459741880212603871, -0.2876062384759424106, -0.7071067811865422437 ) ) ;
#25545 = CARTESIAN_POINT ( 'NONE',  ( 22.48079666807004529, 18.61591633964211212, 11.00000000000000178 ) ) ;
#25546 = CARTESIAN_POINT ( 'NONE',  ( -11.03641663870442713, 15.85735326529964873, 13.00000000000000178 ) ) ;
#25547 = CARTESIAN_POINT ( 'NONE',  ( -9.363324537585850038, 32.27640801132209702, 9.500000000000000000 ) ) ;
#25548 = COLOUR_RGB ( '', 0.31764706, 0.68627451, 0.89019608) ;
#25549 = CARTESIAN_POINT ( 'NONE',  ( 13.91852109418007544, 29.04111810746936229, -8.650529261331366015 ) ) ;
#25550 = DIRECTION ( 'NONE',  ( -0.9135454576426051965, -0.4067366430757904938, 0.000000000000000000 ) ) ;
#25551 = ORIENTED_EDGE ( 'NONE', *, *, #37830, .F. ) ;
#25553 = FACE_OUTER_BOUND ( 'NONE', #29470, .T. ) ;
#25552 = CARTESIAN_POINT ( 'NONE',  ( -19.72315440816933219, 10.70534603068222168, -18.01648663879400303 ) ) ;
#25554 = DIRECTION ( 'NONE',  ( 1.000000000000000000, 0.000000000000000000, 0.000000000000000000 ) ) ;
#25555 = CARTESIAN_POINT ( 'NONE',  ( 10.35225884972404664, -19.11980502629199208, -23.83773470646794479 ) ) ;
#25556 = CARTESIAN_POINT ( 'NONE',  ( 15.02655339034802395, -26.00115400090650652, -9.236043780760597954 ) ) ;
#25557 = CARTESIAN_POINT ( 'NONE',  ( -9.331903152615899089, 11.35703883385581037, 7.500000000000000888 ) ) ;
#25558 = CARTESIAN_POINT ( 'NONE',  ( 11.43104729973414102, 18.48323776028994203, -23.84550412495152116 ) ) ;
#25559 = CARTESIAN_POINT ( 'NONE',  ( -35.36940577612494963, -20.42053594592268695, -14.51648065752878480 ) ) ;
#25560 = CARTESIAN_POINT ( 'NONE',  ( 9.393455880287467252, 11.27231877233265323, 10.49999999999999822 ) ) ;
#25561 = EDGE_CURVE ( 'NONE', #26852, #5502, #4434, .T. ) ;
#25562 = CIRCLE ( 'NONE', #38534, 1.000000000000000888 ) ;
#25563 = CARTESIAN_POINT ( 'NONE',  ( -22.71156489100481934, -22.69643118484121658, -13.00228647887131750 ) ) ;
#25564 = CARTESIAN_POINT ( 'NONE',  ( 6.205112128679617811, -24.95655587313122581, -7.408272597870006138 ) ) ;
#25565 = CARTESIAN_POINT ( 'NONE',  ( 13.04743348150465643, 21.46120596883949005, -17.45731936358998126 ) ) ;
#25566 = EDGE_CURVE ( 'NONE', #10996, #32239, #21945, .T. ) ;
#25567 = CARTESIAN_POINT ( 'NONE',  ( 31.72993655656084755, -21.47020083663496237, -5.857146272187097047 ) ) ;
#25568 = CARTESIAN_POINT ( 'NONE',  ( 14.00731263743715793, 27.57698287931455994, 10.82238861112332629 ) ) ;
#25569 = DIRECTION ( 'NONE',  ( -0.2079116908177516265, 0.9781476007338072431, 0.000000000000000000 ) ) ;
#25570 = ORIENTED_EDGE ( 'NONE', *, *, #32615, .F. ) ;
#25571 = CARTESIAN_POINT ( 'NONE',  ( -7.859885379884856249, 33.27431112823943948, -11.13818915821171274 ) ) ;
#25572 = VECTOR ( 'NONE', #36010, 1000.000000000000000 ) ;
#25573 = FACE_OUTER_BOUND ( 'NONE', #6090, .T. ) ;
#25574 = ORIENTED_EDGE ( 'NONE', *, *, #20432, .F. ) ;
#25575 = CARTESIAN_POINT ( 'NONE',  ( 20.61132694413180388, 0.8343915772789830543, -28.07671223784028314 ) ) ;
#25576 = DIRECTION ( 'NONE',  ( 0.000000000000000000, 0.000000000000000000, 1.000000000000000000 ) ) ;
#25577 = LINE ( 'NONE', #31481, #30360 ) ;
#25578 = ORIENTED_EDGE ( 'NONE', *, *, #38231, .T. ) ;
#25579 = CARTESIAN_POINT ( 'NONE',  ( -29.71183529215159780, 0.1435226407617324063, -9.711128893466487000 ) ) ;
#25580 = CARTESIAN_POINT ( 'NONE',  ( -3.835137251120299684, 29.44922644035488446, 6.000000000000000000 ) ) ;
#25581 = ORIENTED_EDGE ( 'NONE', *, *, #39973, .F. ) ;
#25582 = CARTESIAN_POINT ( 'NONE',  ( 35.10761102947512313, -8.438163957854742492, -6.314036995521373541 ) ) ;
#25583 = AXIS2_PLACEMENT_3D ( 'NONE', #10177, #22552, #3873 ) ;
#25584 = ORIENTED_EDGE ( 'NONE', *, *, #38037, .F. ) ;
#25585 = APPLICATION_PROTOCOL_DEFINITION ( 'draft international standard', 'automotive_design', 1998, #26987 ) ;
#25586 = CARTESIAN_POINT ( 'NONE',  ( -7.591957726968742826, 38.93640765974102180, 11.55979286843917464 ) ) ;
#25587 = CARTESIAN_POINT ( 'NONE',  ( 8.118377661053324701, 10.47536095541698486, 7.000000000000000000 ) ) ;
#25588 = CARTESIAN_POINT ( 'NONE',  ( -8.238488885696254371, 24.65111619403957022, 9.000000000000001776 ) ) ;
#25589 = CARTESIAN_POINT ( 'NONE',  ( 7.884092257452433472, 32.87438847863636937, 18.87996532025784902 ) ) ;
#25590 = AXIS2_PLACEMENT_3D ( 'NONE', #18123, #30309, #18715 ) ;
#25591 = DIRECTION ( 'NONE',  ( -1.000000000000000000, 0.000000000000000000, 0.000000000000000000 ) ) ;
#25592 = ORIENTED_EDGE ( 'NONE', *, *, #7273, .T. ) ;
#25593 = DIRECTION ( 'NONE',  ( 1.000000000000000000, 0.000000000000000000, 0.000000000000000000 ) ) ;
#25594 = CARTESIAN_POINT ( 'NONE',  ( 4.987357081044728524, 19.92651000211460044, -30.00000000000000000 ) ) ;
#25595 = DIRECTION ( 'NONE',  ( -0.000000000000000000, -0.000000000000000000, -1.000000000000000000 ) ) ;
#25596 = EDGE_CURVE ( 'NONE', #6257, #12049, #12158, .T. ) ;
#25597 = DIRECTION ( 'NONE',  ( -0.000000000000000000, -0.000000000000000000, 1.000000000000000000 ) ) ;
#25598 = CARTESIAN_POINT ( 'NONE',  ( 17.47098692575351819, 19.68410474348366179, -8.844102737791779134 ) ) ;
#25599 = CARTESIAN_POINT ( 'NONE',  ( 9.086865688058274770, 35.45071178617213548, -6.734195449777575782 ) ) ;
#25600 = VERTEX_POINT ( 'NONE', #9111 ) ;
#25601 = CARTESIAN_POINT ( 'NONE',  ( 11.71983824754993542, -20.36894919573499863, -20.47130099390510338 ) ) ;
#25602 = PLANE ( 'NONE',  #6782 ) ;
#25603 = CARTESIAN_POINT ( 'NONE',  ( -4.348113209407908464, 9.835177808069893501, 13.00000000000000178 ) ) ;
#25604 = CIRCLE ( 'NONE', #4210, 18.00000000000000355 ) ;
#25605 = ORIENTED_EDGE ( 'NONE', *, *, #22281, .T. ) ;
#25606 = CARTESIAN_POINT ( 'NONE',  ( -11.12856712346650312, 17.61049140408264080, -26.83074947876917449 ) ) ;
#25607 = CARTESIAN_POINT ( 'NONE',  ( -35.45119270310583914, -5.541672998605994493, 15.13084544680260457 ) ) ;
#25608 = CARTESIAN_POINT ( 'NONE',  ( 9.271440805881887570, -18.28379014461920349, -29.35293047210549489 ) ) ;
#25609 = DIRECTION ( 'NONE',  ( -0.000000000000000000, -0.000000000000000000, -1.000000000000000000 ) ) ;
#25610 = ORIENTED_EDGE ( 'NONE', *, *, #26514, .T. ) ;
#25611 = ORIENTED_EDGE ( 'NONE', *, *, #38079, .F. ) ;
#25612 = CARTESIAN_POINT ( 'NONE',  ( -13.62515121305021637, 29.87907916796226360, -8.173113224430574419 ) ) ;
#25613 = VECTOR ( 'NONE', #2981, 1000.000000000000000 ) ;
#25614 = DIRECTION ( 'NONE',  ( 0.000000000000000000, 0.000000000000000000, -1.000000000000000000 ) ) ;
#25615 = FACE_BOUND ( 'NONE', #11659, .T. ) ;
#25616 = VECTOR ( 'NONE', #2771, 1000.000000000000000 ) ;
#25617 = CARTESIAN_POINT ( 'NONE',  ( -19.91373213366430761, -4.906168661338282888, -29.25106315047995054 ) ) ;
#25618 = FACE_OUTER_BOUND ( 'NONE', #15326, .T. ) ;
#25619 = VERTEX_POINT ( 'NONE', #31245 ) ;
#25620 = CARTESIAN_POINT ( 'NONE',  ( 22.19098149685552102, 0.7861450883651701638, -22.74982018612348966 ) ) ;
#25621 = CARTESIAN_POINT ( 'NONE',  ( -8.137585970691988635, 29.15429895402941085, 10.00000000000000000 ) ) ;
#25622 = DIRECTION ( 'NONE',  ( 0.000000000000000000, 0.000000000000000000, 1.000000000000000000 ) ) ;
#25623 = ADVANCED_FACE ( 'NONE', ( #24742 ), #34096, .F. ) ;
#25624 = ORIENTED_EDGE ( 'NONE', *, *, #19067, .T. ) ;
#25625 = CARTESIAN_POINT ( 'NONE',  ( -23.94331431717321834, 0.4798011554587169325, -19.49553339312929268 ) ) ;
#25626 = CARTESIAN_POINT ( 'NONE',  ( 2.211395437248501850, 12.61633075744433796, 12.00000000000000000 ) ) ;
#25627 = ORIENTED_EDGE ( 'NONE', *, *, #34721, .F. ) ;
#25628 = CARTESIAN_POINT ( 'NONE',  ( 20.72609593855841581, -1.618474817249470954, -27.28862543018874121 ) ) ;
#25629 = CARTESIAN_POINT ( 'NONE',  ( 20.37075632078805398, -2.330628970618247919, -29.99999999999998224 ) ) ;
#25630 = CARTESIAN_POINT ( 'NONE',  ( 30.90861030616521177, -0.03770625498525858460, 16.30093088680191116 ) ) ;
#25631 = ORIENTED_EDGE ( 'NONE', *, *, #12633, .T. ) ;
#25632 = CARTESIAN_POINT ( 'NONE',  ( 3.652674690108948852, 39.05729514278202430, 15.13084544680221732 ) ) ;
#25633 = CARTESIAN_POINT ( 'NONE',  ( -6.404490139165758045, 34.42612703509939820, 10.50000000000000000 ) ) ;
#25634 = AXIS2_PLACEMENT_3D ( 'NONE', #1856, #14234, #39016 ) ;
#25635 = CARTESIAN_POINT ( 'NONE',  ( -5.067517038533118523, 26.80213145839204358, 20.94377226548377990 ) ) ;
#25636 = PLANE ( 'NONE',  #6426 ) ;
#25637 = EDGE_CURVE ( 'NONE', #19392, #35589, #2501, .T. ) ;
#25638 = DIRECTION ( 'NONE',  ( 0.000000000000000000, 0.000000000000000000, -1.000000000000000000 ) ) ;
#25639 = AXIS2_PLACEMENT_3D ( 'NONE', #27122, #11089, #8635 ) ;
#25640 = CIRCLE ( 'NONE', #21760, 0.5000000000000004441 ) ;
#25641 = CIRCLE ( 'NONE', #20483, 1.000000000000000000 ) ;
#25642 = FACE_BOUND ( 'NONE', #33434, .T. ) ;
#25643 = ADVANCED_FACE ( 'NONE', ( #31050 ), #33902, .T. ) ;
#25644 = CARTESIAN_POINT ( 'NONE',  ( 15.47112132963536446, 15.31948306976098628, 19.27171037444173507 ) ) ;
#25645 = CARTESIAN_POINT ( 'NONE',  ( -23.10177455024117776, 8.837490529234450776, -9.870891380885264965 ) ) ;
#25646 = ADVANCED_FACE ( 'NONE', ( #27991 ), #28439, .T. ) ;
#25647 = CARTESIAN_POINT ( 'NONE',  ( 13.26265854479622419, -15.63203989815269779, -29.99999999999999289 ) ) ;
#25648 = EDGE_CURVE ( 'NONE', #8022, #14474, #9514, .T. ) ;
#25649 = CARTESIAN_POINT ( 'NONE',  ( -4.780767545418437514, 35.69637305007227468, 10.50000000000000000 ) ) ;
#25650 = CARTESIAN_POINT ( 'NONE',  ( 13.67698555827839968, 23.60253768574900946, -14.45466942440959635 ) ) ;
#25651 = EDGE_LOOP ( 'NONE', ( #29187, #29394 ) ) ;
#25652 = CARTESIAN_POINT ( 'NONE',  ( -14.83746131866766405, 24.15353679605524562, -11.62345532500183864 ) ) ;
#25653 = CARTESIAN_POINT ( 'NONE',  ( -17.42101839920251649, -19.25229542401853067, 20.69868183039781329 ) ) ;
#25654 = DIRECTION ( 'NONE',  ( 0.000000000000000000, 0.000000000000000000, 1.000000000000000000 ) ) ;
#25655 = CARTESIAN_POINT ( 'NONE',  ( 12.96000418219073858, 21.60184555869381384, -17.44299700738821812 ) ) ;
#25656 = ORIENTED_EDGE ( 'NONE', *, *, #33226, .F. ) ;
#25657 = CARTESIAN_POINT ( 'NONE',  ( 32.54628837895766935, -17.94405776258001239, -8.843653535525763942 ) ) ;
#25658 = DIRECTION ( 'NONE',  ( -0.3090169943749573878, -0.9510565162951503115, 0.000000000000000000 ) ) ;
#25659 = VERTEX_POINT ( 'NONE', #165 ) ;
#25661 = CARTESIAN_POINT ( 'NONE',  ( -14.91650131011210156, 21.43496667674312306, 10.76099332938164288 ) ) ;
#25660 = CARTESIAN_POINT ( 'NONE',  ( -11.06077501432392651, 18.23000144808903755, -24.98034412766138956 ) ) ;
#25662 = CARTESIAN_POINT ( 'NONE',  ( -12.84304827169525964, -22.01029806000802935, -17.37299228019244879 ) ) ;
#25663 = DIRECTION ( 'NONE',  ( 1.000000000000000000, 0.000000000000000000, 0.000000000000000000 ) ) ;
#25664 = ORIENTED_EDGE ( 'NONE', *, *, #20964, .F. ) ;
#25665 = CARTESIAN_POINT ( 'NONE',  ( -30.61059542336693085, -12.61261197708686588, -12.91721441924257974 ) ) ;
#25666 = CARTESIAN_POINT ( 'NONE',  ( -13.49856781751322110, -24.92574764376128371, -11.62344980891660740 ) ) ;
#25667 = CYLINDRICAL_SURFACE ( 'NONE', #23549, 1.000000000000000000 ) ;
#25668 = CARTESIAN_POINT ( 'NONE',  ( 14.84856562538137403, 21.17331135784270657, -14.60805661069002781 ) ) ;
#25669 = ORIENTED_EDGE ( 'NONE', *, *, #11064, .F. ) ;
#25670 = CARTESIAN_POINT ( 'NONE',  ( 27.04882373375960825, 3.777209956746526043, -8.341230441078749891 ) ) ;
#25671 = DIRECTION ( 'NONE',  ( 1.000000000000000000, 0.000000000000000000, 0.000000000000000000 ) ) ;
#25672 = ADVANCED_FACE ( 'NONE', ( #12554 ), #8915, .T. ) ;
#25673 = LINE ( 'NONE', #34825, #38764 ) ;
#25674 = EDGE_CURVE ( 'NONE', #17668, #33348, #37527, .T. ) ;
#25675 = AXIS2_PLACEMENT_3D ( 'NONE', #7166, #1087, #28909 ) ;
#25676 = ORIENTED_EDGE ( 'NONE', *, *, #39560, .T. ) ;
#25677 = CARTESIAN_POINT ( 'NONE',  ( -21.00158985414197588, 0.4703539060713058384, -26.19501892574664481 ) ) ;
#25678 = CARTESIAN_POINT ( 'NONE',  ( 26.15888819988984437, -0.1763494521739284449, -16.38123973257840760 ) ) ;
#25679 = VECTOR ( 'NONE', #22498, 1000.000000000000000 ) ;
#25680 = CIRCLE ( 'NONE', #28932, 16.00000000000000000 ) ;
#25681 = CARTESIAN_POINT ( 'NONE',  ( 26.17288861939790579, -20.72787579792467838, 19.66345542862498519 ) ) ;
#25682 = AXIS2_PLACEMENT_3D ( 'NONE', #33918, #18279, #30672 ) ;
#25683 = ORIENTED_EDGE ( 'NONE', *, *, #12296, .F. ) ;
#25684 = CARTESIAN_POINT ( 'NONE',  ( 16.77267017469755217, -29.13948811618736912, -5.000000000000000888 ) ) ;
#25685 = CYLINDRICAL_SURFACE ( 'NONE', #31632, 0.5000000000000004441 ) ;
#25686 = VERTEX_POINT ( 'NONE', #35651 ) ;
#25687 = DIRECTION ( 'NONE',  ( 0.9135454576426004225, -0.4067366430758009854, 0.000000000000000000 ) ) ;
#25688 = B_SPLINE_CURVE_WITH_KNOTS ( 'NONE', 3,
 ( #9947, #16444, #10550, #19284, #32080, #13182, #31679, #29236, #1007, #16652, #4452, #28631, #29034, #26183, #1210, #1408, #19483, #3847 ),
 .UNSPECIFIED., .F., .F.,
 ( 4, 2, 2, 2, 2, 2, 2, 2, 4 ),
 ( 0.000000000000000000, 0.1250000000000000555, 0.2500000000000001110, 0.3750000000000001665, 0.5000000000000002220, 0.6250000000000002220, 0.7500000000000003331, 0.8750000000000001110, 1.000000000000000000 ),
 .UNSPECIFIED. ) ;
#25689 = EDGE_CURVE ( 'NONE', #3455, #13041, #34495, .T. ) ;
#25690 = DIRECTION ( 'NONE',  ( 1.000000000000000000, 0.000000000000000000, 0.000000000000000000 ) ) ;
#25691 = CYLINDRICAL_SURFACE ( 'NONE', #9321, 1.000000000000000000 ) ;
#25692 = DIRECTION ( 'NONE',  ( 1.000000000000000000, 0.000000000000000000, 0.000000000000000000 ) ) ;
#25693 = ORIENTED_EDGE ( 'NONE', *, *, #7911, .T. ) ;
#25694 = DIRECTION ( 'NONE',  ( 0.000000000000000000, 0.000000000000000000, 1.000000000000000000 ) ) ;
#25695 = DIRECTION ( 'NONE',  ( 0.000000000000000000, 0.000000000000000000, 1.000000000000000000 ) ) ;
#25696 = CARTESIAN_POINT ( 'NONE',  ( 25.94815390757270634, -24.00269173140258872, -9.783439592027228571 ) ) ;
#25697 = AXIS2_PLACEMENT_3D ( 'NONE', #7928, #4488, #29067 ) ;
#25698 = DIRECTION ( 'NONE',  ( 1.000000000000000000, 0.000000000000000000, 0.000000000000000000 ) ) ;
#25699 = CARTESIAN_POINT ( 'NONE',  ( 11.87435565298210882, 15.06698729810772619, 9.500000000000000000 ) ) ;
#25700 = CARTESIAN_POINT ( 'NONE',  ( 14.53483714358199919, 25.97957738232134872, -10.61578658074032333 ) ) ;
#25701 = LINE ( 'NONE', #12520, #16553 ) ;
#25702 = ORIENTED_EDGE ( 'NONE', *, *, #15480, .T. ) ;
#25705 = LINE ( 'NONE', #13309, #14223 ) ;
#25704 = VECTOR ( 'NONE', #14131, 1000.000000000000000 ) ;
#25703 = CARTESIAN_POINT ( 'NONE',  ( -15.23813856142597167, 17.31405161251928249, -18.82644271334805453 ) ) ;
#25706 = DIRECTION ( 'NONE',  ( 1.000000000000000000, 0.000000000000000000, 0.000000000000000000 ) ) ;
#25707 = CIRCLE ( 'NONE', #433, 1.000000000000000888 ) ;
#25708 = CARTESIAN_POINT ( 'NONE',  ( 15.25374212246388694, -26.48790319330748133, -7.358088638680141180 ) ) ;
#25709 = DIRECTION ( 'NONE',  ( 0.6847716512521591081, 0.4446959099295441087, 0.5773502691896197359 ) ) ;
#25710 = CARTESIAN_POINT ( 'NONE',  ( 13.76937081925355955, 23.39622061500657324, -14.47626747317092466 ) ) ;
#25711 = ORIENTED_EDGE ( 'NONE', *, *, #17836, .F. ) ;
#25712 = CARTESIAN_POINT ( 'NONE',  ( 11.17466575968340692, 17.76334817009650635, -26.22383286113582201 ) ) ;
#25713 = ORIENTED_EDGE ( 'NONE', *, *, #2542, .T. ) ;
#25715 = CARTESIAN_POINT ( 'NONE',  ( 14.45052027064708255, 26.47704597190804066, 10.49999999999999822 ) ) ;
#25714 = CARTESIAN_POINT ( 'NONE',  ( -15.34454670589055603, 26.76954483690364839, -6.415642936482374381 ) ) ;
#25716 = CARTESIAN_POINT ( 'NONE',  ( -9.469408548107701051, -18.18187935292228019, -29.34893421946817682 ) ) ;
#25717 = CARTESIAN_POINT ( 'NONE',  ( -24.49773858737561838, -28.07267629079790439, 13.92931973827830383 ) ) ;
#25718 = CARTESIAN_POINT ( 'NONE',  ( -26.62430720910999682, -18.39156676930381451, -13.81496718408933333 ) ) ;
#25719 = CARTESIAN_POINT ( 'NONE',  ( -4.703611708043858641, -24.60377627214949925, -8.882725814672168596 ) ) ;
#25720 = CARTESIAN_POINT ( 'NONE',  ( 11.42783708703505852, 17.06964071376472702, -28.72407638117795514 ) ) ;
#25721 = ORIENTED_EDGE ( 'NONE', *, *, #2844, .T. ) ;
#25722 = CARTESIAN_POINT ( 'NONE',  ( 22.52668103003253464, 8.989979787406557676, -11.86183922785617462 ) ) ;
#25723 = CARTESIAN_POINT ( 'NONE',  ( 10.37659643210531257, 39.73422260934388106, 11.00000000000000000 ) ) ;
#25724 = ADVANCED_FACE ( 'NONE', ( #31987 ), #13907, .T. ) ;
#25725 = CARTESIAN_POINT ( 'NONE',  ( 6.320269494896071372, 36.18253918181417816, 17.42190598798391221 ) ) ;
#25726 = ORIENTED_EDGE ( 'NONE', *, *, #30406, .T. ) ;
#25727 = CARTESIAN_POINT ( 'NONE',  ( -28.14360955461928171, -2.773391863289171866, -15.14227585713986812 ) ) ;
#25728 = EDGE_CURVE ( 'NONE', #14129, #24820, #16558, .T. ) ;
#25729 = CARTESIAN_POINT ( 'NONE',  ( -22.71318823113784546, 6.927825590549916868, 17.92354375535276390 ) ) ;
#25730 = ORIENTED_EDGE ( 'NONE', *, *, #5546, .T. ) ;
#25731 = CARTESIAN_POINT ( 'NONE',  ( 22.79104142221947171, -15.00151558123164008, 20.99999999999999645 ) ) ;
#25732 = CARTESIAN_POINT ( 'NONE',  ( -0.3582326297815359162, 33.31072022568110924, 6.000000000000000000 ) ) ;
#25733 = CARTESIAN_POINT ( 'NONE',  ( 19.13306659232624085, -8.411872202393357867, -26.98792224631750258 ) ) ;
#25734 = CARTESIAN_POINT ( 'NONE',  ( 37.28086807198950225, -8.991428209509072289, 12.14047268033097815 ) ) ;
#25735 = AXIS2_PLACEMENT_3D ( 'NONE', #2503, #31273, #15082 ) ;
#25736 = VERTEX_POINT ( 'NONE', #11071 ) ;
#25737 = ORIENTED_EDGE ( 'NONE', *, *, #9833, .F. ) ;
#25738 = CARTESIAN_POINT ( 'NONE',  ( -12.05736835487443237, 14.38397459621567442, 7.499999999999993783 ) ) ;
#25739 = CARTESIAN_POINT ( 'NONE',  ( -27.20167217120908632, 3.999461679458497620, -5.000000000000001776 ) ) ;
#25740 = EDGE_CURVE ( 'NONE', #4731, #21130, #29106, .T. ) ;
#25741 = DIRECTION ( 'NONE',  ( 0.000000000000000000, 0.000000000000000000, -1.000000000000000000 ) ) ;
#25742 = EDGE_LOOP ( 'NONE', ( #25118, #23381, #14192, #11310 ) ) ;
#25743 = EDGE_CURVE ( 'NONE', #3918, #36944, #19594, .T. ) ;
#25744 = CARTESIAN_POINT ( 'NONE',  ( -0.7539017812582481382, 38.52547057370831141, -5.000000000000002665 ) ) ;
#25745 = FACE_OUTER_BOUND ( 'NONE', #40064, .T. ) ;
#25746 = DIRECTION ( 'NONE',  ( 0.7431448254773961315, 0.6691306063588561281, 0.000000000000000000 ) ) ;
#25747 = CARTESIAN_POINT ( 'NONE',  ( 20.57674455326933582, 23.15285302515658472, 10.99999999999999822 ) ) ;
#25748 = CARTESIAN_POINT ( 'NONE',  ( -10.16521142134453548, 24.66068167190384841, 6.000000000000000000 ) ) ;
#25749 = PLANE ( 'NONE',  #37194 ) ;
#25750 = CARTESIAN_POINT ( 'NONE',  ( 9.326849233417362939, 18.43685803866042150, -27.97763387032424731 ) ) ;
#25751 = CARTESIAN_POINT ( 'NONE',  ( 2.629601561899395534, 7.723830143584016206, 10.49999999999999822 ) ) ;
#25752 = VERTEX_POINT ( 'NONE', #1518 ) ;
#25753 = ADVANCED_FACE ( 'NONE', ( #17172 ), #12861, .T. ) ;
#25755 = CARTESIAN_POINT ( 'NONE',  ( 0.3762615568374529929, 19.56555719779890978, 6.000000000000000000 ) ) ;
#25754 = CARTESIAN_POINT ( 'NONE',  ( -19.54739990906080394, 14.10301885897343155, -11.87122386020018006 ) ) ;
#25756 = CARTESIAN_POINT ( 'NONE',  ( 4.331888854854896387, 42.14502281367649772, 22.99999999999999645 ) ) ;
#25757 = CARTESIAN_POINT ( 'NONE',  ( 15.14825655869951682, -26.16207617773802596, -8.764898773645015240 ) ) ;
#25758 = CARTESIAN_POINT ( 'NONE',  ( 10.54146960747273987, 17.40487552589537401, 6.000000000000000000 ) ) ;
#25759 = CARTESIAN_POINT ( 'NONE',  ( 15.21391305131906080, 26.46934913501528541, -7.825681926150065415 ) ) ;
#25760 = CARTESIAN_POINT ( 'NONE',  ( -37.62663912510979003, -8.659558992827880886, -14.26382729546507555 ) ) ;
#25761 = CARTESIAN_POINT ( 'NONE',  ( 2.211395437248501850, 12.61633075744433796, 6.000000000000000000 ) ) ;
#25762 = CIRCLE ( 'NONE', #8258, 18.00000000000002487 ) ;
#25763 = CARTESIAN_POINT ( 'NONE',  ( -25.31025310574754883, -25.23397962983047194, -8.474964599348188798 ) ) ;
#25764 = CARTESIAN_POINT ( 'NONE',  ( 5.866761025329905621, -24.11837628505799458, -11.82181453652845882 ) ) ;
#25765 = CARTESIAN_POINT ( 'NONE',  ( 15.37647888069712465, 26.23441537448958272, -7.358884453500203371 ) ) ;
#25766 = CARTESIAN_POINT ( 'NONE',  ( 25.27966917872702624, -18.27353908186211839, -14.74917764330799308 ) ) ;
#25767 = DIRECTION ( 'NONE',  ( 1.000000000000000000, 0.000000000000000000, 0.000000000000000000 ) ) ;
#25768 = CARTESIAN_POINT ( 'NONE',  ( -38.48801548572855324, -4.879739702264117795, 10.99999999999999822 ) ) ;
#25770 = ORIENTED_EDGE ( 'NONE', *, *, #13737, .T. ) ;
#25769 = EDGE_CURVE ( 'NONE', #15233, #12521, #21316, .T. ) ;
#25771 = CARTESIAN_POINT ( 'NONE',  ( -7.233295743329782646, 30.62580296063414309, -13.90069797551026021 ) ) ;
#25772 = AXIS2_PLACEMENT_3D ( 'NONE', #29191, #35285, #25930 ) ;
#25773 = EDGE_CURVE ( 'NONE', #33038, #22329, #35588, .T. ) ;
#25774 = ORIENTED_EDGE ( 'NONE', *, *, #13131, .T. ) ;
#25775 = EDGE_CURVE ( 'NONE', #14003, #11406, #39464, .T. ) ;
#25776 = AXIS2_PLACEMENT_3D ( 'NONE', #20475, #39351, #23911 ) ;
#25777 = DIRECTION ( 'NONE',  ( 1.000000000000000000, 0.000000000000000000, 0.000000000000000000 ) ) ;
#25778 = ORIENTED_EDGE ( 'NONE', *, *, #25415, .F. ) ;
#25779 = CARTESIAN_POINT ( 'NONE',  ( 30.01319108853827444, 0.005912998638344907354, -9.238060575309988920 ) ) ;
#25780 = LINE ( 'NONE', #10346, #29087 ) ;
#25781 = FACE_OUTER_BOUND ( 'NONE', #20309, .T. ) ;
#25782 = ORIENTED_EDGE ( 'NONE', *, *, #16084, .F. ) ;
#25783 = CARTESIAN_POINT ( 'NONE',  ( -23.28487554430953566, 0.6417891521472164351, -20.55291216075323391 ) ) ;
#25784 = DIRECTION ( 'NONE',  ( 1.000000000000000000, 0.000000000000000000, 0.000000000000000000 ) ) ;
#25785 = ORIENTED_EDGE ( 'NONE', *, *, #18014, .T. ) ;
#25786 = CARTESIAN_POINT ( 'NONE',  ( 26.20077895376393684, -6.234191634555112493, -17.82519732595303452 ) ) ;
#25787 = VERTEX_POINT ( 'NONE', #22095 ) ;
#25788 = SHAPE_DEFINITION_REPRESENTATION ( #1274, #12760 ) ;
#25789 = CARTESIAN_POINT ( 'NONE',  ( 15.98959510862154509, 30.99271259066425088, 11.55979286843923148 ) ) ;
#25790 = DIRECTION ( 'NONE',  ( 1.000000000000000000, 0.000000000000000000, 0.000000000000000000 ) ) ;
#25791 = DIRECTION ( 'NONE',  ( -0.000000000000000000, -0.000000000000000000, -1.000000000000000000 ) ) ;
#25792 = ADVANCED_FACE ( 'NONE', ( #4765 ), #32341, .T. ) ;
#25793 = CARTESIAN_POINT ( 'NONE',  ( -2.498547013092590863, 33.82729453933302466, 19.66345542862529427 ) ) ;
#25794 = AXIS2_PLACEMENT_3D ( 'NONE', #11800, #14041, #30292 ) ;
#25795 = AXIS2_PLACEMENT_3D ( 'NONE', #16999, #7840, #13938 ) ;
#25796 = DIRECTION ( 'NONE',  ( -0.000000000000000000, -0.000000000000000000, -1.000000000000000000 ) ) ;
#25797 = ORIENTED_EDGE ( 'NONE', *, *, #1972, .T. ) ;
#25798 = EDGE_CURVE ( 'NONE', #26803, #8150, #36892, .T. ) ;
#25799 = CARTESIAN_POINT ( 'NONE',  ( -9.103489325454093617, 18.41553740122394345, -29.99999999999998224 ) ) ;
#25800 = DIRECTION ( 'NONE',  ( 0.000000000000000000, 0.000000000000000000, -1.000000000000000000 ) ) ;
#25801 = AXIS2_PLACEMENT_3D ( 'NONE', #27741, #18409, #28333 ) ;
#25802 = CARTESIAN_POINT ( 'NONE',  ( -5.440836655099179353, 34.39106106163288246, 13.00000000000000178 ) ) ;
#25803 = CARTESIAN_POINT ( 'NONE',  ( 16.07357205507025100, 16.08392265437850810, -18.91655558039364848 ) ) ;
#25804 = AXIS2_PLACEMENT_3D ( 'NONE', #22223, #307, #20349 ) ;
#25805 = CARTESIAN_POINT ( 'NONE',  ( 10.90692232337486445, 34.26194292751238635, -4.999999999999999112 ) ) ;
#25806 = ORIENTED_EDGE ( 'NONE', *, *, #2053, .F. ) ;
#25807 = DIRECTION ( 'NONE',  ( -0.3090169943749573878, -0.9510565162951503115, 0.000000000000000000 ) ) ;
#25808 = DIRECTION ( 'NONE',  ( 0.4731467892558156030, -0.5254827454987647251, -0.7071067811865427988 ) ) ;
#25809 = CARTESIAN_POINT ( 'NONE',  ( 15.35372630195935706, -25.59917946473734673, -10.60842069110901598 ) ) ;
#25810 = CARTESIAN_POINT ( 'NONE',  ( 15.07283634909883752, -28.35394831540530447, 13.32518128616608699 ) ) ;
#25811 = CARTESIAN_POINT ( 'NONE',  ( -14.62786683182126168, 20.45979510329166828, 10.94611345180490503 ) ) ;
#25812 = ORIENTED_EDGE ( 'NONE', *, *, #12493, .F. ) ;
#25813 = CARTESIAN_POINT ( 'NONE',  ( -15.02832875975274973, 25.93642894353117256, -9.238718023697360948 ) ) ;
#25814 = CARTESIAN_POINT ( 'NONE',  ( -34.64549836162045438, -5.829828142712631056, 16.30093088680235880 ) ) ;
#25815 = CARTESIAN_POINT ( 'NONE',  ( 9.727620666417239548, -18.90945770702390760, -25.04146322545150483 ) ) ;
#25816 = CARTESIAN_POINT ( 'NONE',  ( -22.32447841415231338, 25.34915137120643180, 11.00000000000000000 ) ) ;
#25817 = EDGE_LOOP ( 'NONE', ( #5190, #38184, #19359, #26052, #15532, #10952 ) ) ;
#25818 = VERTEX_POINT ( 'NONE', #38693 ) ;
#25819 = CARTESIAN_POINT ( 'NONE',  ( -9.245618777199831939, 19.45120513334818568, -24.74765325802571780 ) ) ;
#25820 = DIRECTION ( 'NONE',  ( 1.000000000000000000, 0.000000000000000000, -0.000000000000000000 ) ) ;
#25821 = FACE_BOUND ( 'NONE', #22871, .T. ) ;
#25822 = CARTESIAN_POINT ( 'NONE',  ( -20.69933004820033773, -5.104132961445666972, -25.75960008462992334 ) ) ;
#25823 = CARTESIAN_POINT ( 'NONE',  ( 3.610593701936712474, 31.83882289796390097, 10.50000000000000000 ) ) ;
#25824 = VERTEX_POINT ( 'NONE', #20009 ) ;
#25825 = CARTESIAN_POINT ( 'NONE',  ( 28.18869082171447005, 0.3296785013067420889, -12.55904125333466936 ) ) ;
#25826 = CARTESIAN_POINT ( 'NONE',  ( 14.36910708881319110, 26.64307479831611047, 10.76099332938163755 ) ) ;
#25827 = DIRECTION ( 'NONE',  ( 0.000000000000000000, 0.000000000000000000, 1.000000000000000000 ) ) ;
#25828 = AXIS2_PLACEMENT_3D ( 'NONE', #14305, #13906, #38692 ) ;
#25829 = EDGE_LOOP ( 'NONE', ( #19633, #15447 ) ) ;
#25830 = CARTESIAN_POINT ( 'NONE',  ( -20.81701148534373047, 0.8134213727834409546, -26.82927742226364032 ) ) ;
#25831 = CARTESIAN_POINT ( 'NONE',  ( 5.064564986133971658, 13.54338174056915456, 13.00000000000000178 ) ) ;
#25832 = ORIENTED_EDGE ( 'NONE', *, *, #16239, .F. ) ;
#25833 = CARTESIAN_POINT ( 'NONE',  ( 31.50878031485120090, -2.153655980402962467, -9.579608105637024806 ) ) ;
#25834 = CIRCLE ( 'NONE', #13500, 15.00000000000000000 ) ;
#25835 = CARTESIAN_POINT ( 'NONE',  ( 20.32885146017839517, -2.671174122295890907, -29.99999999999998224 ) ) ;
#25836 = CARTESIAN_POINT ( 'NONE',  ( 25.67968615518546827, -26.00921032235772046, 16.30093088680190760 ) ) ;
#25837 = VERTEX_POINT ( 'NONE', #28938 ) ;
#25838 = CARTESIAN_POINT ( 'NONE',  ( 7.110004120643233172, 37.89265721834169653, 15.13084544680205390 ) ) ;
#25839 = FACE_BOUND ( 'NONE', #37810, .T. ) ;
#25840 = CARTESIAN_POINT ( 'NONE',  ( 5.578133564216165574, 24.05045924978294991, 20.99999999999999645 ) ) ;
#25841 = CARTESIAN_POINT ( 'NONE',  ( 5.187504188494417079, 36.60991850771481637, 7.000000000000000000 ) ) ;
#25842 = CARTESIAN_POINT ( 'NONE',  ( -10.44103466624267185, 32.57396620494226624, 11.00000000000000000 ) ) ;
#25843 = AXIS2_PLACEMENT_3D ( 'NONE', #15629, #31268, #6277 ) ;
#25844 = AXIS2_PLACEMENT_3D ( 'NONE', #27038, #20551, #32944 ) ;
#25845 = FACE_BOUND ( 'NONE', #11655, .T. ) ;
#25846 = CARTESIAN_POINT ( 'NONE',  ( 15.42165057837873654, 26.78649484832369154, 16.30093088680190760 ) ) ;
#25847 = CARTESIAN_POINT ( 'NONE',  ( -19.61511227469957319, 7.169619886183266289, -25.45877017602282777 ) ) ;
#25848 = CARTESIAN_POINT ( 'NONE',  ( 12.77972917816505927, -16.04224856310990432, -29.27848096932829947 ) ) ;
#25849 = CARTESIAN_POINT ( 'NONE',  ( -13.29635151280775140, -18.15191941048946589, -20.55813556249457008 ) ) ;
#25850 = ORIENTED_EDGE ( 'NONE', *, *, #4376, .T. ) ;
#25851 = CARTESIAN_POINT ( 'NONE',  ( 11.56078434465998761, 19.03143594125964455, -22.71333681129807402 ) ) ;
#25852 = ORIENTED_EDGE ( 'NONE', *, *, #15094, .T. ) ;
#25853 = CARTESIAN_POINT ( 'NONE',  ( -14.80615464364070810, 23.19894269259860664, -12.60008722521619262 ) ) ;
#25854 = CARTESIAN_POINT ( 'NONE',  ( -21.42136340053371057, -21.87239718931726173, 19.99202127657076034 ) ) ;
#25855 = CARTESIAN_POINT ( 'NONE',  ( -1.400691654708310585, 37.43445890845833901, 7.000000000000000000 ) ) ;
#25856 = CARTESIAN_POINT ( 'NONE',  ( 12.69837305591254761, 20.98788295457261555, -18.46001444634856625 ) ) ;
#25857 = ORIENTED_EDGE ( 'NONE', *, *, #35332, .F. ) ;
#25858 = CARTESIAN_POINT ( 'NONE',  ( 19.27955278168219522, -10.63738015878406351, -24.21943841340187831 ) ) ;
#25859 = FACE_OUTER_BOUND ( 'NONE', #6255, .T. ) ;
#25860 = ORIENTED_EDGE ( 'NONE', *, *, #11618, .T. ) ;
#25862 = CARTESIAN_POINT ( 'NONE',  ( -10.10646936306323518, 32.94553861768095970, 7.500000000000004441 ) ) ;
#25861 = CARTESIAN_POINT ( 'NONE',  ( -14.96091455162279438, 26.58795068034906350, -8.747906387789663896 ) ) ;
#25863 = CARTESIAN_POINT ( 'NONE',  ( -9.695417275021851466, -18.21019213846330231, -28.07041747300570833 ) ) ;
#25864 = DIRECTION ( 'NONE',  ( 0.000000000000000000, 0.000000000000000000, -1.000000000000000000 ) ) ;
#25865 = ORIENTED_EDGE ( 'NONE', *, *, #6640, .T. ) ;
#25866 = CARTESIAN_POINT ( 'NONE',  ( -23.41415742069401773, -10.51963480729080835, -19.65694573768750786 ) ) ;
#25867 = CARTESIAN_POINT ( 'NONE',  ( -12.95131304720365328, -24.45778571613171692, -12.59044498358920272 ) ) ;
#25868 = LINE ( 'NONE', #10644, #5332 ) ;
#25869 = CARTESIAN_POINT ( 'NONE',  ( 16.18703989492556872, 19.32897852544927275, -13.73088434759361220 ) ) ;
#25870 = ORIENTED_EDGE ( 'NONE', *, *, #18697, .T. ) ;
#25871 = CARTESIAN_POINT ( 'NONE',  ( 21.71166764932993232, 3.770909521622002547, -21.95419646536155511 ) ) ;
#25872 = EDGE_CURVE ( 'NONE', #21859, #16360, #10292, .T. ) ;
#25873 = DIRECTION ( 'NONE',  ( -0.000000000000000000, -0.000000000000000000, -1.000000000000000000 ) ) ;
#25874 = DIRECTION ( 'NONE',  ( -0.000000000000000000, -0.000000000000000000, -1.000000000000000000 ) ) ;
#25875 = ORIENTED_EDGE ( 'NONE', *, *, #37956, .T. ) ;
#25876 = CARTESIAN_POINT ( 'NONE',  ( -30.36316148021155570, -0.1792145421230325053, -8.756721400621293228 ) ) ;
#25878 = CARTESIAN_POINT ( 'NONE',  ( 30.28562270265240031, -0.4997343038466697807, -9.672258859702814959 ) ) ;
#25877 = AXIS2_PLACEMENT_3D ( 'NONE', #20283, #11140, #4838 ) ;
#25879 = VECTOR ( 'NONE', #26570, 1000.000000000000000 ) ;
#25880 = EDGE_CURVE ( 'NONE', #14950, #2452, #1867, .T. ) ;
#25881 = CARTESIAN_POINT ( 'NONE',  ( 30.09689698601827246, -15.93509466225769344, 19.66345542862528362 ) ) ;
#25882 = ORIENTED_EDGE ( 'NONE', *, *, #28504, .T. ) ;
#25883 = EDGE_CURVE ( 'NONE', #35629, #26123, #26087, .T. ) ;
#25884 = CARTESIAN_POINT ( 'NONE',  ( -6.155076441694329326, 21.71698211341365337, -20.11584339644705111 ) ) ;
#25885 = CARTESIAN_POINT ( 'NONE',  ( 0.000000000000000000, 22.50000000000000355, 13.00000000000000178 ) ) ;
#25886 = DIRECTION ( 'NONE',  ( -0.9510565162951503115, 0.3090169943749573878, -0.000000000000000000 ) ) ;
#25887 = DIRECTION ( 'NONE',  ( 0.6691306063588662312, 0.7431448254773869166, 0.000000000000000000 ) ) ;
#25888 = LINE ( 'NONE', #13092, #6505 ) ;
#25889 = CARTESIAN_POINT ( 'NONE',  ( 11.81630298851978722, 31.79381426990546089, 10.50000000000000178 ) ) ;
#25890 = LINE ( 'NONE', #7812, #26297 ) ;
#25891 = EDGE_LOOP ( 'NONE', ( #4391, #1056, #2615, #5369, #34477, #6538, #14709, #26213 ) ) ;
#25892 = EDGE_CURVE ( 'NONE', #25343, #8719, #40128, .T. ) ;
#25893 = CARTESIAN_POINT ( 'NONE',  ( -6.557822374958133693, 35.99981354310120452, 10.49999999999999822 ) ) ;
#25894 = EDGE_CURVE ( 'NONE', #20361, #3606, #38831, .T. ) ;
#25895 = DIRECTION ( 'NONE',  ( 1.000000000000000000, 0.000000000000000000, 0.000000000000000000 ) ) ;
#25896 = CARTESIAN_POINT ( 'NONE',  ( 24.68240227516114871, -21.51021177795922412, -12.94802666595622398 ) ) ;
#25897 = DIRECTION ( 'NONE',  ( -0.4067366430757888285, 0.9135454576426059736, 0.000000000000000000 ) ) ;
#25898 = DIRECTION ( 'NONE',  ( 0.05233595624293101850, -0.9986295347545744994, -3.618009791163114596E-16 ) ) ;
#25899 = CARTESIAN_POINT ( 'NONE',  ( 14.59657937566097274, 26.31754401214214667, -10.13852064072044712 ) ) ;
#25900 = DIRECTION ( 'NONE',  ( 0.000000000000000000, 0.000000000000000000, 1.000000000000000000 ) ) ;
#25901 = AXIS2_PLACEMENT_3D ( 'NONE', #28946, #10464, #35658 ) ;
#25902 = ORIENTED_EDGE ( 'NONE', *, *, #23794, .T. ) ;
#25903 = CARTESIAN_POINT ( 'NONE',  ( -15.45883816434331592, 17.67526787779760866, -17.78974814387579428 ) ) ;
#25904 = CARTESIAN_POINT ( 'NONE',  ( -23.43324262027536875, -8.134040356058614307, 20.99999999999999645 ) ) ;
#25905 = CARTESIAN_POINT ( 'NONE',  ( 15.38966896450798316, -26.64286542733805163, -6.417027897479346876 ) ) ;
#25906 = CARTESIAN_POINT ( 'NONE',  ( -7.267999511062860130, 35.13630417120410954, 7.000000000000000000 ) ) ;
#25907 = CARTESIAN_POINT ( 'NONE',  ( 15.42339932183901752, 26.75673767418847859, -5.474198080818684531 ) ) ;
#25908 = ORIENTED_EDGE ( 'NONE', *, *, #28959, .T. ) ;
#25909 = CARTESIAN_POINT ( 'NONE',  ( 15.17329373222789357, 26.28549969035448086, -8.297710605404072126 ) ) ;
#25910 = AXIS2_PLACEMENT_3D ( 'NONE', #32097, #25796, #38193 ) ;
#25911 = B_SPLINE_SURFACE_WITH_KNOTS ( 'NONE', 1, 3, ( 
 ( #25371, #16648, #37771, #22324, #6878, #29030, #16439, #16243, #28625, #10342 ),
 ( #13384, #37971, #7080, #19478, #12590, #29232, #35737, #29832, #38575, #11150 ) ),
 .UNSPECIFIED., .F., .F., .F.,
 ( 2, 2 ),
 ( 4, 2, 2, 2, 4 ),
 ( 0.000000000000000000, 1.000000000000000000 ),
 ( 1.496612791730134617, 1.889311873428863198, 2.282010955127591778, 2.674710036826319914, 3.067409118525048495 ),
 .UNSPECIFIED. ) ;
#25912 = ORIENTED_EDGE ( 'NONE', *, *, #7716, .T. ) ;
#25914 = CARTESIAN_POINT ( 'NONE',  ( 14.14332487906622049, 26.04398259919119951, 10.49999999999999822 ) ) ;
#25913 = CARTESIAN_POINT ( 'NONE',  ( -11.07661461107485046, 17.64654016112482182, -26.82585402569723954 ) ) ;
#25915 = CARTESIAN_POINT ( 'NONE',  ( -14.92943112510105053, -25.97912449464955387, -9.238937178076628953 ) ) ;
#25916 = CARTESIAN_POINT ( 'NONE',  ( -29.80853493429716750, -25.87953118560963617, 12.73282698324867468 ) ) ;
#25917 = CARTESIAN_POINT ( 'NONE',  ( -32.94090784223518398, -19.89252564384590016, -5.855569924352811206 ) ) ;
#25918 = CARTESIAN_POINT ( 'NONE',  ( -6.958230700871959051, -24.96871470505583090, -7.888467374285714762 ) ) ;
#25919 = CARTESIAN_POINT ( 'NONE',  ( 11.71780135332492634, 17.71433433733627538, -25.06800478147926725 ) ) ;
#25920 = ORIENTED_EDGE ( 'NONE', *, *, #2563, .F. ) ;
#25921 = CARTESIAN_POINT ( 'NONE',  ( 23.41645241902980601, 8.181230565227640028, -10.35730366361351074 ) ) ;
#25922 = LINE ( 'NONE', #1351, #27082 ) ;
#25923 = CARTESIAN_POINT ( 'NONE',  ( -5.023663292579894524, -24.92826071503396790, -5.000000000000000888 ) ) ;
#25924 = CARTESIAN_POINT ( 'NONE',  ( -13.31085751088330760, 29.56957116847145173, 17.42190598798392998 ) ) ;
#25925 = ORIENTED_EDGE ( 'NONE', *, *, #8268, .T. ) ;
#25926 = CARTESIAN_POINT ( 'NONE',  ( -31.91632926199020659, -2.416287452245505118, -9.107245833971825633 ) ) ;
#25927 = ADVANCED_FACE ( 'NONE', ( #35239 ), #29146, .T. ) ;
#25928 = DIRECTION ( 'NONE',  ( 0.9510565162951504226, -0.3090169943749573322, 0.000000000000000000 ) ) ;
#25929 = VERTEX_POINT ( 'NONE', #24055 ) ;
#25930 = DIRECTION ( 'NONE',  ( -0.6691306063588576825, 0.7431448254773946882, 0.000000000000000000 ) ) ;
#25931 = FACE_OUTER_BOUND ( 'NONE', #5132, .T. ) ;
#25932 = CARTESIAN_POINT ( 'NONE',  ( 31.89048545145299585, -15.10830598425978266, -11.07426897462641513 ) ) ;
#25933 = CARTESIAN_POINT ( 'NONE',  ( 37.31659891191883105, -12.87518290988953495, 12.73282698324865514 ) ) ;
#25934 = AXIS2_PLACEMENT_3D ( 'NONE', #12463, #34011, #40092 ) ;
#25935 = VERTEX_POINT ( 'NONE', #14508 ) ;
#25936 = ORIENTED_EDGE ( 'NONE', *, *, #9033, .F. ) ;
#25937 = AXIS2_PLACEMENT_3D ( 'NONE', #12162, #3220, #36752 ) ;
#25938 = CARTESIAN_POINT ( 'NONE',  ( 12.03640989728592459, 29.14264673470096767, 13.00000000000000178 ) ) ;
#25939 = DIRECTION ( 'NONE',  ( 0.000000000000000000, 0.000000000000000000, 1.000000000000000000 ) ) ;
#25940 = CARTESIAN_POINT ( 'NONE',  ( 13.16028273094469192, 27.30176617939681449, 7.000000000000000000 ) ) ;
#25941 = ORIENTED_EDGE ( 'NONE', *, *, #32693, .F. ) ;
#25942 = CARTESIAN_POINT ( 'NONE',  ( -0.7005653291773012992, 35.42634926839502185, -11.06665404971477784 ) ) ;
#25943 = CARTESIAN_POINT ( 'NONE',  ( -14.98807736202308227, 21.89862425409926772, 7.338691926023216183 ) ) ;
#25944 = DIRECTION ( 'NONE',  ( -0.1045284632676436176, 0.9945218953682742891, 0.000000000000000000 ) ) ;
#25945 = EDGE_CURVE ( 'NONE', #17014, #27076, #12753, .T. ) ;
#25946 = PLANE ( 'NONE',  #714 ) ;
#25947 = DIRECTION ( 'NONE',  ( 0.000000000000000000, 0.000000000000000000, 1.000000000000000000 ) ) ;
#25948 = DIRECTION ( 'NONE',  ( -1.000000000000000000, 0.000000000000000000, 0.000000000000000000 ) ) ;
#25949 = CARTESIAN_POINT ( 'NONE',  ( 14.11003552855667209, 29.50458854998396419, -7.283368533493259633 ) ) ;
#25950 = FACE_OUTER_BOUND ( 'NONE', #5187, .T. ) ;
#25951 = EDGE_LOOP ( 'NONE', ( #26722, #36107, #2316, #15547 ) ) ;
#25953 = DIRECTION ( 'NONE',  ( -0.4999999999999933942, 0.8660254037844425934, 0.000000000000000000 ) ) ;
#25952 = CARTESIAN_POINT ( 'NONE',  ( -19.97103809025421484, 14.46599866876007034, -8.894276274733421417 ) ) ;
#25954 = DIRECTION ( 'NONE',  ( 0.000000000000000000, 0.000000000000000000, 1.000000000000000000 ) ) ;
#25955 = CARTESIAN_POINT ( 'NONE',  ( 10.57564039356294572, -19.56442984277105168, -22.72982311932152655 ) ) ;
#25956 = CARTESIAN_POINT ( 'NONE',  ( 9.343266739736582949, 17.68301270189218855, 10.50000000000000000 ) ) ;
#25957 = CARTESIAN_POINT ( 'NONE',  ( 15.31881962885621640, 26.68583777872107632, -6.886503466024833209 ) ) ;
#25958 = CARTESIAN_POINT ( 'NONE',  ( -3.091399026088746727, 22.35909668862748134, -29.99999999999999289 ) ) ;
#25959 = FACE_OUTER_BOUND ( 'NONE', #25817, .T. ) ;
#25960 = CARTESIAN_POINT ( 'NONE',  ( -19.03618297789652303, -16.83210767772735750, -19.74809521649639521 ) ) ;
#25961 = CARTESIAN_POINT ( 'NONE',  ( 5.670805767156023691, -19.83282806932450271, -28.23774505010902303 ) ) ;
#25962 = CARTESIAN_POINT ( 'NONE',  ( 12.48668498222315826, 20.36467295304646186, -19.51308572712811795 ) ) ;
#25963 = CARTESIAN_POINT ( 'NONE',  ( 17.14480940267289455, 11.33456439865563148, -28.29661424734811348 ) ) ;
#25964 = CARTESIAN_POINT ( 'NONE',  ( 0.5000000000000001110, 37.00000000000000711, 7.500000000000000888 ) ) ;
#25965 = CARTESIAN_POINT ( 'NONE',  ( -7.953812613386786801, 14.77701242934787906, 13.00000000000000178 ) ) ;
#25966 = EDGE_LOOP ( 'NONE', ( #12467, #35009, #3494, #11775 ) ) ;
#25967 = CIRCLE ( 'NONE', #16937, 6.000000000000003553 ) ;
#25968 = CARTESIAN_POINT ( 'NONE',  ( -9.332086639220589674, 35.22756758965231683, -6.737663000051229645 ) ) ;
#25969 = ORIENTED_EDGE ( 'NONE', *, *, #20447, .T. ) ;
#25970 = EDGE_CURVE ( 'NONE', #39380, #11229, #24561, .T. ) ;
#25971 = CYLINDRICAL_SURFACE ( 'NONE', #27392, 0.5000000000000001110 ) ;
#25972 = ORIENTED_EDGE ( 'NONE', *, *, #32494, .T. ) ;
#25973 = CARTESIAN_POINT ( 'NONE',  ( 27.75798668795975743, 0.1628108966169759808, -13.51197211289437305 ) ) ;
#25974 = EDGE_CURVE ( 'NONE', #39672, #2261, #15484, .T. ) ;
#25975 = CARTESIAN_POINT ( 'NONE',  ( 10.98647152928294446, 17.30743895948372213, -29.99999999999999289 ) ) ;
#25976 = EDGE_CURVE ( 'NONE', #30884, #13873, #22599, .T. ) ;
#25977 = CARTESIAN_POINT ( 'NONE',  ( -12.30736835487442704, 14.81698729810789672, 7.000000000000000000 ) ) ;
#25978 = ORIENTED_EDGE ( 'NONE', *, *, #22480, .T. ) ;
#25979 = CARTESIAN_POINT ( 'NONE',  ( -29.26835155205951366, 0.1731288304656850296, -10.65622225438751691 ) ) ;
#25980 = ORIENTED_EDGE ( 'NONE', *, *, #15553, .T. ) ;
#25981 = CARTESIAN_POINT ( 'NONE',  ( 24.30836135983651758, -6.551983109444438291, -19.83190686569865946 ) ) ;
#25982 = AXIS2_PLACEMENT_3D ( 'NONE', #34794, #34592, #3313 ) ;
#25983 = ADVANCED_FACE ( 'NONE', ( #8212 ), #21205, .T. ) ;
#25984 = CIRCLE ( 'NONE', #21469, 6.000000000000001776 ) ;
#25985 = ORIENTED_EDGE ( 'NONE', *, *, #5517, .F. ) ;
#25986 = DIRECTION ( 'NONE',  ( -0.4999999999999919509, -0.8660254037844432595, 0.000000000000000000 ) ) ;
#25987 = CARTESIAN_POINT ( 'NONE',  ( 12.44178368932906409, 35.65276919561902957, 11.55979286843929543 ) ) ;
#25988 = LINE ( 'NONE', #35142, #6706 ) ;
#25989 = DIRECTION ( 'NONE',  ( -0.6293203910498448295, -0.7771459614569649066, 0.000000000000000000 ) ) ;
#25990 = CARTESIAN_POINT ( 'NONE',  ( 13.83280510892147674, 26.34487040058358076, 17.92354375535250810 ) ) ;
#25991 = CYLINDRICAL_SURFACE ( 'NONE', #27201, 6.000000000000015987 ) ;
#25992 = ORIENTED_EDGE ( 'NONE', *, *, #22920, .F. ) ;
#25993 = DIRECTION ( 'NONE',  ( 0.2876062384759449642, -0.6459741880212592768, -0.7071067811865424657 ) ) ;
#25994 = CARTESIAN_POINT ( 'NONE',  ( 40.48557158514985588, -11.25000000000009415, 3.000000000000000000 ) ) ;
#25995 = CIRCLE ( 'NONE', #30548, 6.000000000000003553 ) ;
#25996 = ADVANCED_FACE ( 'NONE', ( #30559 ), #33216, .T. ) ;
#25997 = FACE_OUTER_BOUND ( 'NONE', #23380, .T. ) ;
#25998 = EDGE_CURVE ( 'NONE', #6337, #22892, #15211, .T. ) ;
#25999 = CARTESIAN_POINT ( 'NONE',  ( 14.27219392008591292, 14.71651433334269043, -30.00000000000000711 ) ) ;
#26000 = CARTESIAN_POINT ( 'NONE',  ( 10.72270391973751558, 33.55271709729109375, -8.067294441686739148 ) ) ;
#26001 = VERTEX_POINT ( 'NONE', #30755 ) ;
#26002 = CARTESIAN_POINT ( 'NONE',  ( 8.137585970692077453, 29.15429895402930072, 10.00000000000000000 ) ) ;
#26003 = DIRECTION ( 'NONE',  ( 0.000000000000000000, 0.000000000000000000, 1.000000000000000000 ) ) ;
#26004 = CARTESIAN_POINT ( 'NONE',  ( 12.10068356543891710, -20.90411770709192041, -19.42675082364999639 ) ) ;
#26005 = CARTESIAN_POINT ( 'NONE',  ( 3.456468065140018808, 26.15323006594238464, 20.99999999999998934 ) ) ;
#26006 = LINE ( 'NONE', #1639, #1680 ) ;
#26007 = EDGE_LOOP ( 'NONE', ( #6139, #28006, #26622, #23144 ) ) ;
#26008 = CARTESIAN_POINT ( 'NONE',  ( -14.03186475831749647, 23.92943759979809570, -13.51384694048713619 ) ) ;
#26009 = AXIS2_PLACEMENT_3D ( 'NONE', #1675, #4920, #35803 ) ;
#26010 = CARTESIAN_POINT ( 'NONE',  ( -35.14638740386807569, -7.516303343519180835, 16.30093088680109048 ) ) ;
#26011 = CARTESIAN_POINT ( 'NONE',  ( 9.462549223031706092, -18.54705810577948455, -26.84942688299948799 ) ) ;
#26012 = CIRCLE ( 'NONE', #27962, 1.000000000000000000 ) ;
#26013 = LINE ( 'NONE', #10789, #1065 ) ;
#26014 = ORIENTED_EDGE ( 'NONE', *, *, #31965, .F. ) ;
#26015 = ORIENTED_EDGE ( 'NONE', *, *, #22456, .T. ) ;
#26016 = CARTESIAN_POINT ( 'NONE',  ( -8.851921390983532589, 18.49121495627866452, -29.30371079639624909 ) ) ;
#26017 = CARTESIAN_POINT ( 'NONE',  ( -13.16997834948020873, -17.85564821404134150, -23.48525574773325886 ) ) ;
#26018 = EDGE_CURVE ( 'NONE', #37387, #42, #2327, .T. ) ;
#26019 = FACE_BOUND ( 'NONE', #14413, .T. ) ;
#26020 = CARTESIAN_POINT ( 'NONE',  ( -28.17101914744512925, -6.941970696622886905, -15.85777330802162055 ) ) ;
#26021 = CARTESIAN_POINT ( 'NONE',  ( -4.984135866956334482, 36.15314577889358105, 7.500000000000000888 ) ) ;
#26022 = ORIENTED_EDGE ( 'NONE', *, *, #24763, .T. ) ;
#26023 = CARTESIAN_POINT ( 'NONE',  ( 25.78250412838150041, 0.4551448022510044544, -16.45580364150897879 ) ) ;
#26024 = ADVANCED_FACE ( 'NONE', ( #2915 ), #15306, .F. ) ;
#26025 = CARTESIAN_POINT ( 'NONE',  ( 14.32492426577155165, 24.55152792996899080, -12.54456079180045514 ) ) ;
#26026 = CYLINDRICAL_SURFACE ( 'NONE', #10216, 0.5000000000000006661 ) ;
#26027 = AXIS2_PLACEMENT_3D ( 'NONE', #35099, #38750, #4011 ) ;
#26028 = EDGE_LOOP ( 'NONE', ( #130, #2299, #6031, #38237 ) ) ;
#26029 = CARTESIAN_POINT ( 'NONE',  ( -29.37198519057492163, 0.05438766727590542416, -10.65228692739096594 ) ) ;
#26030 = CARTESIAN_POINT ( 'NONE',  ( -5.644276917315582232, 36.40655018617695760, 10.59344459855552678 ) ) ;
#26031 = EDGE_LOOP ( 'NONE', ( #24146, #2427, #15671, #35994 ) ) ;
#26032 = CARTESIAN_POINT ( 'NONE',  ( 22.03578752383834072, -1.794605797681862791, -23.55611175985229266 ) ) ;
#26033 = EDGE_CURVE ( 'NONE', #26924, #21498, #20815, .T. ) ;
#26034 = CARTESIAN_POINT ( 'NONE',  ( 20.32145253026429188, 2.784070299583892183, -30.00000000000000000 ) ) ;
#26035 = CARTESIAN_POINT ( 'NONE',  ( 36.43809855126006880, -10.93713533239221825, 15.13084544680210364 ) ) ;
#26036 = VERTEX_POINT ( 'NONE', #11669 ) ;
#26037 = CARTESIAN_POINT ( 'NONE',  ( -1.474891194420403403E-13, 38.97445513318768207, 15.72805884748939498 ) ) ;
#26038 = CARTESIAN_POINT ( 'NONE',  ( 4.276346332578968397E-14, -21.80712738496724157, 18.87996532025784902 ) ) ;
#26039 = DIRECTION ( 'NONE',  ( 1.000000000000000000, 0.000000000000000000, 0.000000000000000000 ) ) ;
#26040 = CARTESIAN_POINT ( 'NONE',  ( -1.082972213713723431, 27.41125570341915463, 20.99999999999999645 ) ) ;
#26041 = VECTOR ( 'NONE', #9524, 1000.000000000000000 ) ;
#26042 = LINE ( 'NONE', #25841, #4463 ) ;
#26043 = AXIS2_PLACEMENT_3D ( 'NONE', #29645, #32709, #29248 ) ;
#26044 = FACE_OUTER_BOUND ( 'NONE', #39202, .T. ) ;
#26045 = EDGE_CURVE ( 'NONE', #10818, #6396, #1220, .T. ) ;
#26046 = CARTESIAN_POINT ( 'NONE',  ( -2.629601561899595374, 7.723830143584053509, 10.49999999999999822 ) ) ;
#26047 = CARTESIAN_POINT ( 'NONE',  ( 31.51573171626900205, 0.5582143012820769412, 15.13084544680213739 ) ) ;
#26048 = CARTESIAN_POINT ( 'NONE',  ( -18.97876558365113553, 7.800091065717492889, -28.85243984144211993 ) ) ;
#26049 = AXIS2_PLACEMENT_3D ( 'NONE', #20547, #32940, #26830 ) ;
#26050 = CARTESIAN_POINT ( 'NONE',  ( 20.56439459974750150, -26.83426525695362130, -7.688853040980692555 ) ) ;
#26051 = CARTESIAN_POINT ( 'NONE',  ( 9.806975420853749625, 31.15003855377755571, 12.00000000000000000 ) ) ;
#26052 = ORIENTED_EDGE ( 'NONE', *, *, #11413, .T. ) ;
#26053 = CARTESIAN_POINT ( 'NONE',  ( 11.08031616781238782, 17.83112152660168093, -26.21360684684639963 ) ) ;
#26054 = ORIENTED_EDGE ( 'NONE', *, *, #19201, .F. ) ;
#26055 = CARTESIAN_POINT ( 'NONE',  ( -11.76523398598002323, 16.92967342931978791, -28.11894497090000300 ) ) ;
#26056 = CARTESIAN_POINT ( 'NONE',  ( -16.60464863832889648, -22.41657912773201744, 19.66345542862528362 ) ) ;
#26057 = CARTESIAN_POINT ( 'NONE',  ( 10.73132186042472469, 32.83534196859159238, 10.82238861112332273 ) ) ;
#26058 = CARTESIAN_POINT ( 'NONE',  ( 11.12516802696661067, 17.46729153672471924, -27.45183205712903884 ) ) ;
#26059 = ORIENTED_EDGE ( 'NONE', *, *, #9312, .T. ) ;
#26060 = CARTESIAN_POINT ( 'NONE',  ( 19.98779029393962503, -11.02768449253182403, -22.98586908969943110 ) ) ;
#26061 = FACE_OUTER_BOUND ( 'NONE', #2220, .T. ) ;
#26062 = ORIENTED_EDGE ( 'NONE', *, *, #11983, .T. ) ;
#26064 = DIRECTION ( 'NONE',  ( 0.1045284632676570929, 0.9945218953682730678, 0.000000000000000000 ) ) ;
#26063 = CARTESIAN_POINT ( 'NONE',  ( -14.83546550674832432, 26.53435752211777299, -9.210659735667860559 ) ) ;
#26065 = CARTESIAN_POINT ( 'NONE',  ( -14.70647767559404784, -24.71655422085136777, -12.49785459478513161 ) ) ;
#26066 = CARTESIAN_POINT ( 'NONE',  ( 13.53204082366770855, 16.02694346567353634, 7.203056206335837430 ) ) ;
#26067 = ORIENTED_EDGE ( 'NONE', *, *, #13339, .T. ) ;
#26068 = CARTESIAN_POINT ( 'NONE',  ( -35.14568626021495845, -14.53237387118475610, -5.437296911868972238 ) ) ;
#26069 = CARTESIAN_POINT ( 'NONE',  ( -9.443825133297737651, -18.71410463014245096, -26.25643312767523341 ) ) ;
#26070 = CARTESIAN_POINT ( 'NONE',  ( -12.01838097023000529, 23.73363068877903359, 6.000000000000000000 ) ) ;
#26071 = CARTESIAN_POINT ( 'NONE',  ( 13.25821341800907227, 15.76719205175851002, -28.19245977045222773 ) ) ;
#26072 = EDGE_LOOP ( 'NONE', ( #40022, #25262, #17670, #28791 ) ) ;
#26073 = CARTESIAN_POINT ( 'NONE',  ( 27.88619785758654857, 2.892813575489728173, -7.853246008088212271 ) ) ;
#26074 = ADVANCED_FACE ( 'NONE', ( #6350 ), #12896, .T. ) ;
#26075 = DIRECTION ( 'NONE',  ( 0.000000000000000000, 0.000000000000000000, 1.000000000000000000 ) ) ;
#26076 = CARTESIAN_POINT ( 'NONE',  ( -35.27625572565145973, 1.213838575764629946, 23.00000000000000000 ) ) ;
#26077 = VERTEX_POINT ( 'NONE', #10006 ) ;
#26078 = CARTESIAN_POINT ( 'NONE',  ( -20.49112616741955506, 0.6095660351776287511, -29.99999999999999645 ) ) ;
#26079 = CARTESIAN_POINT ( 'NONE',  ( 30.84690724597788858, -0.7292977086491185812, -8.727067712974493574 ) ) ;
#26080 = CARTESIAN_POINT ( 'NONE',  ( 28.20105441993420925, -17.62361288429907447, 19.99202127657103389 ) ) ;
#26081 = ORIENTED_EDGE ( 'NONE', *, *, #38926, .F. ) ;
#26082 = AXIS2_PLACEMENT_3D ( 'NONE', #27542, #17821, #27737 ) ;
#26083 = CARTESIAN_POINT ( 'NONE',  ( -20.48369986121767283, 1.531721084589908966, -28.72957500320905311 ) ) ;
#26084 = CARTESIAN_POINT ( 'NONE',  ( -22.40982762235196191, 2.618079236897031148, -29.99999999999999645 ) ) ;
#26085 = FACE_OUTER_BOUND ( 'NONE', #5770, .T. ) ;
#26086 = CIRCLE ( 'NONE', #807, 0.4999999999999986122 ) ;
#26087 = LINE ( 'NONE', #10866, #16114 ) ;
#26088 = AXIS2_PLACEMENT_3D ( 'NONE', #21007, #2323, #11464 ) ;
#26089 = CARTESIAN_POINT ( 'NONE',  ( 12.41947502333593967, 43.35441443594645250, 7.500000000000000888 ) ) ;
#26090 = DIRECTION ( 'NONE',  ( 1.000000000000000000, 0.000000000000000000, 0.000000000000000000 ) ) ;
#26091 = CIRCLE ( 'NONE', #31300, 0.5000000000000000000 ) ;
#26092 = DIRECTION ( 'NONE',  ( -0.9510565162951504226, 0.3090169943749573322, 0.000000000000000000 ) ) ;
#26093 = EDGE_CURVE ( 'NONE', #20959, #39797, #16150, .T. ) ;
#26094 = EDGE_LOOP ( 'NONE', ( #6874, #36611, #31756, #29627 ) ) ;
#26095 = CARTESIAN_POINT ( 'NONE',  ( -6.843305518951122046, 35.42677428760902103, 10.49999999999999822 ) ) ;
#26096 = DIRECTION ( 'NONE',  ( 0.000000000000000000, 0.000000000000000000, 1.000000000000000000 ) ) ;
#26097 = CARTESIAN_POINT ( 'NONE',  ( 27.17408060449223228, -25.06914451978216718, -6.725518816324792759 ) ) ;
#26098 = ADVANCED_FACE ( 'NONE', ( #9615 ), #9811, .T. ) ;
#26099 = FACE_OUTER_BOUND ( 'NONE', #10019, .T. ) ;
#26100 = DIRECTION ( 'NONE',  ( -0.6724985119639614872, -0.2185080122244129619, -0.7071067811865427988 ) ) ;
#26101 = CARTESIAN_POINT ( 'NONE',  ( 11.77932827439872199, 20.33358996693879561, -20.47140772640445050 ) ) ;
#26102 = FACE_OUTER_BOUND ( 'NONE', #28824, .T. ) ;
#26103 = ORIENTED_EDGE ( 'NONE', *, *, #39545, .F. ) ;
#26104 = CARTESIAN_POINT ( 'NONE',  ( -17.34987630490782351, 20.70268335502479928, -6.910411782773334011 ) ) ;
#26105 = CARTESIAN_POINT ( 'NONE',  ( -19.30730118283918628, -16.27608008926400274, 20.99999999999999645 ) ) ;
#26106 = VECTOR ( 'NONE', #1955, 1000.000000000000000 ) ;
#26107 = CARTESIAN_POINT ( 'NONE',  ( 12.20016556335618141, -22.02549961372093179, -17.44539159223752378 ) ) ;
#26108 = EDGE_CURVE ( 'NONE', #29599, #21075, #24590, .T. ) ;
#26109 = CARTESIAN_POINT ( 'NONE',  ( 14.35088184066152373, 20.32132268570678235, 10.83333333333333393 ) ) ;
#26110 = CARTESIAN_POINT ( 'NONE',  ( 13.77648659466977854, 23.38131483086550944, -14.47688990636883943 ) ) ;
#26111 = EDGE_LOOP ( 'NONE', ( #5898, #24481, #31556 ) ) ;
#26112 = CARTESIAN_POINT ( 'NONE',  ( 10.97760868008098889, 17.31306259807076131, -30.00000000000000000 ) ) ;
#26113 = B_SPLINE_CURVE_WITH_KNOTS ( 'NONE', 3,
 ( #20045, #10092, #13331, #38117, #35277, #7229, #10289, #19630, #4393, #16798, #32026, #4191, #10696, #7639, #32440, #30189, #18202, #8246 ),
 .UNSPECIFIED., .F., .F.,
 ( 4, 2, 2, 2, 2, 2, 2, 2, 4 ),
 ( 0.2985673197444002613, 0.3862464047763500274, 0.4739254898082998491, 0.5616045748402497262, 0.6492836598721997143, 0.7369627449041498135, 0.8246418299360998017, 0.9123209149680500119, 1.000000000000000000 ),
 .UNSPECIFIED. ) ;
#26114 = VERTEX_POINT ( 'NONE', #6943 ) ;
#26116 = DIRECTION ( 'NONE',  ( 1.000000000000000000, 0.000000000000000000, 0.000000000000000000 ) ) ;
#26115 = CARTESIAN_POINT ( 'NONE',  ( -15.39213581000993436, 26.86843326188214576, -5.473789308097052775 ) ) ;
#26117 = CARTESIAN_POINT ( 'NONE',  ( -14.70529695197427422, -25.64556149301234456, -10.18130632746762920 ) ) ;
#26118 = CARTESIAN_POINT ( 'NONE',  ( -20.78821643698927701, -29.20280246618805720, 11.00000000000000000 ) ) ;
#26119 = AXIS2_PLACEMENT_3D ( 'NONE', #33982, #5940, #39865 ) ;
#26120 = CARTESIAN_POINT ( 'NONE',  ( -17.43379632413495983, -11.24738337999374593, -27.70877160700983310 ) ) ;
#26121 = CARTESIAN_POINT ( 'NONE',  ( -2.301023503631009159, -23.23531080007942506, -14.91665611832322114 ) ) ;
#26122 = CARTESIAN_POINT ( 'NONE',  ( 14.30052602520593474, 22.28094600777651380, -14.54308252804225887 ) ) ;
#26123 = VERTEX_POINT ( 'NONE', #40082 ) ;
#26124 = CARTESIAN_POINT ( 'NONE',  ( 18.97764795543955785, 8.024778375806581820, -27.72202992318708681 ) ) ;
#26125 = CARTESIAN_POINT ( 'NONE',  ( 8.437494178870114325, 40.76200630940460456, 11.00000000000000178 ) ) ;
#26126 = CARTESIAN_POINT ( 'NONE',  ( 10.13720066964783939, -25.55706996539716513, -5.000000000000003553 ) ) ;
#26127 = CARTESIAN_POINT ( 'NONE',  ( 12.85888779259182968, 31.22252129899190720, 16.87380292611442201 ) ) ;
#26128 = ORIENTED_EDGE ( 'NONE', *, *, #28134, .F. ) ;
#26129 = CARTESIAN_POINT ( 'NONE',  ( -25.45953608835651139, -1.714497824024611594, -18.18611588942592405 ) ) ;
#26130 = CARTESIAN_POINT ( 'NONE',  ( -10.32009510687426435, 12.89643020662261108, 20.94377226548379056 ) ) ;
#26131 = CIRCLE ( 'NONE', #71, 0.4999999999999997780 ) ;
#26132 = EDGE_LOOP ( 'NONE', ( #23434, #63, #7495, #38839 ) ) ;
#26133 = DIRECTION ( 'NONE',  ( 1.000000000000000000, 0.000000000000000000, 0.000000000000000000 ) ) ;
#26134 = CARTESIAN_POINT ( 'NONE',  ( 8.339609403135806787, 11.87216320208440123, 9.500000000000000000 ) ) ;
#26135 = EDGE_CURVE ( 'NONE', #34064, #39672, #18951, .T. ) ;
#26136 = CARTESIAN_POINT ( 'NONE',  ( 34.95664498758854677, -15.33017443246186495, -5.436732254870795700 ) ) ;
#26137 = CONICAL_SURFACE ( 'NONE', #24838, 1.000000000000007772, 0.7853981633974557175 ) ;
#26138 = CARTESIAN_POINT ( 'NONE',  ( 37.34232268491259532, -8.983628415038312554, 11.55979286843934872 ) ) ;
#26139 = VECTOR ( 'NONE', #31500, 1000.000000000000114 ) ;
#26140 = ORIENTED_EDGE ( 'NONE', *, *, #38418, .T. ) ;
#26141 = CARTESIAN_POINT ( 'NONE',  ( 8.118377661053324701, 10.47536095541698486, 9.000000000000001776 ) ) ;
#26142 = CYLINDRICAL_SURFACE ( 'NONE', #33141, 1.000000000000000000 ) ;
#26143 = AXIS2_PLACEMENT_3D ( 'NONE', #23266, #20827, #20425 ) ;
#26144 = DIRECTION ( 'NONE',  ( 0.7431448254773962425, 0.6691306063588561281, 0.000000000000000000 ) ) ;
#26145 = ORIENTED_EDGE ( 'NONE', *, *, #24142, .F. ) ;
#26146 = CARTESIAN_POINT ( 'NONE',  ( -0.7484310965467956267, 38.13046687410084701, -7.116911809159399027 ) ) ;
#26147 = CARTESIAN_POINT ( 'NONE',  ( -13.93689154498694904, 28.04681619138562709, 7.338691926023206413 ) ) ;
#26148 = EDGE_CURVE ( 'NONE', #31785, #8550, #21963, .T. ) ;
#26149 = DIRECTION ( 'NONE',  ( 1.000000000000000000, 0.000000000000000000, 0.000000000000000000 ) ) ;
#26150 = CARTESIAN_POINT ( 'NONE',  ( 14.47283171447379146, 21.48159823030312054, 11.00000000000000000 ) ) ;
#26151 = CARTESIAN_POINT ( 'NONE',  ( -19.48557158514982390, 33.75000000000009948, 11.00000000000000000 ) ) ;
#26152 = VECTOR ( 'NONE', #8068, 1000.000000000000000 ) ;
#26153 = DIRECTION ( 'NONE',  ( -0.000000000000000000, -0.000000000000000000, -1.000000000000000000 ) ) ;
#26154 = CARTESIAN_POINT ( 'NONE',  ( 10.62820802463951964, 21.51424845583950685, -20.27260820117726681 ) ) ;
#26155 = CARTESIAN_POINT ( 'NONE',  ( -12.69371393710745011, 14.59393057220544776, 10.76099332938163933 ) ) ;
#26156 = ORIENTED_EDGE ( 'NONE', *, *, #21487, .T. ) ;
#26158 = FACE_OUTER_BOUND ( 'NONE', #14894, .T. ) ;
#26157 = CARTESIAN_POINT ( 'NONE',  ( -19.36646015756375760, 13.94833338277440582, -12.87628227385044433 ) ) ;
#26159 = CLOSED_SHELL ( 'NONE', ( #35204, #35647, #1730, #6258, #12387, #7373, #28137, #23807, #4885, #21893, #20744, #27980, #4681, #11590, #37536, #8741, #27444, #24263, #25219, #14998, #11270, #4797, #31707, #25250, #38691, #33970, #21410, #24302, #34954 ) ) ;
#26160 = EDGE_CURVE ( 'NONE', #37653, #13704, #25222, .T. ) ;
#26161 = CARTESIAN_POINT ( 'NONE',  ( -0.4999999999999998890, 37.47223625998407925, 10.68306085400112693 ) ) ;
#26162 = CARTESIAN_POINT ( 'NONE',  ( 15.19304689221615412, -26.28704695153315285, -8.297102716332286576 ) ) ;
#26163 = ADVANCED_FACE ( 'NONE', ( #18759 ), #11631, .T. ) ;
#26164 = DIRECTION ( 'NONE',  ( 0.000000000000000000, 0.000000000000000000, 1.000000000000000000 ) ) ;
#26165 = CARTESIAN_POINT ( 'NONE',  ( 15.15493471932264491, 26.34784287548288262, -8.295283454795825406 ) ) ;
#26166 = CARTESIAN_POINT ( 'NONE',  ( -11.31392148919591811, 36.91540483778867099, -14.26382729546508088 ) ) ;
#26167 = CARTESIAN_POINT ( 'NONE',  ( -24.27952205336340441, -12.77208933892361209, 23.00000000000000711 ) ) ;
#26168 = CIRCLE ( 'NONE', #24894, 1.000000000000000000 ) ;
#26169 = CARTESIAN_POINT ( 'NONE',  ( -25.14789180526689805, -22.31687521175224376, -12.03118656357111860 ) ) ;
#26170 = CARTESIAN_POINT ( 'NONE',  ( 7.832614783866235442, -20.65680624402197907, -21.94422844697728792 ) ) ;
#26171 = CARTESIAN_POINT ( 'NONE',  ( 12.83367166058087072, 20.79141030706715298, -18.48305212125895736 ) ) ;
#26172 = CARTESIAN_POINT ( 'NONE',  ( 18.62263446944652046, 13.67603366424814837, -15.92850824050840863 ) ) ;
#26173 = CARTESIAN_POINT ( 'NONE',  ( 3.813962023474619212, 32.29559562678521445, 11.00000000000000000 ) ) ;
#26174 = CARTESIAN_POINT ( 'NONE',  ( -24.08646667827941457, -13.28101593840491468, 21.00000000000000000 ) ) ;
#26175 = ORIENTED_EDGE ( 'NONE', *, *, #1074, .T. ) ;
#26176 = CARTESIAN_POINT ( 'NONE',  ( -7.058933474767617788, 34.49725963336143764, -10.22158782810721256 ) ) ;
#26177 = ORIENTED_EDGE ( 'NONE', *, *, #38814, .F. ) ;
#26178 = CARTESIAN_POINT ( 'NONE',  ( -14.82146137012738940, -25.95528464061796825, -9.240260087632112374 ) ) ;
#26179 = DIRECTION ( 'NONE',  ( 0.1045284632676436454, -0.9945218953682745111, 0.000000000000000000 ) ) ;
#26180 = EDGE_LOOP ( 'NONE', ( #22486, #31683, #32377, #15636 ) ) ;
#26181 = CARTESIAN_POINT ( 'NONE',  ( -4.188939243032556270, 44.61227686191953268, 11.00000000000000000 ) ) ;
#26182 = EDGE_CURVE ( 'NONE', #34284, #39323, #34396, .T. ) ;
#26183 = CARTESIAN_POINT ( 'NONE',  ( -31.94006737154284892, 0.9747213384881107112, 13.92931973827808534 ) ) ;
#26184 = ADVANCED_FACE ( 'NONE', ( #37244 ), #37043, .F. ) ;
#26185 = ORIENTED_EDGE ( 'NONE', *, *, #2867, .T. ) ;
#26186 = CARTESIAN_POINT ( 'NONE',  ( -20.47826699597012023, 0.9446083685552518761, -29.34992276858810811 ) ) ;
#26187 = ORIENTED_EDGE ( 'NONE', *, *, #7884, .F. ) ;
#26188 = CARTESIAN_POINT ( 'NONE',  ( 20.72580500889552013, -4.914281886810445421, -25.77267062739201364 ) ) ;
#26189 = AXIS2_PLACEMENT_3D ( 'NONE', #1887, #23000, #14059 ) ;
#26190 = ORIENTED_EDGE ( 'NONE', *, *, #36357, .T. ) ;
#26191 = DIRECTION ( 'NONE',  ( 1.000000000000000000, 0.000000000000000000, 0.000000000000000000 ) ) ;
#26192 = CARTESIAN_POINT ( 'NONE',  ( 17.34253826607184834, 27.32041144404034938, 11.00000000000000178 ) ) ;
#26193 = CARTESIAN_POINT ( 'NONE',  ( 13.01837422881150452, 21.26636931122159169, 13.00000000000000178 ) ) ;
#26194 = LINE ( 'NONE', #7503, #11708 ) ;
#26195 = CARTESIAN_POINT ( 'NONE',  ( 2.974899668820615073, 35.98612526451933746, 18.42518152272109333 ) ) ;
#26196 = CIRCLE ( 'NONE', #6721, 0.5000000000000004441 ) ;
#26197 = DIRECTION ( 'NONE',  ( -0.000000000000000000, -0.000000000000000000, -1.000000000000000000 ) ) ;
#26198 = ORIENTED_EDGE ( 'NONE', *, *, #17114, .F. ) ;
#26199 = CARTESIAN_POINT ( 'NONE',  ( -15.93611613685307482, -12.91202363157417565, -30.00000000000004263 ) ) ;
#26200 = CARTESIAN_POINT ( 'NONE',  ( -2.629601561899596263, 7.723830143584054397, 10.63089969389957012 ) ) ;
#26201 = DIRECTION ( 'NONE',  ( 0.8660254037844364872, -0.5000000000000038858, 0.000000000000000000 ) ) ;
#26202 = EDGE_CURVE ( 'NONE', #26207, #37486, #27895, .T. ) ;
#26203 = CARTESIAN_POINT ( 'NONE',  ( 18.59382115548298131, 17.96292538557851515, -5.000000000000004441 ) ) ;
#26204 = CARTESIAN_POINT ( 'NONE',  ( 8.607820399192389615, 29.73311969603586746, -13.95432102836428889 ) ) ;
#26205 =( REPRESENTATION_RELATIONSHIP ('NONE','NONE', #15382, #28068 ) REPRESENTATION_RELATIONSHIP_WITH_TRANSFORMATION ( #26796 )SHAPE_REPRESENTATION_RELATIONSHIP( ) );
#26206 = VECTOR ( 'NONE', #3752, 1000.000000000000000 ) ;
#26207 = VERTEX_POINT ( 'NONE', #69 ) ;
#26208 = CARTESIAN_POINT ( 'NONE',  ( -8.806982162272252168, 13.84996144622306247, 12.00000000000000000 ) ) ;
#26209 = CARTESIAN_POINT ( 'NONE',  ( 4.100636323082810009, 29.29593658752792962, 13.00000000000000178 ) ) ;
#26210 = CARTESIAN_POINT ( 'NONE',  ( 16.27219429315636390, -26.92618254030204383, -5.470502546158905410 ) ) ;
#26211 = CARTESIAN_POINT ( 'NONE',  ( -14.36830325120615903, 20.48707633493503621, 11.00000000000000000 ) ) ;
#26212 = FACE_OUTER_BOUND ( 'NONE', #27571, .T. ) ;
#26213 = ORIENTED_EDGE ( 'NONE', *, *, #19067, .F. ) ;
#26214 = CARTESIAN_POINT ( 'NONE',  ( -12.64541957868966193, 21.06527240651957200, -18.45049806135583736 ) ) ;
#26215 = CIRCLE ( 'NONE', #21695, 1.000000000000000000 ) ;
#26216 = CARTESIAN_POINT ( 'NONE',  ( -33.89025995733841512, -4.271010277521935627, 16.30093088680190405 ) ) ;
#26217 = CARTESIAN_POINT ( 'NONE',  ( 13.95335475392358759, -25.00100328124352345, -11.61047761660894118 ) ) ;
#26218 = CARTESIAN_POINT ( 'NONE',  ( -9.584141256673788689, 10.96086782047184727, 7.338980292232258229 ) ) ;
#26219 = ORIENTED_EDGE ( 'NONE', *, *, #21554, .F. ) ;
#26220 = VERTEX_POINT ( 'NONE', #12656 ) ;
#26221 = CARTESIAN_POINT ( 'NONE',  ( -12.42600970353487533, 29.09350466320093531, -11.32961783136679657 ) ) ;
#26222 = DIRECTION ( 'NONE',  ( 0.1045284632676436593, -0.9945218953682742891, 0.000000000000000000 ) ) ;
#26223 = CARTESIAN_POINT ( 'NONE',  ( -12.64565515434644105, 14.62167732336942194, 10.82238861112330675 ) ) ;
#26224 = AXIS2_PLACEMENT_3D ( 'NONE', #528, #28553, #19207 ) ;
#26225 = CARTESIAN_POINT ( 'NONE',  ( -34.94942070055063255, -7.655693536555084222, -6.319957789537046899 ) ) ;
#26226 = DIRECTION ( 'NONE',  ( 1.000000000000000000, 0.000000000000000000, 0.000000000000000000 ) ) ;
#26227 = VERTEX_POINT ( 'NONE', #28294 ) ;
#26228 = CARTESIAN_POINT ( 'NONE',  ( 22.17991941591415639, 0.8307563611647147406, -22.75514243441729789 ) ) ;
#26229 = CARTESIAN_POINT ( 'NONE',  ( -10.32110986824222110, 33.06327772184317126, 10.49999999999999822 ) ) ;
#26230 = CYLINDRICAL_SURFACE ( 'NONE', #36911, 0.5000000000000004441 ) ;
#26231 = CARTESIAN_POINT ( 'NONE',  ( 12.05736835487432579, 14.38397459621550567, 7.499999999999997335 ) ) ;
#26232 = ORIENTED_EDGE ( 'NONE', *, *, #2234, .T. ) ;
#26233 = CARTESIAN_POINT ( 'NONE',  ( -30.18693267962284565, 0.009138568670973495206, -8.767643421507747448 ) ) ;
#26234 = LINE ( 'NONE', #27042, #28053 ) ;
#26236 = ADVANCED_FACE ( 'NONE', ( #31745 ), #13045, .F. ) ;
#26235 = VERTEX_POINT ( 'NONE', #21794 ) ;
#26237 = CARTESIAN_POINT ( 'NONE',  ( 33.67507661585143808, -4.155749373709020311, -6.800351445119964033 ) ) ;
#26238 = VECTOR ( 'NONE', #8323, 1000.000000000000000 ) ;
#26239 = CARTESIAN_POINT ( 'NONE',  ( 17.61751615880474020, 10.50706712441501978, -29.99999999999999645 ) ) ;
#26240 = CARTESIAN_POINT ( 'NONE',  ( 33.86049899301212207, -2.258468967557679452, 15.13084544680245536 ) ) ;
#26241 = VERTEX_POINT ( 'NONE', #31150 ) ;
#26242 = CARTESIAN_POINT ( 'NONE',  ( -6.948689594653023605, 37.54332414141784113, 15.72805884748933813 ) ) ;
#26243 = CARTESIAN_POINT ( 'NONE',  ( 10.93513760492762366, -22.50092802241915635, 18.87996532025630003 ) ) ;
#26244 = LINE ( 'NONE', #10409, #24089 ) ;
#26245 = CARTESIAN_POINT ( 'NONE',  ( -6.839309919355111234, 27.13928353713039954, 20.69868183039781329 ) ) ;
#26246 = CARTESIAN_POINT ( 'NONE',  ( 7.133890061153791429, 30.26901619224539175, 10.49999999999999645 ) ) ;
#26247 = CARTESIAN_POINT ( 'NONE',  ( 14.36830325120613594, 20.48707633493483371, 7.000000000000000000 ) ) ;
#26248 = PRODUCT_DEFINITION_SHAPE ( 'NONE', 'NONE',  #40207 ) ;
#26249 = ADVANCED_FACE ( 'NONE', ( #37834 ), #34001, .F. ) ;
#26250 = CIRCLE ( 'NONE', #28837, 17.00000000000000355 ) ;
#26251 = CARTESIAN_POINT ( 'NONE',  ( 4.942291792648391358, 37.16033961302324684, -7.558059442438699982 ) ) ;
#26252 = DIRECTION ( 'NONE',  ( -0.6459741880212604981, -0.2876062384759471291, 0.7071067811865402453 ) ) ;
#26253 = EDGE_CURVE ( 'NONE', #37413, #7636, #471, .T. ) ;
#26254 = CARTESIAN_POINT ( 'NONE',  ( 13.83280510891587767, 26.34487040060352925, 17.92354375535250810 ) ) ;
#26255 = CARTESIAN_POINT ( 'NONE',  ( -22.10434164247800481, 10.70873872237885394, -8.898544400284965405 ) ) ;
#26256 = CARTESIAN_POINT ( 'NONE',  ( 21.54393101763996654, -26.56854998837850701, -8.110961036857599282 ) ) ;
#26257 = CARTESIAN_POINT ( 'NONE',  ( 11.11016527260166420, 31.83082137946473367, 7.000000000000000000 ) ) ;
#26258 = AXIS2_PLACEMENT_3D ( 'NONE', #22648, #9868, #13306 ) ;
#26259 = CARTESIAN_POINT ( 'NONE',  ( -9.697889840765284930, 31.90483559858339646, 7.000000000000000000 ) ) ;
#26260 = ORIENTED_EDGE ( 'NONE', *, *, #36068, .F. ) ;
#26261 = CARTESIAN_POINT ( 'NONE',  ( 10.98519287105149544, 17.56129497315728827, -27.44095920151953649 ) ) ;
#26262 = ORIENTED_EDGE ( 'NONE', *, *, #34957, .T. ) ;
#26263 = TOROIDAL_SURFACE ( 'NONE', #38619, 1.000000000000000000, 0.5000000000000000000 ) ;
#26264 = CARTESIAN_POINT ( 'NONE',  ( -15.66962402360438666, 25.81090189859874684, -5.946396493405305961 ) ) ;
#26265 = EDGE_CURVE ( 'NONE', #9140, #31499, #10968, .T. ) ;
#26266 = CARTESIAN_POINT ( 'NONE',  ( -17.00801676779734350, -20.85310720624813641, 20.25080042701566541 ) ) ;
#26267 = CYLINDRICAL_SURFACE ( 'NONE', #14667, 56.99999999999991473 ) ;
#26268 = CARTESIAN_POINT ( 'NONE',  ( 15.44688523099049959, 26.67261462138580441, -5.000000000000000000 ) ) ;
#26269 = ORIENTED_EDGE ( 'NONE', *, *, #37982, .F. ) ;
#26270 = CARTESIAN_POINT ( 'NONE',  ( 33.65939441685168276, -18.56364632560252304, -5.855820354545722140 ) ) ;
#26271 = VERTEX_POINT ( 'NONE', #26448 ) ;
#26273 = CARTESIAN_POINT ( 'NONE',  ( 3.863783140547853712E-14, -86.77689918168233874, -5.000000000000000000 ) ) ;
#26272 = CARTESIAN_POINT ( 'NONE',  ( -14.59220174411789017, 25.82205283844941590, -10.62570393986304396 ) ) ;
#26274 = CARTESIAN_POINT ( 'NONE',  ( -11.32539160478685858, -19.87450722000827241, -21.55174846688731805 ) ) ;
#26275 = CARTESIAN_POINT ( 'NONE',  ( -9.742785792574970571, -49.01344959084108410, 3.000000000000000000 ) ) ;
#26276 = ORIENTED_EDGE ( 'NONE', *, *, #19639, .T. ) ;
#26277 = CARTESIAN_POINT ( 'NONE',  ( -33.95062610603429221, -14.00321741133104148, -8.861547101450529595 ) ) ;
#26278 = CARTESIAN_POINT ( 'NONE',  ( -9.862602973713741505, -19.28908076663119076, -23.89725503471435530 ) ) ;
#26279 = CARTESIAN_POINT ( 'NONE',  ( 12.68475447279710799, 27.14725768220933944, 7.000000000000000000 ) ) ;
#26280 = CARTESIAN_POINT ( 'NONE',  ( 16.96835065415153210, 20.59718713987552263, -9.315625699485860167 ) ) ;
#26281 = ORIENTED_EDGE ( 'NONE', *, *, #24007, .T. ) ;
#26282 = CARTESIAN_POINT ( 'NONE',  ( 26.93411999856199301, 3.776180714121243565, -8.821889400297479256 ) ) ;
#26283 = CARTESIAN_POINT ( 'NONE',  ( -0.5000000000000004441, 36.00000000000000711, 7.000000000000000000 ) ) ;
#26284 = FACE_OUTER_BOUND ( 'NONE', #17553, .T. ) ;
#26285 = ORIENTED_EDGE ( 'NONE', *, *, #33211, .T. ) ;
#26286 = EDGE_CURVE ( 'NONE', #31324, #7177, #34999, .T. ) ;
#26287 = CARTESIAN_POINT ( 'NONE',  ( -27.88474080230812646, -0.0008730228811752835556, -13.49305137967154344 ) ) ;
#26288 = EDGE_CURVE ( 'NONE', #36981, #21371, #32760, .T. ) ;
#26289 = TOROIDAL_SURFACE ( 'NONE', #11363, 1.000000000000000000, 0.5000000000000000000 ) ;
#26290 = CARTESIAN_POINT ( 'NONE',  ( 28.89633671753446009, -0.5709352303838933773, -12.48089840086014668 ) ) ;
#26291 = CARTESIAN_POINT ( 'NONE',  ( 16.41753675003191759, -23.14183271658236762, 19.27171037444156454 ) ) ;
#26292 = VERTEX_POINT ( 'NONE', #14055 ) ;
#26293 = CARTESIAN_POINT ( 'NONE',  ( -28.33534295838423844, 2.626085861103411023, -6.423780397466612335 ) ) ;
#26294 = AXIS2_PLACEMENT_3D ( 'NONE', #1335, #935, #13518 ) ;
#26295 = CARTESIAN_POINT ( 'NONE',  ( 15.29245034862073283, 32.56469986092002955, -4.999999999999995559 ) ) ;
#26296 = CARTESIAN_POINT ( 'NONE',  ( 14.72980548178180804, 19.66324911046165269, 7.102474990965864876 ) ) ;
#26297 = VECTOR ( 'NONE', #4769, 1000.000000000000227 ) ;
#26298 = VECTOR ( 'NONE', #3641, 1000.000000000000000 ) ;
#26299 = CARTESIAN_POINT ( 'NONE',  ( 12.30736835487432579, 14.81698729810772619, 7.000000000000000000 ) ) ;
#26300 = B_SPLINE_CURVE_WITH_KNOTS ( 'NONE', 3,
 ( #3270, #9373, #15663, #28050, #34751, #10169, #37791, #34356 ),
 .UNSPECIFIED., .F., .F.,
 ( 4, 2, 2, 4 ),
 ( 0.000000000000000000, 0.0002364868538934295958, 0.0004729737077868591917, 0.0009459474155737161065 ),
 .UNSPECIFIED. ) ;
#26301 = ADVANCED_FACE ( 'NONE', ( #16714 ), #10208, .F. ) ;
#26302 = CARTESIAN_POINT ( 'NONE',  ( -20.23296131041716706, 28.12381335138030636, 0.000000000000000000 ) ) ;
#26303 = FACE_OUTER_BOUND ( 'NONE', #26463, .T. ) ;
#26304 = ADVANCED_FACE ( 'NONE', ( #16510 ), #25636, .T. ) ;
#26305 = DIRECTION ( 'NONE',  ( -1.000000000000000000, 0.000000000000000000, 0.000000000000000000 ) ) ;
#26306 = VERTEX_POINT ( 'NONE', #7150 ) ;
#26307 = DIRECTION ( 'NONE',  ( 0.000000000000000000, 0.000000000000000000, 1.000000000000000000 ) ) ;
#26308 = PLANE ( 'NONE',  #32420 ) ;
#26309 = CARTESIAN_POINT ( 'NONE',  ( 16.06823390034044152, -13.10808670322615832, -27.74124904695872473 ) ) ;
#26310 = DIRECTION ( 'NONE',  ( 1.000000000000000000, 0.000000000000000000, 0.000000000000000000 ) ) ;
#26311 = CARTESIAN_POINT ( 'NONE',  ( 14.48927117870123027, -30.61587158504688233, 11.00000000000000000 ) ) ;
#26312 = CARTESIAN_POINT ( 'NONE',  ( 15.17508192504865683, 27.32470433355475237, -6.406894672669320556 ) ) ;
#26313 = SURFACE_SIDE_STYLE ('',( #13919 ) ) ;
#26314 = ORIENTED_EDGE ( 'NONE', *, *, #12220, .T. ) ;
#26315 = CARTESIAN_POINT ( 'NONE',  ( -14.49642055680277331, 14.68297716386891594, -27.65792624604139860 ) ) ;
#26316 = CARTESIAN_POINT ( 'NONE',  ( -25.28503033819723456, -11.77807541141262782, 20.99999999999999645 ) ) ;
#26317 = CARTESIAN_POINT ( 'NONE',  ( 14.55400969869553229, -25.44726499792421492, -10.65473343070086010 ) ) ;
#26318 = CARTESIAN_POINT ( 'NONE',  ( 10.44103466624280685, 32.57396620494213124, 9.000000000000001776 ) ) ;
#26319 = CARTESIAN_POINT ( 'NONE',  ( 11.19624587173573893, 17.74773942844264596, -26.22615366399902470 ) ) ;
#26320 = ORIENTED_EDGE ( 'NONE', *, *, #968, .F. ) ;
#26321 = CARTESIAN_POINT ( 'NONE',  ( 15.10138251737948600, 26.13808434145718351, -8.767643565617396106 ) ) ;
#26322 = ORIENTED_EDGE ( 'NONE', *, *, #5012, .T. ) ;
#26324 = CARTESIAN_POINT ( 'NONE',  ( 14.41595319144214926, 26.31931657363112720, 10.49999999999999822 ) ) ;
#26323 = CARTESIAN_POINT ( 'NONE',  ( -13.16545571440353335, 22.31697612090500016, -16.43388903272470714 ) ) ;
#26325 = CARTESIAN_POINT ( 'NONE',  ( -13.01110499904087980, -23.09146633989079334, -15.45099639591618690 ) ) ;
#26326 = CARTESIAN_POINT ( 'NONE',  ( -37.58754968649146377, -10.91577297561622117, 11.55979286843978215 ) ) ;
#26327 = CIRCLE ( 'NONE', #39317, 0.5000000000000004441 ) ;
#26328 = VECTOR ( 'NONE', #19924, 1000.000000000000000 ) ;
#26329 = CARTESIAN_POINT ( 'NONE',  ( -22.52291761385160740, -14.54607051226803449, -18.61927420860634541 ) ) ;
#26330 = CARTESIAN_POINT ( 'NONE',  ( -6.891701031399811050, -24.81840269475382499, -8.859753654562227965 ) ) ;
#26331 = CARTESIAN_POINT ( 'NONE',  ( 11.63255956027453841, 17.11425915239349393, -27.48977356258791360 ) ) ;
#26332 = EDGE_LOOP ( 'NONE', ( #4489, #22679 ) ) ;
#26333 = CARTESIAN_POINT ( 'NONE',  ( 18.88780196539459055, 8.001059241770983377, -29.99999999999999645 ) ) ;
#26334 = CARTESIAN_POINT ( 'NONE',  ( -15.21690460405485545, 17.55572914666943873, 12.00000000000000000 ) ) ;
#26335 = CARTESIAN_POINT ( 'NONE',  ( -15.47933092437222768, -26.74032362632396342, -5.000000000000000888 ) ) ;
#26336 = DIRECTION ( 'NONE',  ( -0.8090169943749426773, 0.5877852522924796874, 0.000000000000000000 ) ) ;
#26337 = EDGE_LOOP ( 'NONE', ( #32253, #13352 ) ) ;
#26338 = CARTESIAN_POINT ( 'NONE',  ( -29.45776514400509072, -1.389050121157273665, -12.41183737987973323 ) ) ;
#26339 = CARTESIAN_POINT ( 'NONE',  ( -12.61496056324094539, 7.283250877003592194, 20.99999999999999645 ) ) ;
#26340 = ORIENTED_EDGE ( 'NONE', *, *, #24410, .T. ) ;
#26341 = CARTESIAN_POINT ( 'NONE',  ( 25.28503033819712087, -11.77807541141322822, 20.99999999999999645 ) ) ;
#26342 = DIRECTION ( 'NONE',  ( -1.000000000000000000, 0.000000000000000000, 0.000000000000000000 ) ) ;
#26343 = EDGE_CURVE ( 'NONE', #5601, #1586, #26042, .T. ) ;
#26344 =( LENGTH_UNIT ( ) NAMED_UNIT ( * ) SI_UNIT ( .MILLI., .METRE. ) );
#26345 = CARTESIAN_POINT ( 'NONE',  ( 23.21470675034833775, -11.03075323633567528, -19.64526940384888576 ) ) ;
#26346 = CARTESIAN_POINT ( 'NONE',  ( 36.47502800187007210, -5.175502249961421164, 12.14047268033090887 ) ) ;
#26347 = ORIENTED_EDGE ( 'NONE', *, *, #9131, .T. ) ;
#26348 = CYLINDRICAL_SURFACE ( 'NONE', #21686, 0.4999999999999984457 ) ;
#26349 = DIRECTION ( 'NONE',  ( 1.000000000000000000, 0.000000000000000000, 0.000000000000000000 ) ) ;
#26350 = CIRCLE ( 'NONE', #12746, 1.000000000000000000 ) ;
#26351 = DIRECTION ( 'NONE',  ( 0.000000000000000000, 0.000000000000000000, 1.000000000000000000 ) ) ;
#26352 = ORIENTED_EDGE ( 'NONE', *, *, #1425, .F. ) ;
#26353 = CARTESIAN_POINT ( 'NONE',  ( 1.195900963322536814, 29.06378828199482101, -16.62768215971903984 ) ) ;
#26354 = CARTESIAN_POINT ( 'NONE',  ( -1.590043107810763079, 12.61456814725308107, 10.00000000000000000 ) ) ;
#26355 = VECTOR ( 'NONE', #27764, 1000.000000000000000 ) ;
#26356 = CARTESIAN_POINT ( 'NONE',  ( 3.485571585149869200, -11.24999999999998224, 0.000000000000000000 ) ) ;
#26357 = CARTESIAN_POINT ( 'NONE',  ( 34.47241746879583957, 3.460351812918713854, 0.000000000000000000 ) ) ;
#26358 = DIRECTION ( 'NONE',  ( -1.000000000000000000, 0.000000000000000000, 0.000000000000000000 ) ) ;
#26359 = LINE ( 'NONE', #4422, #38526 ) ;
#26360 = CARTESIAN_POINT ( 'NONE',  ( 11.80513401506518001, 23.30479376290859506, -17.22064554265607228 ) ) ;
#26361 = LINE ( 'NONE', #8072, #18559 ) ;
#26362 = VERTEX_POINT ( 'NONE', #35602 ) ;
#26364 = CARTESIAN_POINT ( 'NONE',  ( 6.064564986133971658, 13.54338174056915456, 13.00000000000000178 ) ) ;
#26363 = CARTESIAN_POINT ( 'NONE',  ( -17.52657988488712704, 12.36839558647593051, -22.23037286673406143 ) ) ;
#26365 = CARTESIAN_POINT ( 'NONE',  ( -9.183247089818959097, 16.78440424842446532, 13.00000000000000178 ) ) ;
#26366 = CARTESIAN_POINT ( 'NONE',  ( 9.523339034571952411, -18.15368110581538019, -30.00000000000000000 ) ) ;
#26367 = DIRECTION ( 'NONE',  ( 0.000000000000000000, 0.000000000000000000, 1.000000000000000000 ) ) ;
#26368 = CARTESIAN_POINT ( 'NONE',  ( 14.99969651570772378, 26.02920516864225675, -9.235286274286707453 ) ) ;
#26369 = CARTESIAN_POINT ( 'NONE',  ( -37.49625565938783467, -14.69322820095469240, -5.000000000000006217 ) ) ;
#26370 = CARTESIAN_POINT ( 'NONE',  ( -3.476907992048017260, 18.63850621467409496, 12.00000000000000000 ) ) ;
#26371 = CARTESIAN_POINT ( 'NONE',  ( -27.87119330683370677, -24.65308250635607479, -6.720147514500800057 ) ) ;
#26372 = CARTESIAN_POINT ( 'NONE',  ( 3.491862997321047324, -22.96065156239022897, -15.91807752016459432 ) ) ;
#26373 = CARTESIAN_POINT ( 'NONE',  ( 15.36189083411322187, 25.97148884136161939, -7.830196362163139412 ) ) ;
#26374 = CARTESIAN_POINT ( 'NONE',  ( 20.43196929446886401, 13.86938077394290580, -7.915868592357410805 ) ) ;
#26375 = CARTESIAN_POINT ( 'NONE',  ( 11.78893975237933134, 23.27376113029817617, 12.00000000000000000 ) ) ;
#26376 = ORIENTED_EDGE ( 'NONE', *, *, #30259, .F. ) ;
#26377 = CARTESIAN_POINT ( 'NONE',  ( -6.250014167710259194, 36.16780209143936986, -8.434276216203160814 ) ) ;
#26378 = VERTEX_POINT ( 'NONE', #35398 ) ;
#26379 = FACE_OUTER_BOUND ( 'NONE', #24541, .T. ) ;
#26380 = ORIENTED_EDGE ( 'NONE', *, *, #20817, .T. ) ;
#26381 = CYLINDRICAL_SURFACE ( 'NONE', #27787, 0.4999999999999995559 ) ;
#26382 = ADVANCED_FACE ( 'NONE', ( #17123 ), #10614, .T. ) ;
#26383 = CARTESIAN_POINT ( 'NONE',  ( -8.412270287199726582, 10.07085245822961994, 10.49999999999999822 ) ) ;
#26384 = ORIENTED_EDGE ( 'NONE', *, *, #2043, .T. ) ;
#26385 = CARTESIAN_POINT ( 'NONE',  ( -25.80299850805823425, 0.4204530589918408223, -16.45275957436017933 ) ) ;
#26386 = ORIENTED_EDGE ( 'NONE', *, *, #32408, .T. ) ;
#26387 = CARTESIAN_POINT ( 'NONE',  ( 34.97939493771907848, -10.55727357374866493, -7.588994557062878954 ) ) ;
#26388 = ADVANCED_FACE ( 'NONE', ( #19547 ), #19753, .F. ) ;
#26389 = ORIENTED_EDGE ( 'NONE', *, *, #40163, .F. ) ;
#26390 =( NAMED_UNIT ( * ) PLANE_ANGLE_UNIT ( ) SI_UNIT ( $, .RADIAN. ) );
#26391 = FACE_OUTER_BOUND ( 'NONE', #10773, .T. ) ;
#26392 = ORIENTED_EDGE ( 'NONE', *, *, #36830, .T. ) ;
#26393 = EDGE_CURVE ( 'NONE', #19420, #2652, #38844, .T. ) ;
#26394 = CARTESIAN_POINT ( 'NONE',  ( 9.831584923911636409, 26.22020669908449975, 10.50000000000000000 ) ) ;
#26395 = CARTESIAN_POINT ( 'NONE',  ( -3.789799368034432181, 7.986433676831034667, 7.485699520496976511 ) ) ;
#26396 = CARTESIAN_POINT ( 'NONE',  ( -1.189115275033253716E-13, 36.23016441347868977, 18.42518152272108622 ) ) ;
#26397 = CYLINDRICAL_SURFACE ( 'NONE', #12298, 0.5000000000000000000 ) ;
#26398 = ORIENTED_EDGE ( 'NONE', *, *, #14701, .T. ) ;
#26399 = CARTESIAN_POINT ( 'NONE',  ( -14.31603901957233660, 19.98981538725089990, 10.49999999999999467 ) ) ;
#26400 = DIRECTION ( 'NONE',  ( 0.000000000000000000, 0.000000000000000000, 1.000000000000000000 ) ) ;
#26401 = CARTESIAN_POINT ( 'NONE',  ( -0.9819677022348329842, 30.37627742347970283, 13.00000000000000178 ) ) ;
#26402 = CARTESIAN_POINT ( 'NONE',  ( 18.78138322832032969, 16.61749776086161035, -9.368813598564180722 ) ) ;
#26403 = AXIS2_PLACEMENT_3D ( 'NONE', #11105, #16596, #38929 ) ;
#26404 = CARTESIAN_POINT ( 'NONE',  ( 10.84964834875164463, 34.03396980005788919, -6.755589542877508791 ) ) ;
#26405 = CIRCLE ( 'NONE', #23194, 0.4999999999999998890 ) ;
#26406 = VERTEX_POINT ( 'NONE', #22995 ) ;
#26407 = DIRECTION ( 'NONE',  ( 0.000000000000000000, 0.000000000000000000, 1.000000000000000000 ) ) ;
#26408 = CARTESIAN_POINT ( 'NONE',  ( 0.000000000000000000, 22.50000000000000355, 7.000000000000000000 ) ) ;
#26409 = ADVANCED_FACE ( 'NONE', ( #32148 ), #4106, .T. ) ;
#26410 = EDGE_CURVE ( 'NONE', #37009, #16315, #20718, .T. ) ;
#26411 = CARTESIAN_POINT ( 'NONE',  ( 12.67954175781115822, -22.01374323132807476, -17.39205990358088272 ) ) ;
#26412 = CARTESIAN_POINT ( 'NONE',  ( 19.48557158514975285, -11.24999999999995737, 6.000000000000000000 ) ) ;
#26413 = AXIS2_PLACEMENT_3D ( 'NONE', #29834, #14602, #14399 ) ;
#26414 = DIRECTION ( 'NONE',  ( 0.4156269377774587936, 0.5720614028176801424, -0.7071067811865477948 ) ) ;
#26415 = ORIENTED_EDGE ( 'NONE', *, *, #25025, .F. ) ;
#26416 = CIRCLE ( 'NONE', #23167, 1.000000000000014655 ) ;
#26417 = CARTESIAN_POINT ( 'NONE',  ( -15.40573053741202791, 26.82015453055286969, -5.000000000000001776 ) ) ;
#26418 = CARTESIAN_POINT ( 'NONE',  ( -29.03912765165685528, -24.78940378269006573, 15.72805884748945715 ) ) ;
#26419 = CARTESIAN_POINT ( 'NONE',  ( 12.39246001483761539, -23.54175171672831723, -14.52989995892280106 ) ) ;
#26420 = CARTESIAN_POINT ( 'NONE',  ( 1.838889047819958655, 31.15129278236397781, 9.000000000000001776 ) ) ;
#26421 = EDGE_LOOP ( 'NONE', ( #2066, #33698, #26015, #28754 ) ) ;
#26422 = EDGE_LOOP ( 'NONE', ( #22135, #20049 ) ) ;
#26423 = CARTESIAN_POINT ( 'NONE',  ( -12.61462386970939775, 32.22368281794742018, -6.341505710337779433 ) ) ;
#26424 = LINE ( 'NONE', #27032, #8125 ) ;
#26425 = LINE ( 'NONE', #10591, #22391 ) ;
#26426 = CARTESIAN_POINT ( 'NONE',  ( -23.48166808057901989, -5.066536945620522481, -20.99526510558111170 ) ) ;
#26427 = CARTESIAN_POINT ( 'NONE',  ( 3.476901250629512941, 26.36149378532653031, 6.000000000000000000 ) ) ;
#26428 = ORIENTED_EDGE ( 'NONE', *, *, #39800, .F. ) ;
#26429 = CARTESIAN_POINT ( 'NONE',  ( 20.68909164424603730, 0.9095261957111510087, -27.45237514931904954 ) ) ;
#26430 = CARTESIAN_POINT ( 'NONE',  ( -10.14084140100247389, 32.97648733965221624, 10.49999999999999822 ) ) ;
#26431 = FACE_OUTER_BOUND ( 'NONE', #9603, .T. ) ;
#26432 = FACE_OUTER_BOUND ( 'NONE', #11489, .T. ) ;
#26433 = ORIENTED_EDGE ( 'NONE', *, *, #593, .F. ) ;
#26434 = CARTESIAN_POINT ( 'NONE',  ( -27.15853788013058079, 0.2099631823020539356, -14.47428761516277618 ) ) ;
#26435 = EDGE_CURVE ( 'NONE', #21143, #35248, #3815, .T. ) ;
#26436 = LINE ( 'NONE', #38834, #7957 ) ;
#26437 = ORIENTED_EDGE ( 'NONE', *, *, #27423, .F. ) ;
#26438 = CARTESIAN_POINT ( 'NONE',  ( 20.73891562577072634, -0.9609881625880122291, -27.33083722918737735 ) ) ;
#26439 = CARTESIAN_POINT ( 'NONE',  ( 36.73707435953490119, -10.93158220173851802, 14.53008259254007051 ) ) ;
#26440 = ORIENTED_EDGE ( 'NONE', *, *, #16400, .T. ) ;
#26441 = CARTESIAN_POINT ( 'NONE',  ( 13.24632657851087991, 31.48533120267433461, 16.30093088680191116 ) ) ;
#26442 = CIRCLE ( 'NONE', #36831, 1.000000000000000888 ) ;
#26443 = CARTESIAN_POINT ( 'NONE',  ( 11.18737074831306266, -21.01894785638886987, 19.66345542862420714 ) ) ;
#26444 = B_SPLINE_CURVE_WITH_KNOTS ( 'NONE', 3,
 ( #31197, #27552, #9266, #18416 ),
 .UNSPECIFIED., .F., .F.,
 ( 4, 4 ),
 ( 0.000000000000000000, 1.000000000000000000 ),
 .UNSPECIFIED. ) ;
#26445 = FACE_OUTER_BOUND ( 'NONE', #36643, .T. ) ;
#26446 = CARTESIAN_POINT ( 'NONE',  ( -4.499574175057204251, 28.42082499241989169, 20.82122704794079837 ) ) ;
#26447 = CIRCLE ( 'NONE', #29699, 1.000000000000000000 ) ;
#26448 = CARTESIAN_POINT ( 'NONE',  ( -12.64211604268330724, 20.79918788657763429, 13.00000000000000178 ) ) ;
#26449 = ORIENTED_EDGE ( 'NONE', *, *, #27220, .F. ) ;
#26450 = LINE ( 'NONE', #32966, #30587 ) ;
#26451 = CARTESIAN_POINT ( 'NONE',  ( 4.986586119666859496, 37.59550631332245985, -6.283304853315398120 ) ) ;
#26452 = CARTESIAN_POINT ( 'NONE',  ( -1.278175571584109660, 14.08178954835378427, 9.000000000000001776 ) ) ;
#26453 = CARTESIAN_POINT ( 'NONE',  ( 18.85374159600720745, 16.91074157332428385, 16.30093088680196445 ) ) ;
#26454 = ADVANCED_FACE ( 'NONE', ( #13859 ), #34306, .T. ) ;
#26455 = CARTESIAN_POINT ( 'NONE',  ( 12.14263327931022474, -17.31510639158323173, -25.99352023739256623 ) ) ;
#26456 = CARTESIAN_POINT ( 'NONE',  ( -13.80290580123967992, 34.21636679304901918, 11.00000000000033218 ) ) ;
#26457 = VECTOR ( 'NONE', #26414, 1000.000000000000000 ) ;
#26458 = CARTESIAN_POINT ( 'NONE',  ( -11.11016527260153808, 31.83082137946488643, 7.500000000000004441 ) ) ;
#26459 = CARTESIAN_POINT ( 'NONE',  ( 4.724371395536106633, 32.23037938972932892, 13.00000000000000178 ) ) ;
#26460 = ORIENTED_EDGE ( 'NONE', *, *, #35662, .F. ) ;
#26461 = CARTESIAN_POINT ( 'NONE',  ( 15.13632466973338353, 26.41015704048310297, -8.292868291921246637 ) ) ;
#26462 = CIRCLE ( 'NONE', #4398, 0.5000000000000004441 ) ;
#26463 = EDGE_LOOP ( 'NONE', ( #15079, #21625, #713, #2017 ) ) ;
#26465 = AXIS2_PLACEMENT_3D ( 'NONE', #11104, #30595, #20652 ) ;
#26464 = CARTESIAN_POINT ( 'NONE',  ( -13.03586472630768078, 20.49849890579186962, -18.51679387589177139 ) ) ;
#26466 = CARTESIAN_POINT ( 'NONE',  ( -30.40812954450618832, -7.345122744317324148, 19.66345542862560691 ) ) ;
#26467 = DIRECTION ( 'NONE',  ( 0.8660254037844431485, 0.4999999999999921174, -0.000000000000000000 ) ) ;
#26468 = CARTESIAN_POINT ( 'NONE',  ( 14.77255199613913739, 25.29418844797250898, -10.65547838526898694 ) ) ;
#26469 = ORIENTED_EDGE ( 'NONE', *, *, #13596, .F. ) ;
#26470 = CARTESIAN_POINT ( 'NONE',  ( 17.54066805493992121, -11.09882095461065710, -27.70640768852350888 ) ) ;
#26471 = B_SPLINE_CURVE_WITH_KNOTS ( 'NONE', 3,
 ( #14179, #33290, #17652, #5632, #2399, #23929 ),
 .UNSPECIFIED., .F., .F.,
 ( 4, 2, 4 ),
 ( 0.000000000000000000, 0.5000000000000001110, 1.000000000000000000 ),
 .UNSPECIFIED. ) ;
#26472 = EDGE_LOOP ( 'NONE', ( #36739, #23902, #18596, #1155 ) ) ;
#26473 = CONICAL_SURFACE ( 'NONE', #5707, 0.5000000000000002220, 0.7853981633974506105 ) ;
#26475 = DIRECTION ( 'NONE',  ( 0.000000000000000000, 0.000000000000000000, -1.000000000000000000 ) ) ;
#26474 = CARTESIAN_POINT ( 'NONE',  ( -13.77510122325607789, 24.52954501137963916, -13.45804258254887209 ) ) ;
#26476 = CARTESIAN_POINT ( 'NONE',  ( -10.52265961525695559, -18.21930999212262137, -26.15301577430472335 ) ) ;
#26477 = CARTESIAN_POINT ( 'NONE',  ( 13.44717671261699010, 15.85337785810300026, 7.339470489435489853 ) ) ;
#26478 = CIRCLE ( 'NONE', #21294, 58.00000000000006395 ) ;
#26479 = B_SPLINE_CURVE_WITH_KNOTS ( 'NONE', 3,
 ( #27300, #39878, #8817, #17776, #15303, #39688, #18556, #24646 ),
 .UNSPECIFIED., .F., .F.,
 ( 4, 2, 2, 4 ),
 ( 0.000000000000000000, 0.0002364868538934288640, 0.0004729737077868577280, 0.0009459474155737242380 ),
 .UNSPECIFIED. ) ;
#26480 = ORIENTED_EDGE ( 'NONE', *, *, #9427, .F. ) ;
#26481 = CARTESIAN_POINT ( 'NONE',  ( -34.66916150951502829, -13.09694564545405626, -7.995340687606282692 ) ) ;
#26482 = CARTESIAN_POINT ( 'NONE',  ( -10.85943135922135561, -20.52714661791293338, -20.57883059674998805 ) ) ;
#26483 = DIRECTION ( 'NONE',  ( -0.6459741880212607201, -0.2876062384759439094, -0.7071067811865414665 ) ) ;
#26484 = CARTESIAN_POINT ( 'NONE',  ( 16.54809703417162225, 21.62887500659449103, -9.299666550987730318 ) ) ;
#26485 = ORIENTED_EDGE ( 'NONE', *, *, #10012, .T. ) ;
#26486 = CARTESIAN_POINT ( 'NONE',  ( 20.51437803745783484, 4.510445312378868365, -25.33195205685563423 ) ) ;
#26487 = CARTESIAN_POINT ( 'NONE',  ( -8.145563986382438060, 10.43794218875019908, 10.99999999999999289 ) ) ;
#26488 = CARTESIAN_POINT ( 'NONE',  ( -24.51396478725048667, -11.15767879383074757, 23.00000000000000000 ) ) ;
#26489 = VERTEX_POINT ( 'NONE', #29500 ) ;
#26490 = CARTESIAN_POINT ( 'NONE',  ( -20.61986670983709402, 0.6792029499141194471, -28.06894698849345460 ) ) ;
#26491 = ADVANCED_FACE ( 'NONE', ( #29301 ), #1470, .T. ) ;
#26492 = CARTESIAN_POINT ( 'NONE',  ( 23.48977253511795737, 0.06509944194096961567, -20.47537068515592296 ) ) ;
#26493 = ADVANCED_FACE ( 'NONE', ( #1673 ), #35800, .F. ) ;
#26494 = CARTESIAN_POINT ( 'NONE',  ( 30.54456991890647899, -14.74984208377836481, 19.66345542862529072 ) ) ;
#26495 = ORIENTED_EDGE ( 'NONE', *, *, #4858, .F. ) ;
#26496 = CARTESIAN_POINT ( 'NONE',  ( -23.30533847871739184, 2.001508224256452362, -19.66258829786930562 ) ) ;
#26497 = CARTESIAN_POINT ( 'NONE',  ( 16.84920187454417828, 29.09530251867925443, -5.000000000000000000 ) ) ;
#26498 = CYLINDRICAL_SURFACE ( 'NONE', #15453, 1.000000000000000000 ) ;
#26499 = AXIS2_PLACEMENT_3D ( 'NONE', #39335, #5007, #29192 ) ;
#26500 = CIRCLE ( 'NONE', #27776, 1.000000000000000888 ) ;
#26501 = EDGE_CURVE ( 'NONE', #11836, #29721, #31648, .T. ) ;
#26502 = DIRECTION ( 'NONE',  ( 0.000000000000000000, 0.000000000000000000, 1.000000000000000000 ) ) ;
#26503 = AXIS2_PLACEMENT_3D ( 'NONE', #4355, #1116, #4968 ) ;
#26504 = VECTOR ( 'NONE', #14357, 1000.000000000000000 ) ;
#26505 = CARTESIAN_POINT ( 'NONE',  ( -23.05386822411323422, -7.747535282638357224, 23.00000000000000000 ) ) ;
#26506 = CARTESIAN_POINT ( 'NONE',  ( -13.94482798346716201, 26.50521816028930999, 9.500000000000000000 ) ) ;
#26507 = LINE ( 'NONE', #16968, #30219 ) ;
#26508 = ORIENTED_EDGE ( 'NONE', *, *, #20767, .F. ) ;
#26509 = CARTESIAN_POINT ( 'NONE',  ( -26.14285255608131209, 5.307274672128771797, -6.434788150531786322 ) ) ;
#26510 = CARTESIAN_POINT ( 'NONE',  ( -8.927394655428429360, 11.06314620770957013, 7.000000000000000000 ) ) ;
#26511 = CARTESIAN_POINT ( 'NONE',  ( -14.57486473880221745, 26.18419839932921533, 7.000000000000000000 ) ) ;
#26512 = CARTESIAN_POINT ( 'NONE',  ( 28.04695191141788158, -24.37772861669491320, -7.143925439455689030 ) ) ;
#26513 = EDGE_CURVE ( 'NONE', #9757, #17958, #34339, .T. ) ;
#26514 = EDGE_CURVE ( 'NONE', #5201, #22834, #36921, .T. ) ;
#26515 = CARTESIAN_POINT ( 'NONE',  ( 3.295881626406574672, 9.398963235502481695, 10.50000000000000000 ) ) ;
#26516 = DIRECTION ( 'NONE',  ( 1.000000000000000000, 0.000000000000000000, 0.000000000000000000 ) ) ;
#26517 = EDGE_CURVE ( 'NONE', #15234, #1646, #8381, .T. ) ;
#26518 = CARTESIAN_POINT ( 'NONE',  ( 11.89959718257016164, 20.19666440959803921, -20.49464208040282642 ) ) ;
#26519 = DIRECTION ( 'NONE',  ( 1.000000000000000000, 0.000000000000000000, 0.000000000000000000 ) ) ;
#26520 = ORIENTED_EDGE ( 'NONE', *, *, #25773, .F. ) ;
#26521 = CARTESIAN_POINT ( 'NONE',  ( -13.39027686378713788, 15.57931273310112985, -28.79240298120324226 ) ) ;
#26522 = CARTESIAN_POINT ( 'NONE',  ( -21.14791330573199346, -16.83114732581389461, 21.00000000000004619 ) ) ;
#26523 = CARTESIAN_POINT ( 'NONE',  ( 9.583578724557431983, -18.35907664999004396, -27.45048110621220872 ) ) ;
#26524 = DIRECTION ( 'NONE',  ( -1.000000000000000000, 0.000000000000000000, 0.000000000000000000 ) ) ;
#26525 = CARTESIAN_POINT ( 'NONE',  ( 11.31934672680579723, 18.03076597873480935, -25.01582983836050644 ) ) ;
#26526 = ORIENTED_EDGE ( 'NONE', *, *, #20676, .F. ) ;
#26527 = CARTESIAN_POINT ( 'NONE',  ( -14.51883047965001694, 21.47676356526632446, 11.00000000000000355 ) ) ;
#26528 = ORIENTED_EDGE ( 'NONE', *, *, #4352, .F. ) ;
#26530 = LINE ( 'NONE', #23478, #32861 ) ;
#26529 = CARTESIAN_POINT ( 'NONE',  ( -10.95814459664155294, 17.32538844660855659, -29.99999999999999645 ) ) ;
#26531 = CARTESIAN_POINT ( 'NONE',  ( -11.96823149460782254, -21.48079789499611536, -18.44457378902819400 ) ) ;
#26532 = CARTESIAN_POINT ( 'NONE',  ( -34.83527399001570046, -1.648960735038180525, 11.55979286843900411 ) ) ;
#26533 = VECTOR ( 'NONE', #858, 1000.000000000000000 ) ;
#26534 = CARTESIAN_POINT ( 'NONE',  ( -20.72646010994916210, -13.37970267315822781, -20.69910896450166149 ) ) ;
#26535 = CARTESIAN_POINT ( 'NONE',  ( -6.348761669075202008, -23.58403035214085008, -13.80701084941673606 ) ) ;
#26536 = CARTESIAN_POINT ( 'NONE',  ( 11.55093992908412126, 16.93669310835906572, -29.36020701913010456 ) ) ;
#26537 = ORIENTED_EDGE ( 'NONE', *, *, #39419, .F. ) ;
#26538 = CARTESIAN_POINT ( 'NONE',  ( 19.51861134948594056, 7.376813021019582806, -25.46285920900043109 ) ) ;
#26539 = CARTESIAN_POINT ( 'NONE',  ( 17.34253826607186255, 27.32041144404028543, -5.000000000000000000 ) ) ;
#26540 = DIRECTION ( 'NONE',  ( 1.000000000000000000, 0.000000000000000000, 0.000000000000000000 ) ) ;
#26541 = LINE ( 'NONE', #38930, #30350 ) ;
#26542 = VECTOR ( 'NONE', #15907, 1000.000000000000114 ) ;
#26543 = EDGE_LOOP ( 'NONE', ( #33157, #7281, #34501, #18112 ) ) ;
#26544 = CARTESIAN_POINT ( 'NONE',  ( -32.63376561907040951, -2.508419813268226939, -7.282485175223003537 ) ) ;
#26545 =( BOUNDED_CURVE ( )  B_SPLINE_CURVE ( 2, ( #35309, #2000, #29614 ),
 .UNSPECIFIED., .F., .F. ) 
 B_SPLINE_CURVE_WITH_KNOTS ( ( 3, 3 ),
 ( 0.000000000000000000, 1.000000000000000000 ),
 .UNSPECIFIED. ) 
 CURVE ( )  GEOMETRIC_REPRESENTATION_ITEM ( )  RATIONAL_B_SPLINE_CURVE ( ( 1.000000000000000000, 0.7071067811865474617, 1.000000000000000000 ) ) 
 REPRESENTATION_ITEM ( '' )  );
#26546 = EDGE_CURVE ( 'NONE', #9387, #33664, #16802, .T. ) ;
#26547 = CARTESIAN_POINT ( 'NONE',  ( -14.04126239388531161, 8.106726622871482490, 20.82122704794079837 ) ) ;
#26548 = EDGE_CURVE ( 'NONE', #10384, #21291, #39834, .T. ) ;
#26549 = CARTESIAN_POINT ( 'NONE',  ( 23.61737546510263996, -7.194424252577891643, 20.99999999999999645 ) ) ;
#26550 = CARTESIAN_POINT ( 'NONE',  ( 18.23649648353767461, -16.09146789626181118, 20.99999999999999645 ) ) ;
#26551 = PLANE ( 'NONE',  #20321 ) ;
#26552 = CARTESIAN_POINT ( 'NONE',  ( 34.23814126792781565, -17.55187814006816538, -5.435598090313549235 ) ) ;
#26553 = CARTESIAN_POINT ( 'NONE',  ( -19.48557158514985588, -11.25000000000002309, 6.000000000000000000 ) ) ;
#26554 = ORIENTED_EDGE ( 'NONE', *, *, #29593, .F. ) ;
#26555 = CARTESIAN_POINT ( 'NONE',  ( -12.80736835487442349, 15.68301270189233954, 7.000000000000000000 ) ) ;
#26556 = CIRCLE ( 'NONE', #2462, 1.000000000000000000 ) ;
#26557 = AXIS2_PLACEMENT_3D ( 'NONE', #9280, #6420, #24913 ) ;
#26558 = FACE_OUTER_BOUND ( 'NONE', #20481, .T. ) ;
#26559 = ORIENTED_EDGE ( 'NONE', *, *, #8513, .F. ) ;
#26560 = CARTESIAN_POINT ( 'NONE',  ( 1.576739634193316197, 38.46478598617967748, -5.000000000000004441 ) ) ;
#26561 = DIRECTION ( 'NONE',  ( 0.6691306063588671194, 0.7431448254773862505, 0.000000000000000000 ) ) ;
#26562 = PLANE ( 'NONE',  #12362 ) ;
#26563 = DIRECTION ( 'NONE',  ( -0.000000000000000000, -0.000000000000000000, -1.000000000000000000 ) ) ;
#26564 = CARTESIAN_POINT ( 'NONE',  ( -6.686869517299739663, 14.99761530854305391, 10.50000000000000533 ) ) ;
#26565 = CARTESIAN_POINT ( 'NONE',  ( -1.734965421685230824, 7.600674680189156263, 7.000000000000000000 ) ) ;
#26566 = CARTESIAN_POINT ( 'NONE',  ( 12.28075117147713513, 22.65327156252982022, -17.30410852053039861 ) ) ;
#26567 = DIRECTION ( 'NONE',  ( -0.5254827454987587299, -0.4731467892558131605, -0.7071067811865487940 ) ) ;
#26568 = ORIENTED_EDGE ( 'NONE', *, *, #10502, .T. ) ;
#26570 = DIRECTION ( 'NONE',  ( 0.4067366430758009299, 0.9135454576426005335, -0.000000000000000000 ) ) ;
#26569 = CARTESIAN_POINT ( 'NONE',  ( -16.87192496629801397, 11.79917111600507162, -27.72865834311171795 ) ) ;
#26571 = DIRECTION ( 'NONE',  ( 1.000000000000000000, 0.000000000000000000, 0.000000000000000000 ) ) ;
#26572 = CARTESIAN_POINT ( 'NONE',  ( 11.56771891837488120, -20.97406469625146386, -19.49405188942785117 ) ) ;
#26573 = DIRECTION ( 'NONE',  ( 0.6691306063588570163, -0.7431448254773953543, 0.000000000000000000 ) ) ;
#26574 = CARTESIAN_POINT ( 'NONE',  ( 11.87119298004463097, 19.40464818915105383, -21.61300753313285128 ) ) ;
#26575 = CARTESIAN_POINT ( 'NONE',  ( 6.155076441694339096, 21.71698211341367468, -20.11584339644708308 ) ) ;
#26576 = CARTESIAN_POINT ( 'NONE',  ( -23.43644022947910344, -8.137298067154993930, 22.99999999999999289 ) ) ;
#26577 = CARTESIAN_POINT ( 'NONE',  ( -15.37450020624324232, -14.42786494016273124, -26.36729165574789491 ) ) ;
#26578 = CARTESIAN_POINT ( 'NONE',  ( 3.990328747834301915, -24.74414097261287537, -7.420647813714800201 ) ) ;
#26579 = CARTESIAN_POINT ( 'NONE',  ( 15.41962056465840369, 26.08857641750358880, -7.359439485418601379 ) ) ;
#26580 = CARTESIAN_POINT ( 'NONE',  ( 21.03405174098776342, 12.96318115116885394, -6.940238061123360502 ) ) ;
#26581 = CARTESIAN_POINT ( 'NONE',  ( -12.30736835487442704, 14.81698729810789672, 7.499999999999993783 ) ) ;
#26582 = ORIENTED_EDGE ( 'NONE', *, *, #39048, .F. ) ;
#26583 = CARTESIAN_POINT ( 'NONE',  ( -6.386588552221052595, 37.17016244130430636, -4.999999999999996447 ) ) ;
#26584 = VERTEX_POINT ( 'NONE', #18121 ) ;
#26585 = CONICAL_SURFACE ( 'NONE', #31109, 0.5000000000000111022, 0.7853981633974492782 ) ;
#26586 = DIRECTION ( 'NONE',  ( 0.000000000000000000, -0.000000000000000000, -1.000000000000000000 ) ) ;
#26587 = ORIENTED_EDGE ( 'NONE', *, *, #15267, .F. ) ;
#26588 = CARTESIAN_POINT ( 'NONE',  ( -5.034171952701850472, 35.03623199971308111, 10.00000000000000000 ) ) ;
#26589 = DIRECTION ( 'NONE',  ( -0.000000000000000000, -0.000000000000000000, -1.000000000000000000 ) ) ;
#26590 = CIRCLE ( 'NONE', #9074, 0.4999999999999998335 ) ;
#26591 = ORIENTED_EDGE ( 'NONE', *, *, #32902, .T. ) ;
#26592 = CARTESIAN_POINT ( 'NONE',  ( -30.19789697583199839, 0.4197591680151108728, -7.359975557626077247 ) ) ;
#26593 = ORIENTED_EDGE ( 'NONE', *, *, #35561, .F. ) ;
#26594 = CARTESIAN_POINT ( 'NONE',  ( 33.75734116780339633, -10.15240224287356519, -9.788738968072763669 ) ) ;
#26595 = ORIENTED_EDGE ( 'NONE', *, *, #37296, .F. ) ;
#26596 = LINE ( 'NONE', #2028, #7652 ) ;
#26597 = VERTEX_POINT ( 'NONE', #14454 ) ;
#26598 = CARTESIAN_POINT ( 'NONE',  ( 17.34253826607184479, 27.32041144404033162, 2.999999999999999112 ) ) ;
#26599 = DIRECTION ( 'NONE',  ( 0.000000000000000000, 0.000000000000000000, 1.000000000000000000 ) ) ;
#26600 = CARTESIAN_POINT ( 'NONE',  ( -5.496198527381525700, 34.39821714758459592, 18.87996532025786323 ) ) ;
#26601 = CARTESIAN_POINT ( 'NONE',  ( 0.000000000000000000, 22.50000000000000355, 7.000000000000000000 ) ) ;
#26602 = ORIENTED_EDGE ( 'NONE', *, *, #31759, .T. ) ;
#26603 = CARTESIAN_POINT ( 'NONE',  ( -1.494943660522439099, 10.76222879119470832, 6.000000000000000000 ) ) ;
#26604 = DIRECTION ( 'NONE',  ( 0.000000000000000000, 0.000000000000000000, 1.000000000000000000 ) ) ;
#26605 = CARTESIAN_POINT ( 'NONE',  ( 10.39021566973303656, 20.90519018800546647, 10.00000000000000000 ) ) ;
#26606 = CARTESIAN_POINT ( 'NONE',  ( 16.16724516751253660, 14.83928554355248330, -21.07326466058601611 ) ) ;
#26607 = CARTESIAN_POINT ( 'NONE',  ( 10.52168943551277280, 32.83820809845378363, -9.399405207729710554 ) ) ;
#26608 = ORIENTED_EDGE ( 'NONE', *, *, #12218, .F. ) ;
#26609 = FACE_OUTER_BOUND ( 'NONE', #5263, .T. ) ;
#26610 = DIRECTION ( 'NONE',  ( -0.9135454576426070838, -0.4067366430757864970, 0.000000000000000000 ) ) ;
#26611 = EDGE_CURVE ( 'NONE', #30937, #22876, #12261, .T. ) ;
#26612 = CARTESIAN_POINT ( 'NONE',  ( 15.33699111502133583, -26.20517303025969369, -8.756749650358152337 ) ) ;
#26613 = CARTESIAN_POINT ( 'NONE',  ( 14.36830325120613594, 20.48707633493483371, 7.500000000000010658 ) ) ;
#26614 = CIRCLE ( 'NONE', #4573, 1.000000000000000000 ) ;
#26615 = CARTESIAN_POINT ( 'NONE',  ( 13.48130249190479724, 27.93180293473185927, 9.500000000000000000 ) ) ;
#26616 = CARTESIAN_POINT ( 'NONE',  ( -13.76002159541111247, 23.41745082153441615, -14.47402975780730117 ) ) ;
#26617 = CARTESIAN_POINT ( 'NONE',  ( -36.01097648505578519, -14.57711145883881620, 15.13084544680213384 ) ) ;
#26618 = CARTESIAN_POINT ( 'NONE',  ( 9.154532225212971497, -18.83911771395485601, -26.28255396391754672 ) ) ;
#26619 = EDGE_CURVE ( 'NONE', #4691, #16943, #34973, .T. ) ;
#26620 = DIRECTION ( 'NONE',  ( -0.3090169943749434545, 0.9510565162951548634, 0.000000000000000000 ) ) ;
#26621 = EDGE_CURVE ( 'NONE', #7162, #34341, #27056, .T. ) ;
#26622 = ORIENTED_EDGE ( 'NONE', *, *, #23307, .F. ) ;
#26623 = ORIENTED_EDGE ( 'NONE', *, *, #22264, .T. ) ;
#26624 = CARTESIAN_POINT ( 'NONE',  ( -7.700672618952613568, 19.08108758880122480, -28.57812135046165736 ) ) ;
#26625 = DIRECTION ( 'NONE',  ( -0.000000000000000000, -0.000000000000000000, 1.000000000000000000 ) ) ;
#26626 = DIRECTION ( 'NONE',  ( 0.8090169943749430104, -0.5877852522924791323, 0.000000000000000000 ) ) ;
#26627 = VECTOR ( 'NONE', #2917, 999.9999999999998863 ) ;
#26628 = CARTESIAN_POINT ( 'NONE',  ( -22.77417947270713228, -3.486102136050852618, -22.25714798909087833 ) ) ;
#26629 = DIRECTION ( 'NONE',  ( 0.000000000000000000, 0.000000000000000000, 1.000000000000000000 ) ) ;
#26630 = ORIENTED_EDGE ( 'NONE', *, *, #4272, .F. ) ;
#26631 = CARTESIAN_POINT ( 'NONE',  ( 30.55543456312852157, 0.04490906986981075405, -7.358140873893511902 ) ) ;
#26632 = FACE_OUTER_BOUND ( 'NONE', #25505, .T. ) ;
#26633 = PLANE ( 'NONE',  #14200 ) ;
#26634 = CARTESIAN_POINT ( 'NONE',  ( -2.535262076962894184, 8.167662524930003443, 10.99999999999999289 ) ) ;
#26635 = UNCERTAINTY_MEASURE_WITH_UNIT (LENGTH_MEASURE( 1.000000000000000082E-05 ), #35352, 'distance_accuracy_value', 'NONE');
#26636 = B_SPLINE_CURVE_WITH_KNOTS ( 'NONE', 3,
 ( #23654, #8418, #8211, #17777, #20616, #1725, #26296, #20414 ),
 .UNSPECIFIED., .F., .F.,
 ( 4, 2, 2, 4 ),
 ( 0.000000000000000000, 0.0002364868538934280237, 0.0004729737077868560475, 0.0009459474155737213107 ),
 .UNSPECIFIED. ) ;
#26637 = ORIENTED_EDGE ( 'NONE', *, *, #691, .T. ) ;
#26638 = CARTESIAN_POINT ( 'NONE',  ( -30.16151852821994694, 0.03644184463863008039, -8.767989454590962239 ) ) ;
#26639 = CYLINDRICAL_SURFACE ( 'NONE', #11857, 0.5000000000000004441 ) ;
#26640 = VERTEX_POINT ( 'NONE', #30102 ) ;
#26641 = CARTESIAN_POINT ( 'NONE',  ( 27.72733811610554966, -4.089226208729503043, -16.01998001631908508 ) ) ;
#26642 = CARTESIAN_POINT ( 'NONE',  ( 35.28408311606053616, -16.24929212131948475, 15.72805884748936656 ) ) ;
#26643 = ORIENTED_EDGE ( 'NONE', *, *, #33127, .F. ) ;
#26644 = CARTESIAN_POINT ( 'NONE',  ( 15.69115823232677620, 30.83414889893647626, 13.32518128616601061 ) ) ;
#26645 = ADVANCED_FACE ( 'NONE', ( #26649 ), #39038, .T. ) ;
#26646 = CARTESIAN_POINT ( 'NONE',  ( -15.48695972776671326, -26.74878859331622039, 16.30093088680190405 ) ) ;
#26647 = DIRECTION ( 'NONE',  ( -0.8090169943749505599, -0.5877852522924690293, 0.000000000000000000 ) ) ;
#26648 = CARTESIAN_POINT ( 'NONE',  ( -5.140622461635718565, 27.93365566737808692, 20.82122704794108259 ) ) ;
#26649 = FACE_OUTER_BOUND ( 'NONE', #21728, .T. ) ;
#26650 = ORIENTED_EDGE ( 'NONE', *, *, #22999, .F. ) ;
#26651 = CARTESIAN_POINT ( 'NONE',  ( -4.817371740575545402, 23.83900317890010001, 20.99999999999999645 ) ) ;
#26652 = DIRECTION ( 'NONE',  ( -0.000000000000000000, -0.000000000000000000, -1.000000000000000000 ) ) ;
#26653 = CARTESIAN_POINT ( 'NONE',  ( 5.661823860689081833, 34.35857903786058642, -11.10029543532181684 ) ) ;
#26654 = AXIS2_PLACEMENT_3D ( 'NONE', #2278, #24005, #9169 ) ;
#26655 = CARTESIAN_POINT ( 'NONE',  ( 2.140527761532491802, 7.619874298175139948, 10.49999999999999822 ) ) ;
#26656 = CARTESIAN_POINT ( 'NONE',  ( 25.98021325959672723, -4.875178728621328617, 20.50957957746029336 ) ) ;
#26657 = TOROIDAL_SURFACE ( 'NONE', #31845, 16.00000000000000000, 2.000000000000000000 ) ;
#26658 = CARTESIAN_POINT ( 'NONE',  ( 15.48507841534874174, -21.65259304786752992, -17.10787087048629473 ) ) ;
#26659 = CARTESIAN_POINT ( 'NONE',  ( 12.03640989728592459, 29.14264673470096767, 12.00000000000000000 ) ) ;
#26660 = DIRECTION ( 'NONE',  ( 0.000000000000000000, 0.000000000000000000, 1.000000000000000000 ) ) ;
#26661 = CYLINDRICAL_SURFACE ( 'NONE', #5791, 1.000000000000000888 ) ;
#26662 = EDGE_CURVE ( 'NONE', #6928, #26114, #11217, .T. ) ;
#26663 = ORIENTED_EDGE ( 'NONE', *, *, #15825, .F. ) ;
#26664 = CARTESIAN_POINT ( 'NONE',  ( 14.48160356497363210, 25.11524105193378631, -11.58817748003706249 ) ) ;
#26665 = ORIENTED_EDGE ( 'NONE', *, *, #34779, .T. ) ;
#26666 = CARTESIAN_POINT ( 'NONE',  ( -15.47773846523890917, 25.89138777182121842, -7.360181588512314299 ) ) ;
#26667 = CARTESIAN_POINT ( 'NONE',  ( -28.63945468191068500, -5.523831429905184720, 19.99202127657074612 ) ) ;
#26668 = FACE_OUTER_BOUND ( 'NONE', #39261, .T. ) ;
#26669 = CARTESIAN_POINT ( 'NONE',  ( 12.18240653381212546, 19.86309505633298400, -20.55012464957514240 ) ) ;
#26670 = EDGE_CURVE ( 'NONE', #13041, #22404, #32368, .T. ) ;
#26671 = ORIENTED_EDGE ( 'NONE', *, *, #18716, .T. ) ;
#26672 = CARTESIAN_POINT ( 'NONE',  ( 18.20742805688900745, -10.77041048090527475, -26.25434379449587752 ) ) ;
#26673 = VECTOR ( 'NONE', #177, 1000.000000000000000 ) ;
#26674 = ORIENTED_EDGE ( 'NONE', *, *, #32462, .T. ) ;
#26676 = DIRECTION ( 'NONE',  ( 0.000000000000000000, 0.000000000000000000, 1.000000000000000000 ) ) ;
#26675 = CARTESIAN_POINT ( 'NONE',  ( -10.58469681223512637, 17.55611623359288131, -29.99999999999999289 ) ) ;
#26677 = CARTESIAN_POINT ( 'NONE',  ( -12.80954651559351554, -20.78165554548692739, -19.34070390230921888 ) ) ;
#26678 = LINE ( 'NONE', #39066, #4313 ) ;
#26679 = VERTEX_POINT ( 'NONE', #23803 ) ;
#26680 = CARTESIAN_POINT ( 'NONE',  ( -35.48442078681456024, -11.08901139838818040, -5.440863991683305478 ) ) ;
#26681 = CARTESIAN_POINT ( 'NONE',  ( -13.47854813221718828, -24.52993117364806608, -12.57113449638200819 ) ) ;
#26682 = DIRECTION ( 'NONE',  ( 0.3090169943749448977, -0.9510565162951543083, 0.000000000000000000 ) ) ;
#26683 = CARTESIAN_POINT ( 'NONE',  ( 16.67513756147528525, 21.84779437510598754, -8.337953292251496507 ) ) ;
#26684 = ORIENTED_EDGE ( 'NONE', *, *, #30468, .F. ) ;
#26685 = CARTESIAN_POINT ( 'NONE',  ( 28.38291952110844463, 2.016127822867134878, -8.795360184343094190 ) ) ;
#26686 = CARTESIAN_POINT ( 'NONE',  ( -8.016213763118818392, 9.982035245863954742, 10.49999999999999822 ) ) ;
#26687 = CARTESIAN_POINT ( 'NONE',  ( -14.48927117870124270, -30.61587158504648087, 11.00000000000000000 ) ) ;
#26688 = ORIENTED_EDGE ( 'NONE', *, *, #16815, .T. ) ;
#26689 = CARTESIAN_POINT ( 'NONE',  ( -26.02112680601035422, 0.05871972700698699366, -16.41040207964921294 ) ) ;
#26690 = CARTESIAN_POINT ( 'NONE',  ( 21.37444128088304041, -0.04091218078597470137, -24.92512316553253271 ) ) ;
#26691 = AXIS2_PLACEMENT_3D ( 'NONE', #23362, #35958, #38394 ) ;
#26692 = CARTESIAN_POINT ( 'NONE',  ( 29.18141975161354651, -3.595827299475466532, 19.27171037444328405 ) ) ;
#26693 = AXIS2_PLACEMENT_3D ( 'NONE', #8560, #14451, #24196 ) ;
#26694 = EDGE_CURVE ( 'NONE', #5105, #30551, #20747, .T. ) ;
#26695 = EDGE_LOOP ( 'NONE', ( #34469, #32327, #36586 ) ) ;
#26696 = CARTESIAN_POINT ( 'NONE',  ( -20.44235121065545613, 1.535337040937289510, -30.00000000000000000 ) ) ;
#26697 = EDGE_CURVE ( 'NONE', #29281, #24654, #5314, .T. ) ;
#26698 = CARTESIAN_POINT ( 'NONE',  ( -22.52744239175981278, -0.1803094636421871677, -30.00000000000000000 ) ) ;
#26699 = FACE_OUTER_BOUND ( 'NONE', #1562, .T. ) ;
#26700 = CARTESIAN_POINT ( 'NONE',  ( 13.63581098909226874, 27.45627467658428955, 7.000000000000000000 ) ) ;
#26701 = VECTOR ( 'NONE', #18691, 1000.000000000000227 ) ;
#26702 = LINE ( 'NONE', #26302, #27915 ) ;
#26703 = DIRECTION ( 'NONE',  ( 1.000000000000000000, 0.000000000000000000, 0.000000000000000000 ) ) ;
#26704 = FACE_OUTER_BOUND ( 'NONE', #13345, .T. ) ;
#26705 = VERTEX_POINT ( 'NONE', #17921 ) ;
#26706 = CARTESIAN_POINT ( 'NONE',  ( -20.65325954363973793, 5.772693315354555210, -23.19235817845973102 ) ) ;
#26707 = DIRECTION ( 'NONE',  ( 0.000000000000000000, 0.000000000000000000, 1.000000000000000000 ) ) ;
#26708 = FACE_OUTER_BOUND ( 'NONE', #13754, .T. ) ;
#26709 = CARTESIAN_POINT ( 'NONE',  ( 19.41133145638843871, -19.02227157888451714, -17.76749197532162583 ) ) ;
#26710 = CYLINDRICAL_SURFACE ( 'NONE', #21624, 0.5000000000000004441 ) ;
#26711 = CARTESIAN_POINT ( 'NONE',  ( 8.401171878996485987, 21.11424711454080594, 9.000000000000001776 ) ) ;
#26712 = B_SPLINE_CURVE_WITH_KNOTS ( 'NONE', 3,
 ( #37820, #13231, #16289, #13638, #22775, #31728 ),
 .UNSPECIFIED., .F., .F.,
 ( 4, 2, 4 ),
 ( 0.000000000000000000, 0.4666667928354990558, 0.9333335856709981115 ),
 .UNSPECIFIED. ) ;
#26713 = EDGE_CURVE ( 'NONE', #19050, #25293, #33615, .T. ) ;
#26714 = CARTESIAN_POINT ( 'NONE',  ( 10.72171203101364867, 17.52793616594421877, -28.69511805704588170 ) ) ;
#26715 = CARTESIAN_POINT ( 'NONE',  ( 5.050662510305750530, -26.77689918168226058, 11.00000000000000000 ) ) ;
#26716 = ORIENTED_EDGE ( 'NONE', *, *, #30897, .F. ) ;
#26717 = CIRCLE ( 'NONE', #34439, 0.5000000000000007772 ) ;
#26718 = CARTESIAN_POINT ( 'NONE',  ( -16.84357371261561198, 21.61857896997960893, -7.862167963560605877 ) ) ;
#26719 = CARTESIAN_POINT ( 'NONE',  ( -20.92112759555556067, -16.07000418475133330, 20.99999999999999645 ) ) ;
#26720 = DIRECTION ( 'NONE',  ( -0.000000000000000000, -0.000000000000000000, -1.000000000000000000 ) ) ;
#26721 = CARTESIAN_POINT ( 'NONE',  ( 10.99531269100861763, 17.30182433700542788, -29.34858954477268611 ) ) ;
#26722 = ORIENTED_EDGE ( 'NONE', *, *, #18412, .T. ) ;
#26723 = CARTESIAN_POINT ( 'NONE',  ( -14.97009266215794554, 21.42933399866948818, 10.49999999999999822 ) ) ;
#26724 = ORIENTED_EDGE ( 'NONE', *, *, #3908, .T. ) ;
#26726 = DIRECTION ( 'NONE',  ( -0.000000000000000000, 0.000000000000000000, 1.000000000000000000 ) ) ;
#26725 = CARTESIAN_POINT ( 'NONE',  ( -11.10439374658453637, 17.81390274193991274, -26.21621397894739403 ) ) ;
#26727 = EDGE_CURVE ( 'NONE', #2950, #37992, #35648, .T. ) ;
#26728 = CARTESIAN_POINT ( 'NONE',  ( -9.632883284787542522, -18.33499355343117543, -27.44695152100973701 ) ) ;
#26729 = CARTESIAN_POINT ( 'NONE',  ( -37.51589702892751887, -12.89337557385609401, 10.99999999999969269 ) ) ;
#26730 = CARTESIAN_POINT ( 'NONE',  ( -32.09753123880218340, -19.38851364860806470, -8.404147750168046827 ) ) ;
#26731 = CARTESIAN_POINT ( 'NONE',  ( -5.215330786035433874, -21.06133893932229029, -22.11287648887297408 ) ) ;
#26732 = CARTESIAN_POINT ( 'NONE',  ( 15.30762326431969456, 23.80283413495887501, -10.68953207114196680 ) ) ;
#26733 = ORIENTED_EDGE ( 'NONE', *, *, #20256, .T. ) ;
#26734 = CARTESIAN_POINT ( 'NONE',  ( 19.52319669605035912, 6.624509332748552026, -27.69642029748051471 ) ) ;
#26735 = DIRECTION ( 'NONE',  ( 0.000000000000000000, 0.000000000000000000, 1.000000000000000000 ) ) ;
#26736 = AXIS2_PLACEMENT_3D ( 'NONE', #9059, #12302, #39532 ) ;
#26737 = CARTESIAN_POINT ( 'NONE',  ( 23.05386822411318803, -7.747535282638377652, 23.00000000000000000 ) ) ;
#26738 = FACE_OUTER_BOUND ( 'NONE', #10479, .T. ) ;
#26739 = ORIENTED_EDGE ( 'NONE', *, *, #15807, .F. ) ;
#26740 = CARTESIAN_POINT ( 'NONE',  ( -22.62547799901289025, -1.388567265765580760, -22.47904496567277022 ) ) ;
#26741 = CARTESIAN_POINT ( 'NONE',  ( 27.16112558961255630, 0.2057471714452771827, -14.47458546668211454 ) ) ;
#26742 = DIRECTION ( 'NONE',  ( -0.000000000000000000, -0.000000000000000000, 1.000000000000000000 ) ) ;
#26743 = CARTESIAN_POINT ( 'NONE',  ( 24.39151161285758107, -15.73551128733868865, 20.94377226548388293 ) ) ;
#26744 = CARTESIAN_POINT ( 'NONE',  ( 9.625795778761983001, 10.95253033666821274, 7.000000000000000000 ) ) ;
#26745 = EDGE_CURVE ( 'NONE', #7299, #880, #607, .T. ) ;
#26746 = CARTESIAN_POINT ( 'NONE',  ( 36.53369576860743706, -5.154516326609254406, 11.00000000000007994 ) ) ;
#26747 = AXIS2_PLACEMENT_3D ( 'NONE', #5326, #10827, #38857 ) ;
#26748 = ORIENTED_EDGE ( 'NONE', *, *, #5914, .T. ) ;
#26749 = DIRECTION ( 'NONE',  ( 0.000000000000000000, 0.000000000000000000, 1.000000000000000000 ) ) ;
#26750 = DIRECTION ( 'NONE',  ( -0.1045284632676570929, -0.9945218953682730678, 0.000000000000000000 ) ) ;
#26751 = ORIENTED_EDGE ( 'NONE', *, *, #18470, .T. ) ;
#26752 = CARTESIAN_POINT ( 'NONE',  ( 0.2626407527151565779, 24.68515879224474929, -20.69159593321769464 ) ) ;
#26753 = DIRECTION ( 'NONE',  ( 0.000000000000000000, 0.000000000000000000, 1.000000000000000000 ) ) ;
#26754 = DIRECTION ( 'NONE',  ( 0.000000000000000000, 0.000000000000000000, 1.000000000000000000 ) ) ;
#26755 = CIRCLE ( 'NONE', #31939, 1.000000000000000888 ) ;
#26756 = CARTESIAN_POINT ( 'NONE',  ( 6.811226782241714517, 35.33967249274190436, 11.00000000000000000 ) ) ;
#26757 = DIRECTION ( 'NONE',  ( 0.8660254037844377084, -0.5000000000000019984, 0.000000000000000000 ) ) ;
#26758 = EDGE_CURVE ( 'NONE', #7299, #19863, #14232, .T. ) ;
#26759 = CARTESIAN_POINT ( 'NONE',  ( 9.408554248005412290, 10.90613044664325670, 10.49999999999999822 ) ) ;
#26760 = CARTESIAN_POINT ( 'NONE',  ( 12.35707315130249562, 23.65243939895810144, -16.27315544969195571 ) ) ;
#26761 = CARTESIAN_POINT ( 'NONE',  ( 35.48538791413476190, -11.24999995268670006, -5.000000000000002665 ) ) ;
#26762 = ORIENTED_EDGE ( 'NONE', *, *, #32867, .T. ) ;
#26764 = CARTESIAN_POINT ( 'NONE',  ( 5.034171952702015673, 35.03623199971300295, 10.00000000000000000 ) ) ;
#26763 = CARTESIAN_POINT ( 'NONE',  ( -18.72571766207202160, 17.65421610605874747, -5.960612349730155302 ) ) ;
#26765 = CYLINDRICAL_SURFACE ( 'NONE', #9485, 0.5000000000000004441 ) ;
#26766 = ADVANCED_FACE ( 'NONE', ( #28444 ), #37195, .F. ) ;
#26767 = CARTESIAN_POINT ( 'NONE',  ( 9.649927930759803374, -18.32663946374046660, -27.44572378285204550 ) ) ;
#26768 = DIRECTION ( 'NONE',  ( -0.000000000000000000, -0.000000000000000000, -1.000000000000000000 ) ) ;
#26769 = CARTESIAN_POINT ( 'NONE',  ( 14.82926489102576184, 25.64310198477804192, -10.17817126611451783 ) ) ;
#26770 = CARTESIAN_POINT ( 'NONE',  ( -16.72075857324140102, 7.444561356925720297, 7.000000000000000000 ) ) ;
#26771 = DIRECTION ( 'NONE',  ( 0.000000000000000000, 0.000000000000000000, -1.000000000000000000 ) ) ;
#26772 = ADVANCED_FACE ( 'NONE', ( #19105, #40030 ), #25000, .T. ) ;
#26773 = CARTESIAN_POINT ( 'NONE',  ( -26.09240205010872060, -24.51935322919086602, -8.901813507160523997 ) ) ;
#26774 = CARTESIAN_POINT ( 'NONE',  ( 3.334020111461103664, -22.39794475360687542, -17.98710033329706803 ) ) ;
#26775 = CARTESIAN_POINT ( 'NONE',  ( 14.97853101390886010, 25.19679915242138080, -10.18807554250177816 ) ) ;
#26776 = CARTESIAN_POINT ( 'NONE',  ( 17.58948748090468328, 12.74787095466262343, -21.15892960070590334 ) ) ;
#26777 = LINE ( 'NONE', #5845, #14082 ) ;
#26778 = ORIENTED_EDGE ( 'NONE', *, *, #18987, .T. ) ;
#26779 = CARTESIAN_POINT ( 'NONE',  ( -7.424996026816661043, 36.56248452709654373, -6.293540445570466879 ) ) ;
#26780 = ORIENTED_EDGE ( 'NONE', *, *, #27420, .T. ) ;
#26781 = AXIS2_PLACEMENT_3D ( 'NONE', #37449, #31155, #12461 ) ;
#26782 = FACE_OUTER_BOUND ( 'NONE', #34443, .T. ) ;
#26783 = VERTEX_POINT ( 'NONE', #3065 ) ;
#26784 = CARTESIAN_POINT ( 'NONE',  ( -2.140527761532693418, 7.619874298175171035, 11.00000000000000000 ) ) ;
#26785 = CIRCLE ( 'NONE', #13172, 1.000000000000000000 ) ;
#26786 = CARTESIAN_POINT ( 'NONE',  ( -1.494943660522439099, 10.76222879119470832, 13.00000000000000178 ) ) ;
#26787 = ORIENTED_EDGE ( 'NONE', *, *, #4667, .T. ) ;
#26788 = CARTESIAN_POINT ( 'NONE',  ( -20.47628691903608811, 0.9865603022909631425, -30.00000000000000000 ) ) ;
#26789 = EDGE_CURVE ( 'NONE', #6055, #9203, #15659, .T. ) ;
#26790 = B_SPLINE_CURVE_WITH_KNOTS ( 'NONE', 3,
 ( #30630, #21472, #30433, #36723, #8887, #9087, #18236, #39561, #24717, #21275, #27965, #6231, #2991, #14982, #20886, #33877, #33288, #27369 ),
 .UNSPECIFIED., .F., .F.,
 ( 4, 2, 2, 2, 2, 2, 2, 2, 4 ),
 ( 0.000000000000000000, 0.1249999999999998335, 0.2499999999999996669, 0.3749999999999995004, 0.4999999999999993339, 0.6249999999999994449, 0.7499999999999996669, 0.8749999999999997780, 1.000000000000000000 ),
 .UNSPECIFIED. ) ;
#26791 = VERTEX_POINT ( 'NONE', #9369 ) ;
#26792 = CARTESIAN_POINT ( 'NONE',  ( 34.00946725009706029, -11.35794860730630162, -9.327975789640845505 ) ) ;
#26793 = ADVANCED_FACE ( 'NONE', ( #31102 ), #31498, .F. ) ;
#26794 = AXIS2_PLACEMENT_3D ( 'NONE', #13634, #19735, #22174 ) ;
#26795 = ORIENTED_EDGE ( 'NONE', *, *, #33265, .T. ) ;
#26796 = ITEM_DEFINED_TRANSFORMATION ( 'NONE', 'NONE', #1526,  #24238 ) ;
#26797 = CARTESIAN_POINT ( 'NONE',  ( -0.5000000000000000000, 37.50000000000000711, 10.63089969389957190 ) ) ;
#26798 = ORIENTED_EDGE ( 'NONE', *, *, #30238, .F. ) ;
#26799 = DIRECTION ( 'NONE',  ( 0.000000000000000000, 0.000000000000000000, -1.000000000000000000 ) ) ;
#26800 = CARTESIAN_POINT ( 'NONE',  ( 6.506711629694180488, 35.47525137376717908, 10.83333333333333037 ) ) ;
#26801 = CIRCLE ( 'NONE', #8657, 6.000000000000003553 ) ;
#26802 = CARTESIAN_POINT ( 'NONE',  ( 4.727507481117211086, 31.88885898370940453, 10.50000000000000000 ) ) ;
#26803 = VERTEX_POINT ( 'NONE', #12210 ) ;
#26804 = CARTESIAN_POINT ( 'NONE',  ( -14.16516198183350639, -14.87677494158405977, -30.00000000000001421 ) ) ;
#26805 = PLANE ( 'NONE',  #20226 ) ;
#26806 = VECTOR ( 'NONE', #15154, 1000.000000000000000 ) ;
#26807 = CARTESIAN_POINT ( 'NONE',  ( -1.590043107810761525, 12.61456814725308817, 10.50000000000001066 ) ) ;
#26808 = ADVANCED_FACE ( 'NONE', ( #21745 ), #39548, .T. ) ;
#26809 = CARTESIAN_POINT ( 'NONE',  ( 18.41721206756663776, 17.73514788426912858, -8.380454930519549706 ) ) ;
#26810 = VECTOR ( 'NONE', #14356, 1000.000000000000000 ) ;
#26811 = CARTESIAN_POINT ( 'NONE',  ( 6.908205946113894491, 19.31174812457788548, -30.00000000000000000 ) ) ;
#26812 = VERTEX_POINT ( 'NONE', #37599 ) ;
#26813 = CARTESIAN_POINT ( 'NONE',  ( 12.68475447279711688, 27.14725768220934299, 9.500000000000000000 ) ) ;
#26814 = CARTESIAN_POINT ( 'NONE',  ( -1.829593030691901284E-15, 22.50000000000001066, 3.000000000000000000 ) ) ;
#26815 = ADVANCED_FACE ( 'NONE', ( #13001 ), #9765, .T. ) ;
#26816 = CARTESIAN_POINT ( 'NONE',  ( 15.94498026452435901, -26.77773472525574405, -6.408825021150274637 ) ) ;
#26817 = DIRECTION ( 'NONE',  ( 0.5877852522924689183, -0.8090169943749505599, -0.000000000000000000 ) ) ;
#26818 = CARTESIAN_POINT ( 'NONE',  ( 16.24796006241085422, 15.88921519459651144, -21.50719306941225639 ) ) ;
#26819 = CARTESIAN_POINT ( 'NONE',  ( -15.16784012994541087, 26.30413795963287527, -8.296983500820855895 ) ) ;
#26820 = VECTOR ( 'NONE', #23665, 1000.000000000000114 ) ;
#26821 = CARTESIAN_POINT ( 'NONE',  ( -27.69088631810926415, -26.08775134479659741, 15.13084544680184074 ) ) ;
#26822 = CARTESIAN_POINT ( 'NONE',  ( 9.319357777823674027, -19.06942296064119802, -25.08597432989563814 ) ) ;
#26823 = CARTESIAN_POINT ( 'NONE',  ( 14.11133924723984379, 27.61078317377175750, 10.49999999999999822 ) ) ;
#26824 = ORIENTED_EDGE ( 'NONE', *, *, #3158, .F. ) ;
#26825 = EDGE_LOOP ( 'NONE', ( #1051, #38714, #21906, #10542 ) ) ;
#26826 = CARTESIAN_POINT ( 'NONE',  ( -11.56028495311938720, 32.06293909086500094, -8.988039450567926636 ) ) ;
#26827 = LINE ( 'NONE', #39217, #34093 ) ;
#26828 = CIRCLE ( 'NONE', #9318, 1.000000000000000888 ) ;
#26829 = CARTESIAN_POINT ( 'NONE',  ( -2.317734025672947951, 9.191051544684766483, 7.000000000000000000 ) ) ;
#26830 = DIRECTION ( 'NONE',  ( 1.000000000000000000, 0.000000000000000000, 0.000000000000000000 ) ) ;
#26831 = EDGE_LOOP ( 'NONE', ( #31657, #39263, #15259, #38232 ) ) ;
#26832 = CARTESIAN_POINT ( 'NONE',  ( 24.52064454744603594, 0.5127890810554470713, -18.46105024167576403 ) ) ;
#26833 = LINE ( 'NONE', #17710, #8329 ) ;
#26834 = DIRECTION ( 'NONE',  ( 0.5720614028176875809, -0.4156269377774574059, 0.7071067811865425767 ) ) ;
#26835 = CARTESIAN_POINT ( 'NONE',  ( -34.30322546405390227, -21.55963432478805331, 11.00000000000007105 ) ) ;
#26836 = VERTEX_POINT ( 'NONE', #25389 ) ;
#26837 = CARTESIAN_POINT ( 'NONE',  ( -30.33764259824372900, 0.01140825290230679939, -8.297842417475935761 ) ) ;
#26838 = CARTESIAN_POINT ( 'NONE',  ( -13.63581098909220479, 27.45627467658446008, 7.499999999999993783 ) ) ;
#26839 = ORIENTED_EDGE ( 'NONE', *, *, #25648, .T. ) ;
#26840 = CARTESIAN_POINT ( 'NONE',  ( 25.12025796159581859, -3.672407670025477522, -19.02952475234523888 ) ) ;
#26841 = AXIS2_PLACEMENT_3D ( 'NONE', #13104, #27954, #19012 ) ;
#26842 = CARTESIAN_POINT ( 'NONE',  ( 27.83556507003290648, -26.34944855520544493, 14.53008259253983070 ) ) ;
#26843 = EDGE_LOOP ( 'NONE', ( #27668, #22146, #23038, #29553 ) ) ;
#26844 =( GEOMETRIC_REPRESENTATION_CONTEXT ( 3 ) GLOBAL_UNCERTAINTY_ASSIGNED_CONTEXT ( ( #38426 ) ) GLOBAL_UNIT_ASSIGNED_CONTEXT ( ( #7912, #38392, #7300 ) ) REPRESENTATION_CONTEXT ( 'NONE', 'WORKASPACE' ) );
#26845 = CARTESIAN_POINT ( 'NONE',  ( -13.15434222961970612, 33.66598129999007227, 14.53008259254024281 ) ) ;
#26846 = EDGE_CURVE ( 'NONE', #22349, #3843, #15458, .T. ) ;
#26847 = CARTESIAN_POINT ( 'NONE',  ( 4.269643690484067594E-14, -24.31502561551697283, 16.87380292611441845 ) ) ;
#26848 = DIRECTION ( 'NONE',  ( -0.6916548014802257338, 0.1470157664652036178, -0.7071067811865463515 ) ) ;
#26849 = CARTESIAN_POINT ( 'NONE',  ( 4.721973484737132409, 30.34170004520692032, 20.50957957746029692 ) ) ;
#26850 = AXIS2_PLACEMENT_3D ( 'NONE', #31444, #763, #12354 ) ;
#26851 = CARTESIAN_POINT ( 'NONE',  ( 10.10646936306337729, 32.94553861768082470, 7.000000000000000000 ) ) ;
#26852 = VERTEX_POINT ( 'NONE', #27646 ) ;
#26853 = CARTESIAN_POINT ( 'NONE',  ( -8.768078002823386896, 24.93711404285670952, 20.50957957746029692 ) ) ;
#26854 = CARTESIAN_POINT ( 'NONE',  ( 14.52509594610761923, 21.97885917798724975, 10.49999999999999822 ) ) ;
#26855 = CARTESIAN_POINT ( 'NONE',  ( 6.925036540929339957, 35.55535081222223681, -8.883103387068663537 ) ) ;
#26856 = CARTESIAN_POINT ( 'NONE',  ( 7.468455364333220992, 29.89744377950669474, 10.00000000000000000 ) ) ;
#26857 = CIRCLE ( 'NONE', #8711, 1.000000000000000000 ) ;
#26858 = CARTESIAN_POINT ( 'NONE',  ( 27.14644468510626041, -3.730463242941437496, 19.99202127657103389 ) ) ;
#26859 = CARTESIAN_POINT ( 'NONE',  ( 15.74947785296019021, -20.78724321937316333, -18.03682299684260570 ) ) ;
#26860 = CARTESIAN_POINT ( 'NONE',  ( 13.48130249190479368, 27.93180293473185927, 11.00000000000000000 ) ) ;
#26861 = CARTESIAN_POINT ( 'NONE',  ( -13.23567246089835869, 15.94827353674837767, 10.49999999999999822 ) ) ;
#26862 = CARTESIAN_POINT ( 'NONE',  ( 2.535262076962677913, 8.167662524929967915, 11.00000000000000355 ) ) ;
#26863 = ORIENTED_EDGE ( 'NONE', *, *, #4895, .T. ) ;
#26864 = CARTESIAN_POINT ( 'NONE',  ( 13.14824004184070638, 22.34849671386530190, -16.42994992985817149 ) ) ;
#26865 = AXIS2_PLACEMENT_3D ( 'NONE', #24013, #20377, #39050 ) ;
#26866 = EDGE_LOOP ( 'NONE', ( #28876, #14903, #12895, #35325 ) ) ;
#26867 = CARTESIAN_POINT ( 'NONE',  ( -15.29345365570516435, 25.52021322302956818, -8.773791920665329869 ) ) ;
#26868 = CARTESIAN_POINT ( 'NONE',  ( -31.98112326865703992, -15.20435932463186113, 18.87996532025782415 ) ) ;
#26869 = EDGE_CURVE ( 'NONE', #29611, #25142, #24892, .T. ) ;
#26870 = CARTESIAN_POINT ( 'NONE',  ( -14.31632963181202456, 26.62592636301959814, 10.82238861112336714 ) ) ;
#26871 = CARTESIAN_POINT ( 'NONE',  ( 12.21409306628939184, 19.82566689378781888, -20.55567861157228648 ) ) ;
#26872 = ORIENTED_EDGE ( 'NONE', *, *, #21575, .F. ) ;
#26873 = CARTESIAN_POINT ( 'NONE',  ( 27.95286989306738690, -16.54226243461976154, -13.80388540367800054 ) ) ;
#26874 = ORIENTED_EDGE ( 'NONE', *, *, #17749, .T. ) ;
#26876 = CARTESIAN_POINT ( 'NONE',  ( -5.440908595777636414, 35.94977745735568675, 11.00000000000000000 ) ) ;
#26875 = CARTESIAN_POINT ( 'NONE',  ( -13.26571186845993289, 23.26405244385044924, -15.39968056061676549 ) ) ;
#26877 = CARTESIAN_POINT ( 'NONE',  ( -10.23258877305064196, -17.82419513942780753, -28.67841817144874739 ) ) ;
#26878 = CARTESIAN_POINT ( 'NONE',  ( -7.713869163866016621, 10.18146832927085121, 7.000000000000000000 ) ) ;
#26879 = CIRCLE ( 'NONE', #32720, 16.00000000000000000 ) ;
#26880 = EDGE_LOOP ( 'NONE', ( #8591, #21897, #14252, #33840 ) ) ;
#26881 = CARTESIAN_POINT ( 'NONE',  ( -34.55718164801944425, -11.87514214786398448, -8.441259157958310055 ) ) ;
#26882 = CARTESIAN_POINT ( 'NONE',  ( -9.018257521923398912, -18.41052938026230024, -30.00000000000000000 ) ) ;
#26883 = CARTESIAN_POINT ( 'NONE',  ( 13.95683075005237050, 28.08631143191933432, 7.000000000000000000 ) ) ;
#26884 = ORIENTED_EDGE ( 'NONE', *, *, #8164, .F. ) ;
#26885 = CARTESIAN_POINT ( 'NONE',  ( 28.97648499451679527, 1.995013090243813236, -5.474227664210660649 ) ) ;
#26886 = CARTESIAN_POINT ( 'NONE',  ( -7.899339922805356018, 10.02167583667232265, 10.49999999999999822 ) ) ;
#26887 = FACE_OUTER_BOUND ( 'NONE', #28261, .T. ) ;
#26888 = ORIENTED_EDGE ( 'NONE', *, *, #9621, .T. ) ;
#26889 = CARTESIAN_POINT ( 'NONE',  ( -29.87381286097529198, -0.03451733885659702405, -9.704015530497390074 ) ) ;
#26890 = CARTESIAN_POINT ( 'NONE',  ( 20.50011096633554786, 0.05624224123783942708, -29.33361002156190978 ) ) ;
#26891 = AXIS2_PLACEMENT_3D ( 'NONE', #33568, #25349, #28399 ) ;
#26892 = CARTESIAN_POINT ( 'NONE',  ( 20.37435360786973959, -23.49902402743850871, 19.27171037444156099 ) ) ;
#26893 = EDGE_CURVE ( 'NONE', #32909, #14918, #23316, .T. ) ;
#26894 = ORIENTED_EDGE ( 'NONE', *, *, #14361, .F. ) ;
#26895 = CARTESIAN_POINT ( 'NONE',  ( -26.41979680957344812, 2.663940752761243758, -12.66501335940618311 ) ) ;
#26896 = DIRECTION ( 'NONE',  ( 1.000000000000000000, 0.000000000000000000, -0.000000000000000000 ) ) ;
#26897 = CIRCLE ( 'NONE', #9379, 16.00000000000000000 ) ;
#26898 = CARTESIAN_POINT ( 'NONE',  ( -8.843266739736659332, 16.81698729810787185, 10.00000000000000000 ) ) ;
#26899 = CARTESIAN_POINT ( 'NONE',  ( -15.37000524125038048, -27.20210912714572160, 15.72805884748939853 ) ) ;
#26900 = EDGE_CURVE ( 'NONE', #24946, #33412, #16056, .T. ) ;
#26901 = EDGE_CURVE ( 'NONE', #25736, #23174, #30704, .T. ) ;
#26902 = VECTOR ( 'NONE', #27167, 1000.000000000000114 ) ;
#26903 = CIRCLE ( 'NONE', #16523, 1.000000000000000888 ) ;
#26904 = FACE_OUTER_BOUND ( 'NONE', #27982, .T. ) ;
#26905 = DIRECTION ( 'NONE',  ( 0.000000000000000000, 0.000000000000000000, 1.000000000000000000 ) ) ;
#26906 = PLANE ( 'NONE',  #17267 ) ;
#26907 = ORIENTED_EDGE ( 'NONE', *, *, #710, .T. ) ;
#26908 = CARTESIAN_POINT ( 'NONE',  ( -24.91587395908689828, 6.157934535019561118, -9.832588768546241198 ) ) ;
#26909 = FACE_OUTER_BOUND ( 'NONE', #29367, .T. ) ;
#26910 = DIRECTION ( 'NONE',  ( 0.9135454576426005335, -0.4067366430758009299, 0.000000000000000000 ) ) ;
#26911 = CARTESIAN_POINT ( 'NONE',  ( 14.80116457086245063, -14.50031048367034003, -27.79137631540835329 ) ) ;
#26912 = DIRECTION ( 'NONE',  ( 0.000000000000000000, 0.000000000000000000, 1.000000000000000000 ) ) ;
#26913 = CARTESIAN_POINT ( 'NONE',  ( -14.72308455763294077, 20.12562289931506854, 10.49999999999999822 ) ) ;
#26914 = CARTESIAN_POINT ( 'NONE',  ( 15.22398294079505732, 27.00394357737293660, -6.879655644394929936 ) ) ;
#26915 = CARTESIAN_POINT ( 'NONE',  ( -5.146739273647190416, -25.63390596715193936, 15.13084544680213739 ) ) ;
#26916 = ORIENTED_EDGE ( 'NONE', *, *, #19201, .T. ) ;
#26917 = CARTESIAN_POINT ( 'NONE',  ( -13.95161305026674015, 16.60687172368021081, -23.05558987895942380 ) ) ;
#26918 = EDGE_CURVE ( 'NONE', #28310, #27267, #4491, .T. ) ;
#26919 = CARTESIAN_POINT ( 'NONE',  ( -20.02374874442591590, -18.66705478562314013, 20.82122704794079837 ) ) ;
#26920 = ADVANCED_FACE ( 'NONE', ( #21950 ), #6500, .F. ) ;
#26921 = EDGE_CURVE ( 'NONE', #13267, #36570, #18512, .T. ) ;
#26922 = CARTESIAN_POINT ( 'NONE',  ( -11.44473057578096764, 31.45924896672619298, 10.49999999999999822 ) ) ;
#26923 = CARTESIAN_POINT ( 'NONE',  ( 11.13905890951745548, 17.60318892418004566, -26.83172267188130533 ) ) ;
#26924 = VERTEX_POINT ( 'NONE', #1225 ) ;
#26925 = CARTESIAN_POINT ( 'NONE',  ( 10.98647152928299597, 17.30743895948370081, -29.34839841643595904 ) ) ;
#26926 = ORIENTED_EDGE ( 'NONE', *, *, #19695, .F. ) ;
#26928 = CARTESIAN_POINT ( 'NONE',  ( 9.941034666242805073, 32.57396620494213124, 9.500000000000000000 ) ) ;
#26927 = CARTESIAN_POINT ( 'NONE',  ( -11.12155928551759132, 17.80160828069594459, -26.21807330386510060 ) ) ;
#26929 = CARTESIAN_POINT ( 'NONE',  ( -13.79154419894701711, -24.12836806479996099, -13.50637930408640486 ) ) ;
#26930 = CARTESIAN_POINT ( 'NONE',  ( -36.53368004180963169, -5.154483866377390200, 11.55979286843969511 ) ) ;
#26931 = VECTOR ( 'NONE', #1047, 1000.000000000000000 ) ;
#26932 = CARTESIAN_POINT ( 'NONE',  ( -24.36260255128434693, -13.71872778104093626, -17.59360786939599919 ) ) ;
#26933 = CARTESIAN_POINT ( 'NONE',  ( -7.584868861406902418, -22.23149659495907216, -17.80198783937951035 ) ) ;
#26934 = CARTESIAN_POINT ( 'NONE',  ( 9.831584923911636409, 26.22020669908449975, 10.50000000000000000 ) ) ;
#26935 = CARTESIAN_POINT ( 'NONE',  ( 15.39490642557507805, 24.42544543857336237, -9.730889705983216231 ) ) ;
#26936 = VERTEX_POINT ( 'NONE', #13604 ) ;
#26937 = CARTESIAN_POINT ( 'NONE',  ( 24.00150849657053342, 7.288234594027279023, -10.34479505154993006 ) ) ;
#26938 = DIRECTION ( 'NONE',  ( 0.000000000000000000, 0.000000000000000000, 1.000000000000000000 ) ) ;
#26939 = FACE_OUTER_BOUND ( 'NONE', #27593, .T. ) ;
#26940 = CARTESIAN_POINT ( 'NONE',  ( 2.587660364795204782, 9.681887955242936883, 12.00000000000000000 ) ) ;
#26941 = CIRCLE ( 'NONE', #9417, 15.00000000000000000 ) ;
#26942 = ORIENTED_EDGE ( 'NONE', *, *, #4519, .T. ) ;
#26943 = CARTESIAN_POINT ( 'NONE',  ( -20.50243331965346627, -0.1390943044478715751, -30.00000000000000000 ) ) ;
#26944 = CARTESIAN_POINT ( 'NONE',  ( 26.54774961419984791, 0.2119857837146491009, -15.44276492342872942 ) ) ;
#26945 = VECTOR ( 'NONE', #8447, 1000.000000000000000 ) ;
#26946 = DIRECTION ( 'NONE',  ( -0.3090169943749448977, 0.9510565162951543083, 0.000000000000000000 ) ) ;
#26947 = CARTESIAN_POINT ( 'NONE',  ( 19.96384346486630434, -17.84145166816523798, 20.94377226548378701 ) ) ;
#26948 = DIRECTION ( 'NONE',  ( 0.5877852522924689183, -0.8090169943749503378, 0.000000000000000000 ) ) ;
#26949 = ADVANCED_FACE ( 'NONE', ( #13197 ), #35550, .F. ) ;
#26950 = DIRECTION ( 'NONE',  ( 1.000000000000000000, 0.000000000000000000, 0.000000000000000000 ) ) ;
#26951 = CARTESIAN_POINT ( 'NONE',  ( 24.65531199400567175, -28.60128534115908749, 10.99999999999988987 ) ) ;
#26952 = ORIENTED_EDGE ( 'NONE', *, *, #2825, .T. ) ;
#26953 = DIRECTION ( 'NONE',  ( -0.000000000000000000, 0.000000000000000000, 1.000000000000000000 ) ) ;
#26954 = AXIS2_PLACEMENT_3D ( 'NONE', #10793, #23982, #36378 ) ;
#26955 = DIRECTION ( 'NONE',  ( 1.000000000000000000, 0.000000000000000000, 0.000000000000000000 ) ) ;
#26956 = ORIENTED_EDGE ( 'NONE', *, *, #29002, .F. ) ;
#26957 = CARTESIAN_POINT ( 'NONE',  ( 0.3974060216068843188, 36.87773723323857666, -9.281964161181997852 ) ) ;
#26958 = DIRECTION ( 'NONE',  ( 0.9659258262890684232, 0.2588190451025203509, 0.000000000000000000 ) ) ;
#26959 = CARTESIAN_POINT ( 'NONE',  ( 4.817371740575539185, 23.83900317890011422, 20.99999999999999645 ) ) ;
#26960 = PLANE ( 'NONE',  #12914 ) ;
#26961 = CIRCLE ( 'NONE', #3583, 5.999999999999996447 ) ;
#26962 = DIRECTION ( 'NONE',  ( 0.000000000000000000, 0.000000000000000000, 1.000000000000000000 ) ) ;
#26963 = FACE_OUTER_BOUND ( 'NONE', #23545, .T. ) ;
#26964 = DIRECTION ( 'NONE',  ( 1.000000000000000000, 0.000000000000000000, 0.000000000000000000 ) ) ;
#26965 = CARTESIAN_POINT ( 'NONE',  ( 10.88564509527626711, 20.38589894840641037, -21.43542534558934420 ) ) ;
#26967 = CIRCLE ( 'NONE', #32810, 0.9999999999999997780 ) ;
#26966 = DIRECTION ( 'NONE',  ( 0.000000000000000000, 0.000000000000000000, 1.000000000000000000 ) ) ;
#26968 = VERTEX_POINT ( 'NONE', #4668 ) ;
#26971 = DIRECTION ( 'NONE',  ( 0.000000000000000000, 0.000000000000000000, 1.000000000000000000 ) ) ;
#26970 = AXIS2_PLACEMENT_3D ( 'NONE', #19732, #35170, #29278 ) ;
#26969 = CARTESIAN_POINT ( 'NONE',  ( -19.27426644434435943, 15.23580267750421768, -10.36995949012763951 ) ) ;
#26972 = CARTESIAN_POINT ( 'NONE',  ( -6.312041872459064784, 25.58773265502866678, 13.00000000000000178 ) ) ;
#26973 = CARTESIAN_POINT ( 'NONE',  ( 12.67787564303985093, -22.55830435898898045, -16.44121654803666033 ) ) ;
#26974 = EDGE_CURVE ( 'NONE', #5248, #13411, #19514, .T. ) ;
#26975 = DIRECTION ( 'NONE',  ( 1.000000000000000000, 0.000000000000000000, 0.000000000000000000 ) ) ;
#26976 = CARTESIAN_POINT ( 'NONE',  ( 13.19712304331239849, 22.25851351613993501, -16.44121704333481659 ) ) ;
#26977 = FACE_OUTER_BOUND ( 'NONE', #11151, .T. ) ;
#26978 = FACE_OUTER_BOUND ( 'NONE', #6932, .T. ) ;
#26979 = CARTESIAN_POINT ( 'NONE',  ( -15.84100732309063453, -13.15637747550469605, -28.47180823155512286 ) ) ;
#26980 = CARTESIAN_POINT ( 'NONE',  ( 1.757052035680020996, -24.31965863861416466, -9.891202175810470010 ) ) ;
#26981 = CARTESIAN_POINT ( 'NONE',  ( 15.47372898463780899, 26.31603480030968711, -6.417418525855842937 ) ) ;
#26982 = CARTESIAN_POINT ( 'NONE',  ( 20.56691591868512603, 12.65939849767090131, -10.88559607822821640 ) ) ;
#26983 = CARTESIAN_POINT ( 'NONE',  ( -2.494943660522439099, 10.76222879119470832, 12.00000000000000000 ) ) ;
#26984 = EDGE_LOOP ( 'NONE', ( #39067, #30375 ) ) ;
#26985 = CARTESIAN_POINT ( 'NONE',  ( -5.057544419104798905, 24.90275516936592126, -19.74804168192481058 ) ) ;
#26986 = ORIENTED_EDGE ( 'NONE', *, *, #32339, .F. ) ;
#26987 = APPLICATION_CONTEXT ( 'automotive_design' ) ;
#26988 = CARTESIAN_POINT ( 'NONE',  ( -22.19961376577589718, 12.81695298357469426, 15.13084544680213561 ) ) ;
#26989 = ORIENTED_EDGE ( 'NONE', *, *, #3945, .T. ) ;
#26990 = DIRECTION ( 'NONE',  ( -1.000000000000000000, 0.000000000000000000, 0.000000000000000000 ) ) ;
#26991 = CARTESIAN_POINT ( 'NONE',  ( 13.95683075005237050, 28.08631143191933432, 10.50000000000000000 ) ) ;
#26992 = EDGE_LOOP ( 'NONE', ( #4460, #2012, #21783, #20382 ) ) ;
#26993 = CIRCLE ( 'NONE', #1676, 0.5000000000000004441 ) ;
#26994 = CARTESIAN_POINT ( 'NONE',  ( -20.80125368753044057, 0.9936892722615382478, -26.84302245589054081 ) ) ;
#26995 = EDGE_CURVE ( 'NONE', #2021, #4297, #1022, .T. ) ;
#26996 = CARTESIAN_POINT ( 'NONE',  ( 35.47190708691255168, -11.90251233358380212, -5.439855546327714286 ) ) ;
#26997 = AXIS2_PLACEMENT_3D ( 'NONE', #23515, #26567, #7868 ) ;
#26998 = AXIS2_PLACEMENT_3D ( 'NONE', #344, #37516, #26116 ) ;
#26999 = EDGE_CURVE ( 'NONE', #36571, #28556, #5162, .T. ) ;
#27000 = CIRCLE ( 'NONE', #6882, 1.000000000000000000 ) ;
#27001 = EDGE_LOOP ( 'NONE', ( #25229, #10140, #1748, #9251, #16 ) ) ;
#27002 = DIRECTION ( 'NONE',  ( 0.000000000000000000, 0.000000000000000000, 1.000000000000000000 ) ) ;
#27003 = ORIENTED_EDGE ( 'NONE', *, *, #28726, .F. ) ;
#27004 = DIRECTION ( 'NONE',  ( 0.5877852522924801315, 0.8090169943749424553, -0.000000000000000000 ) ) ;
#27005 = LINE ( 'NONE', #39387, #20141 ) ;
#27006 = ADVANCED_FACE ( 'NONE', ( #10164 ), #25991, .F. ) ;
#27007 = CARTESIAN_POINT ( 'NONE',  ( -1.000003370709253492, 22.50000000000031264, 6.000000000000000000 ) ) ;
#27008 = EDGE_LOOP ( 'NONE', ( #27992, #9277, #9009, #37217 ) ) ;
#27009 = DIRECTION ( 'NONE',  ( -1.000000000000000000, 0.000000000000000000, 0.000000000000000000 ) ) ;
#27010 = CARTESIAN_POINT ( 'NONE',  ( 4.794796183863160977, 36.71301971979253409, 7.000000000000000000 ) ) ;
#27011 = LINE ( 'NONE', #39198, #37054 ) ;
#27012 = CARTESIAN_POINT ( 'NONE',  ( 19.19831057544300634, 15.58298917004336381, -9.871960784555227519 ) ) ;
#27013 = CARTESIAN_POINT ( 'NONE',  ( 9.500247868936627427, 26.82341383387064582, -15.94768270033280366 ) ) ;
#27014 = ORIENTED_EDGE ( 'NONE', *, *, #38286, .F. ) ;
#27015 = CARTESIAN_POINT ( 'NONE',  ( -18.81973674586063439, 9.357238322791348040, -24.40929192524837887 ) ) ;
#27016 = DIRECTION ( 'NONE',  ( -0.5877852522924690293, 0.8090169943749504489, 0.000000000000000000 ) ) ;
#27017 = CYLINDRICAL_SURFACE ( 'NONE', #20511, 1.000000000000000000 ) ;
#27018 = CARTESIAN_POINT ( 'NONE',  ( 9.846686707545563522, -18.36693667979134048, -26.81703511278297469 ) ) ;
#27019 = DIRECTION ( 'NONE',  ( 1.000000000000000000, 0.000000000000000000, 0.000000000000000000 ) ) ;
#27020 = EDGE_CURVE ( 'NONE', #31127, #15240, #6897, .T. ) ;
#27021 = EDGE_CURVE ( 'NONE', #3978, #38096, #10997, .T. ) ;
#27022 = DIRECTION ( 'NONE',  ( 0.9781476007338070211, 0.2079116908177534029, -0.000000000000000000 ) ) ;
#27023 = EDGE_CURVE ( 'NONE', #9166, #3260, #35001, .T. ) ;
#27024 = CARTESIAN_POINT ( 'NONE',  ( -12.12621152392383372, 19.92962288602521781, -20.53998900965990160 ) ) ;
#27025 = AXIS2_PLACEMENT_3D ( 'NONE', #30178, #36472, #2549 ) ;
#27026 = CARTESIAN_POINT ( 'NONE',  ( 9.072119448907619343, -18.72396509061168501, -26.88084378092850102 ) ) ;
#27027 = VECTOR ( 'NONE', #29326, 1000.000000000000000 ) ;
#27028 = CARTESIAN_POINT ( 'NONE',  ( 3.610593701936714695, 31.83882289796390097, 10.49999999999999645 ) ) ;
#27029 = ORIENTED_EDGE ( 'NONE', *, *, #169, .T. ) ;
#27030 = ORIENTED_EDGE ( 'NONE', *, *, #7889, .T. ) ;
#27031 = CARTESIAN_POINT ( 'NONE',  ( -7.145981593079294925, 19.42380627178312480, -27.86802767370806677 ) ) ;
#27032 = CARTESIAN_POINT ( 'NONE',  ( -5.767236651883567156, 13.71142893291686171, 10.00000000000000000 ) ) ;
#27033 = CARTESIAN_POINT ( 'NONE',  ( -12.09742388243079070, 14.36084852659847400, 10.49999999999999822 ) ) ;
#27034 = CARTESIAN_POINT ( 'NONE',  ( 5.440908595777815826, 35.94977745735560859, 9.500000000000000000 ) ) ;
#27035 = EDGE_LOOP ( 'NONE', ( #31687, #33397 ) ) ;
#27036 = CARTESIAN_POINT ( 'NONE',  ( 25.16949050179799841, 0.4568851818789111952, -17.44635195342746314 ) ) ;
#27037 = LINE ( 'NONE', #39420, #28413 ) ;
#27038 = CARTESIAN_POINT ( 'NONE',  ( -1.605702774688126722, 27.44183462127829642, 12.00000000000000000 ) ) ;
#27039 = CARTESIAN_POINT ( 'NONE',  ( -37.48481798130409004, -12.61800288157225580, 10.99999999999995381 ) ) ;
#27040 = ORIENTED_EDGE ( 'NONE', *, *, #20230, .T. ) ;
#27041 = CARTESIAN_POINT ( 'NONE',  ( -20.48147506303724441, 0.8713082578521279542, -30.00000000000000000 ) ) ;
#27042 = CARTESIAN_POINT ( 'NONE',  ( 15.02235689379175732, 21.92659494635341844, 10.50000000000000355 ) ) ;
#27043 = ADVANCED_FACE ( 'NONE', ( #35350 ), #26397, .T. ) ;
#27044 = ORIENTED_EDGE ( 'NONE', *, *, #8412, .F. ) ;
#27045 = CARTESIAN_POINT ( 'NONE',  ( 20.60546234692413847, -2.909310255760186870, -27.21192818574509786 ) ) ;
#27046 = CARTESIAN_POINT ( 'NONE',  ( 29.60586052328657303, -25.59238499873126216, 13.92931973827783843 ) ) ;
#27047 = EDGE_CURVE ( 'NONE', #3614, #29069, #4467, .T. ) ;
#27048 = EDGE_LOOP ( 'NONE', ( #28924, #2983, #24268, #26140 ) ) ;
#27049 = CARTESIAN_POINT ( 'NONE',  ( -13.38233516095408149, 33.85946688991404585, 13.92931973827825587 ) ) ;
#27050 = CARTESIAN_POINT ( 'NONE',  ( 12.15426487969635261, -15.33773963132624552, 20.99999999999999645 ) ) ;
#27051 = CARTESIAN_POINT ( 'NONE',  ( -35.84808252048276955, -3.038699442442200027, -5.000000000000005329 ) ) ;
#27052 = B_SPLINE_CURVE_WITH_KNOTS ( 'NONE', 3,
 ( #28419, #19080, #10138, #34126 ),
 .UNSPECIFIED., .F., .F.,
 ( 4, 4 ),
 ( 0.000000000000000000, 1.000000000000000000 ),
 .UNSPECIFIED. ) ;
#27053 = CARTESIAN_POINT ( 'NONE',  ( 7.962467718761615743, 24.71319220551615459, 20.69868183039781329 ) ) ;
#27054 = CIRCLE ( 'NONE', #9538, 1.000000000000000000 ) ;
#27055 = CIRCLE ( 'NONE', #7583, 1.000000000000000000 ) ;
#27056 = LINE ( 'NONE', #26851, #9664 ) ;
#27057 = EDGE_LOOP ( 'NONE', ( #27189, #36761, #6322, #8792 ) ) ;
#27058 = DIRECTION ( 'NONE',  ( -0.7431448254773862505, 0.6691306063588672304, -0.000000000000000000 ) ) ;
#27059 = LINE ( 'NONE', #30905, #20202 ) ;
#27060 = CARTESIAN_POINT ( 'NONE',  ( 7.011078276407629595, 36.06490844421831099, -8.006587430816212603 ) ) ;
#27061 = CARTESIAN_POINT ( 'NONE',  ( -14.36830325120615903, 20.48707633493503621, 7.000000000000000000 ) ) ;
#27062 = CARTESIAN_POINT ( 'NONE',  ( 11.85876577156197165, 19.91979463203424672, 19.99202127657068218 ) ) ;
#27063 = CARTESIAN_POINT ( 'NONE',  ( 18.66842418841368101, -27.23445290579710232, -5.917650609604824474 ) ) ;
#27064 = CARTESIAN_POINT ( 'NONE',  ( 12.44178368932927015, 35.65276919561884483, 10.99999999999994493 ) ) ;
#27065 = DIRECTION ( 'NONE',  ( 0.2079116908177532919, -0.9781476007338070211, -0.000000000000000000 ) ) ;
#27066 = CARTESIAN_POINT ( 'NONE',  ( 2.564829916171746937, 8.028556778314797526, 10.96580508970283141 ) ) ;
#27067 = ORIENTED_EDGE ( 'NONE', *, *, #10882, .T. ) ;
#27068 = CARTESIAN_POINT ( 'NONE',  ( 12.07661549505689536, 19.98892357814243681, -20.52991758538416889 ) ) ;
#27069 = EDGE_LOOP ( 'NONE', ( #24116, #11610, #21892 ) ) ;
#27070 = CARTESIAN_POINT ( 'NONE',  ( -11.90844352419377827, 18.06674963033532322, -23.91691853855833116 ) ) ;
#27071 = CARTESIAN_POINT ( 'NONE',  ( -31.37624276535950330, -18.11508220673910685, 18.42518152272108622 ) ) ;
#27072 = CARTESIAN_POINT ( 'NONE',  ( -14.41595319144209775, 26.31931657363132260, 10.49999999999999822 ) ) ;
#27073 = CARTESIAN_POINT ( 'NONE',  ( 11.25263760713990280, 17.70681266469984294, -26.23215722482760981 ) ) ;
#27074 = ORIENTED_EDGE ( 'NONE', *, *, #1313, .F. ) ;
#27075 = CARTESIAN_POINT ( 'NONE',  ( 17.72709310700289720, -10.48608855509684901, -28.44358586278453060 ) ) ;
#27076 = VERTEX_POINT ( 'NONE', #10972 ) ;
#27078 = CARTESIAN_POINT ( 'NONE',  ( -5.706342468480190000, 20.64589803375067945, 12.00000000000000000 ) ) ;
#27077 = CARTESIAN_POINT ( 'NONE',  ( -10.64042804724655689, 17.68140777639901984, -28.05361844119051540 ) ) ;
#27079 = CARTESIAN_POINT ( 'NONE',  ( -17.30319042518958383, -25.82435514465430515, -10.50227512508310923 ) ) ;
#27080 = DIRECTION ( 'NONE',  ( 0.000000000000000000, 0.000000000000000000, 1.000000000000000000 ) ) ;
#27081 = VECTOR ( 'NONE', #22626, 1000.000000000000000 ) ;
#27082 = VECTOR ( 'NONE', #34877, 1000.000000000000000 ) ;
#27083 = ORIENTED_EDGE ( 'NONE', *, *, #25415, .T. ) ;
#27084 = CARTESIAN_POINT ( 'NONE',  ( -20.53428788010907979, -7.794484820519511636, -24.29087954726551857 ) ) ;
#27085 = CARTESIAN_POINT ( 'NONE',  ( -9.394160329388485664, -18.36112709139673171, -28.08710526393325324 ) ) ;
#27086 = CARTESIAN_POINT ( 'NONE',  ( 23.05386822411317027, -7.747535282638454035, 23.00000000000000000 ) ) ;
#27087 = VERTEX_POINT ( 'NONE', #19298 ) ;
#27088 = CARTESIAN_POINT ( 'NONE',  ( 22.69882725526681710, 2.255467933073600051, -20.73643980054142943 ) ) ;
#27089 = DIRECTION ( 'NONE',  ( 0.4067366430758009299, 0.9135454576426005335, 0.000000000000000000 ) ) ;
#27090 = CARTESIAN_POINT ( 'NONE',  ( -14.42035624161473883, 26.65972665747678860, 11.00000000000000000 ) ) ;
#27091 = VECTOR ( 'NONE', #18212, 999.9999999999998863 ) ;
#27092 = EDGE_LOOP ( 'NONE', ( #27400, #17152, #15181, #32898 ) ) ;
#27093 = CARTESIAN_POINT ( 'NONE',  ( -25.91514792629616437, 0.2343253458700045866, -16.43276076001953356 ) ) ;
#27094 = VERTEX_POINT ( 'NONE', #28645 ) ;
#27095 = CARTESIAN_POINT ( 'NONE',  ( 25.57042713151565749, -0.2977480437168726346, -17.35121141349176455 ) ) ;
#27096 = CARTESIAN_POINT ( 'NONE',  ( 31.11751882148445603, -7.091474513517732170, 19.27171037444123414 ) ) ;
#27097 = ORIENTED_EDGE ( 'NONE', *, *, #26018, .F. ) ;
#27098 = CARTESIAN_POINT ( 'NONE',  ( -23.46629586039856363, 2.745952860400708406, -18.68457461683295762 ) ) ;
#27099 = CARTESIAN_POINT ( 'NONE',  ( -15.64741614794215252, 37.44040872933206288, 7.000000000000000000 ) ) ;
#27100 = CARTESIAN_POINT ( 'NONE',  ( 2.229431105722923245, 20.49260818092372460, 6.000000000000000000 ) ) ;
#27101 = CARTESIAN_POINT ( 'NONE',  ( 0.9999999999999991118, 36.00000000000000711, 10.00000000000000000 ) ) ;
#27102 = FACE_OUTER_BOUND ( 'NONE', #34546, .T. ) ;
#27103 = AXIS2_PLACEMENT_3D ( 'NONE', #20756, #8752, #39025 ) ;
#27104 = CIRCLE ( 'NONE', #32303, 1.000000000000000000 ) ;
#27105 = LINE ( 'NONE', #38897, #30081 ) ;
#27106 = CARTESIAN_POINT ( 'NONE',  ( -0.2474735156158440752, 16.63111439559750693, 6.000000000000000000 ) ) ;
#27107 = ORIENTED_EDGE ( 'NONE', *, *, #851, .F. ) ;
#27108 = CARTESIAN_POINT ( 'NONE',  ( -20.36783817944476027, 5.016842631823707599, -25.36215431227993022 ) ) ;
#27109 = CARTESIAN_POINT ( 'NONE',  ( 14.26584437371809777, 27.13525491562438319, 12.00000000000000000 ) ) ;
#27110 = LINE ( 'NONE', #15118, #12310 ) ;
#27111 = CARTESIAN_POINT ( 'NONE',  ( 16.13373544545436999, -15.79625797353112482, -23.17830139746911655 ) ) ;
#27112 = CIRCLE ( 'NONE', #25828, 1.000000000000000000 ) ;
#27113 = LINE ( 'NONE', #11477, #28090 ) ;
#27114 = DIRECTION ( 'NONE',  ( 1.000000000000000000, 0.000000000000000000, 0.000000000000000000 ) ) ;
#27115 = CARTESIAN_POINT ( 'NONE',  ( 12.11058524023762040, 20.85765977519871939, -19.43838798737532514 ) ) ;
#27116 = TOROIDAL_SURFACE ( 'NONE', #21257, 1.000000000000000000, 0.5000000000000000000 ) ;
#27117 = CARTESIAN_POINT ( 'NONE',  ( 4.238566308745586637E-14, -25.93120163663720845, 14.53008259254011136 ) ) ;
#27118 = ORIENTED_EDGE ( 'NONE', *, *, #2867, .F. ) ;
#27119 = CARTESIAN_POINT ( 'NONE',  ( -16.58187255403813509, 22.94673014519461773, -5.949379142203228277 ) ) ;
#27120 = CARTESIAN_POINT ( 'NONE',  ( -26.13185812888372794, -11.12779425996339988, 20.94377226548397886 ) ) ;
#27121 = ADVANCED_FACE ( 'NONE', ( #34746 ), #31696, .T. ) ;
#27122 = CARTESIAN_POINT ( 'NONE',  ( -14.26585111513660031, 17.86474508437623143, 13.00000000000000178 ) ) ;
#27123 = CARTESIAN_POINT ( 'NONE',  ( 11.70346012238788980, 18.89484313388442160, -22.73802100965551176 ) ) ;
#27124 = ORIENTED_EDGE ( 'NONE', *, *, #17381, .T. ) ;
#27125 = CARTESIAN_POINT ( 'NONE',  ( -14.56494338438164071, 21.47191690367856864, 10.99387789255782799 ) ) ;
#27126 = VERTEX_POINT ( 'NONE', #19498 ) ;
#27128 = CARTESIAN_POINT ( 'NONE',  ( 5.440908595777814050, 35.94977745735560859, 7.000000000000000000 ) ) ;
#27127 = CARTESIAN_POINT ( 'NONE',  ( -15.30745419785728778, 26.89740918011089121, -6.413591019650938918 ) ) ;
#27129 = CARTESIAN_POINT ( 'NONE',  ( -10.89308438657891465, -19.97759514595176356, -21.60980701075553867 ) ) ;
#27130 = CARTESIAN_POINT ( 'NONE',  ( -16.87498849720607552, -29.16588574430774017, 10.99999999999931433 ) ) ;
#27131 = CARTESIAN_POINT ( 'NONE',  ( -20.35163850574221556, -12.28510868635483000, -21.83632322477828680 ) ) ;
#27132 = CARTESIAN_POINT ( 'NONE',  ( -7.667318022502500163, -19.44231725057151294, -26.40555248174693048 ) ) ;
#27133 = CARTESIAN_POINT ( 'NONE',  ( -24.22138565352712902, -9.557272464391486366, 20.99999999999999289 ) ) ;
#27134 = CARTESIAN_POINT ( 'NONE',  ( 11.91108122330540375, 16.91021841892633049, -27.50939510565961044 ) ) ;
#27135 = EDGE_CURVE ( 'NONE', #12781, #10973, #3216, .T. ) ;
#27136 = ORIENTED_EDGE ( 'NONE', *, *, #9432, .T. ) ;
#27137 = CARTESIAN_POINT ( 'NONE',  ( 23.59500296165097666, 6.292542308228194159, -13.80885738943037389 ) ) ;
#27138 = DIRECTION ( 'NONE',  ( -0.000000000000000000, -0.000000000000000000, -1.000000000000000000 ) ) ;
#27139 = DIRECTION ( 'NONE',  ( 1.000000000000000000, 0.000000000000000000, 0.000000000000000000 ) ) ;
#27140 = ADVANCED_FACE ( 'NONE', ( #10362 ), #22741, .F. ) ;
#27141 = CARTESIAN_POINT ( 'NONE',  ( 15.02235689379175732, 21.92659494635341844, 10.50000000000000000 ) ) ;
#27142 = ORIENTED_EDGE ( 'NONE', *, *, #29777, .F. ) ;
#27143 = CARTESIAN_POINT ( 'NONE',  ( -30.31125568725408570, -1.084487226365530743, -10.56604182229928135 ) ) ;
#27145 = CARTESIAN_POINT ( 'NONE',  ( 26.60678562830161553, 0.1240764605644925633, -15.43182042406326815 ) ) ;
#27144 = VECTOR ( 'NONE', #9104, 1000.000000000000000 ) ;
#27146 = CIRCLE ( 'NONE', #10936, 1.000000000000004441 ) ;
#27147 = PLANE ( 'NONE',  #31284 ) ;
#27148 = CARTESIAN_POINT ( 'NONE',  ( 21.14791330573125805, -16.83114732581536899, 21.00000000000004619 ) ) ;
#27149 = CARTESIAN_POINT ( 'NONE',  ( 23.06249103411542478, 13.31513540672987972, -4.999999999999992006 ) ) ;
#27151 = CIRCLE ( 'NONE', #32995, 1.000000000000000000 ) ;
#27150 = CARTESIAN_POINT ( 'NONE',  ( 8.339609403135803234, 11.87216320208440123, 10.00000000000000000 ) ) ;
#27152 = EDGE_CURVE ( 'NONE', #1450, #32508, #1273, .T. ) ;
#27153 = ORIENTED_EDGE ( 'NONE', *, *, #21533, .T. ) ;
#27154 = ADVANCED_FACE ( 'NONE', ( #29046 ), #1421, .T. ) ;
#27155 = FACE_OUTER_BOUND ( 'NONE', #15058, .T. ) ;
#27156 = CARTESIAN_POINT ( 'NONE',  ( 5.953805871968278929, 30.22298757065274444, 12.00000000000000000 ) ) ;
#27157 = ORIENTED_EDGE ( 'NONE', *, *, #16970, .T. ) ;
#27158 = CARTESIAN_POINT ( 'NONE',  ( 0.2195541181463148694, 20.74688730825959837, -27.70547263837515217 ) ) ;
#27159 = CARTESIAN_POINT ( 'NONE',  ( -14.31603901957233838, 19.98981538725089990, 11.00000000000000000 ) ) ;
#27160 = CARTESIAN_POINT ( 'NONE',  ( 13.22866120778972387, 26.17694675929307735, 18.42518152272108978 ) ) ;
#27161 = FACE_OUTER_BOUND ( 'NONE', #24341, .T. ) ;
#27162 = DIRECTION ( 'NONE',  ( 1.000000000000000000, 0.000000000000000000, 0.000000000000000000 ) ) ;
#27163 = DIRECTION ( 'NONE',  ( -0.000000000000000000, -0.000000000000000000, -1.000000000000000000 ) ) ;
#27164 = CARTESIAN_POINT ( 'NONE',  ( -4.881458130668121953, -28.77689918168226413, 22.99999999999999645 ) ) ;
#27165 = AXIS2_PLACEMENT_3D ( 'NONE', #9804, #13039, #34585 ) ;
#27166 = CARTESIAN_POINT ( 'NONE',  ( 13.53295666386236995, 26.20769765665461648, -12.41112605713692396 ) ) ;
#27167 = DIRECTION ( 'NONE',  ( 0.4731467892558273158, 0.5254827454987467394, -0.7071067811865482389 ) ) ;
#27168 = AXIS2_PLACEMENT_3D ( 'NONE', #18545, #8805, #33597 ) ;
#27169 = ORIENTED_EDGE ( 'NONE', *, *, #31962, .T. ) ;
#27171 = DIRECTION ( 'NONE',  ( 1.000000000000000000, 0.000000000000000000, 0.000000000000000000 ) ) ;
#27170 = CARTESIAN_POINT ( 'NONE',  ( -16.62029253314668864, 12.60395031145305289, -25.48503712365854312 ) ) ;
#27172 = CARTESIAN_POINT ( 'NONE',  ( 0.000000000000000000, 22.50000000000000355, 7.000000000000000000 ) ) ;
#27173 = CARTESIAN_POINT ( 'NONE',  ( 12.29527272661349713, -22.02268596340331186, -17.43674506788135048 ) ) ;
#27174 = DIRECTION ( 'NONE',  ( -0.000000000000000000, -0.000000000000000000, -1.000000000000000000 ) ) ;
#27175 = CARTESIAN_POINT ( 'NONE',  ( 13.75279816399555877, 23.43377685412391287, -14.47231226931382864 ) ) ;
#27176 = AXIS2_PLACEMENT_3D ( 'NONE', #17525, #8766, #12010 ) ;
#27177 = ORIENTED_EDGE ( 'NONE', *, *, #4151, .T. ) ;
#27178 = FACE_OUTER_BOUND ( 'NONE', #37429, .T. ) ;
#27179 = EDGE_CURVE ( 'NONE', #9314, #7162, #23559, .T. ) ;
#27180 = DIRECTION ( 'NONE',  ( -1.224646799147351235E-16, 1.000000000000000000, 0.000000000000000000 ) ) ;
#27181 = CARTESIAN_POINT ( 'NONE',  ( -17.92780664361741927, -14.00736870931739375, -23.04536792413068724 ) ) ;
#27182 = CARTESIAN_POINT ( 'NONE',  ( 4.025418116673052715, -24.86707171575129038, -5.481476286668475417 ) ) ;
#27183 = CARTESIAN_POINT ( 'NONE',  ( 15.58410715161808824, 26.18909738223269557, -5.474078854422544715 ) ) ;
#27184 = CARTESIAN_POINT ( 'NONE',  ( 18.48238482655413861, 11.30487917964827105, -21.18117017502385480 ) ) ;
#27185 = CARTESIAN_POINT ( 'NONE',  ( -15.26585111513660209, 17.86474508437623143, 6.000000000000000000 ) ) ;
#27186 = CARTESIAN_POINT ( 'NONE',  ( -4.180913945065587889, 37.58733905612867687, -7.125526861301994863 ) ) ;
#27187 = ORIENTED_EDGE ( 'NONE', *, *, #25093, .F. ) ;
#27188 = CARTESIAN_POINT ( 'NONE',  ( -28.53381226739762511, 4.748233269558084224, 13.32518128617320130 ) ) ;
#27189 = ORIENTED_EDGE ( 'NONE', *, *, #1972, .F. ) ;
#27190 = CARTESIAN_POINT ( 'NONE',  ( 4.524139159579308789, 31.43208625488810171, 10.49999999999999645 ) ) ;
#27191 = CARTESIAN_POINT ( 'NONE',  ( 9.204968164644647288, 10.68109904802224541, 10.68306085400111982 ) ) ;
#27192 = CARTESIAN_POINT ( 'NONE',  ( -20.60009190789856959, 1.015461553205563083, -28.08564569100201780 ) ) ;
#27193 = CARTESIAN_POINT ( 'NONE',  ( 19.80298806677364709, -5.334938486795024026, -29.99999999999998579 ) ) ;
#27194 = VECTOR ( 'NONE', #4728, 1000.000000000000114 ) ;
#27195 = AXIS2_PLACEMENT_3D ( 'NONE', #2774, #14571, #24110 ) ;
#27196 = ORIENTED_EDGE ( 'NONE', *, *, #38570, .F. ) ;
#27197 = EDGE_CURVE ( 'NONE', #26812, #16537, #38244, .T. ) ;
#27198 = DIRECTION ( 'NONE',  ( 0.8660254037844363761, -0.5000000000000038858, 0.000000000000000000 ) ) ;
#27199 = ORIENTED_EDGE ( 'NONE', *, *, #14758, .T. ) ;
#27200 = EDGE_CURVE ( 'NONE', #6928, #37263, #34364, .T. ) ;
#27201 = AXIS2_PLACEMENT_3D ( 'NONE', #16260, #37991, #4056 ) ;
#27202 = CYLINDRICAL_SURFACE ( 'NONE', #2212, 0.5000000000000004441 ) ;
#27203 = DIRECTION ( 'NONE',  ( -1.000000000000000000, 0.000000000000000000, 0.000000000000000000 ) ) ;
#27204 = CARTESIAN_POINT ( 'NONE',  ( 10.47804177580207607, 33.28010392086025604, 10.49999999999999645 ) ) ;
#27205 = ORIENTED_EDGE ( 'NONE', *, *, #4478, .F. ) ;
#27206 = LINE ( 'NONE', #18271, #33460 ) ;
#27207 = CARTESIAN_POINT ( 'NONE',  ( 10.47804177580207607, 33.28010392086025604, 10.50000000000000000 ) ) ;
#27208 = DIRECTION ( 'NONE',  ( -0.000000000000000000, -0.000000000000000000, -1.000000000000000000 ) ) ;
#27209 = CARTESIAN_POINT ( 'NONE',  ( 29.55170335801485493, -22.74801049114014972, -7.986860386523519928 ) ) ;
#27210 = CARTESIAN_POINT ( 'NONE',  ( 17.32108554687955149, 13.66007284228603602, -20.07984646109152038 ) ) ;
#27211 = CARTESIAN_POINT ( 'NONE',  ( 9.198933924422197705, 23.73018153482928128, -19.01023341765094798 ) ) ;
#27212 = ORIENTED_EDGE ( 'NONE', *, *, #21507, .T. ) ;
#27213 = CARTESIAN_POINT ( 'NONE',  ( -19.43993472154038216, 9.610213393078213429, -21.17343657839546722 ) ) ;
#27214 = CARTESIAN_POINT ( 'NONE',  ( -9.294006203984645609, 33.46401007850805343, 12.00000000000000000 ) ) ;
#27215 = DIRECTION ( 'NONE',  ( 1.000000000000000000, 0.000000000000000000, 0.000000000000000000 ) ) ;
#27216 = CARTESIAN_POINT ( 'NONE',  ( 15.22921972075588748, -26.04634760375180491, -9.226272813048730370 ) ) ;
#27217 = B_SPLINE_CURVE_WITH_KNOTS ( 'NONE', 3,
 ( #28026, #15639, #30881, #15437 ),
 .UNSPECIFIED., .F., .F.,
 ( 4, 4 ),
 ( 0.000000000000000000, 1.000000000000000000 ),
 .UNSPECIFIED. ) ;
#27218 = DIRECTION ( 'NONE',  ( 0.000000000000000000, 0.000000000000000000, 1.000000000000000000 ) ) ;
#27219 = CARTESIAN_POINT ( 'NONE',  ( 17.34253826539385201, 27.32041144647958575, -13.70816084473008800 ) ) ;
#27220 = EDGE_CURVE ( 'NONE', #7663, #5398, #39193, .T. ) ;
#27222 = AXIS2_PLACEMENT_3D ( 'NONE', #23054, #7611, #1527 ) ;
#27221 = CARTESIAN_POINT ( 'NONE',  ( -15.35818044939771632, 26.72156206222938124, -6.416418653425738583 ) ) ;
#27223 = CARTESIAN_POINT ( 'NONE',  ( -20.50183232903691177, -24.38735400865616754, -12.17096377724693035 ) ) ;
#27224 = CARTESIAN_POINT ( 'NONE',  ( 14.14567267149670293, -26.22303375651868151, -7.362319143684429079 ) ) ;
#27225 = ADVANCED_FACE ( 'NONE', ( #36547 ), #24151, .T. ) ;
#27226 = DIRECTION ( 'NONE',  ( -0.9781476007338069101, -0.2079116908177533751, 0.000000000000000000 ) ) ;
#27227 = ORIENTED_EDGE ( 'NONE', *, *, #32488, .T. ) ;
#27228 = EDGE_LOOP ( 'NONE', ( #17598, #38593, #27711, #20307 ) ) ;
#27229 = CARTESIAN_POINT ( 'NONE',  ( -10.84359833522533023, 29.92721541907581084, -12.17318395035172074 ) ) ;
#27230 = CARTESIAN_POINT ( 'NONE',  ( -6.688306800005769048, 28.52217545723006609, 6.000000000000000000 ) ) ;
#27231 = LINE ( 'NONE', #18099, #21110 ) ;
#27232 = CARTESIAN_POINT ( 'NONE',  ( -5.237540274239744775, 35.49300472853438038, 7.500000000000000888 ) ) ;
#27233 = VERTEX_POINT ( 'NONE', #4864 ) ;
#27234 = CARTESIAN_POINT ( 'NONE',  ( 20.60758928576245452, 0.8974886860145109280, -28.07985037303415510 ) ) ;
#27235 = DIRECTION ( 'NONE',  ( -0.000000000000000000, -0.000000000000000000, -1.000000000000000000 ) ) ;
#27236 = CARTESIAN_POINT ( 'NONE',  ( 0.000000000000000000, 22.50000000000000355, 7.000000000000000000 ) ) ;
#27237 = VERTEX_POINT ( 'NONE', #14412 ) ;
#27238 = CARTESIAN_POINT ( 'NONE',  ( -28.88209946128927896, 0.1111908453527043067, -11.59938499466097817 ) ) ;
#27239 = CARTESIAN_POINT ( 'NONE',  ( 7.935770203493858865, 22.34671014717335780, 12.00000000000000000 ) ) ;
#27240 = VERTEX_POINT ( 'NONE', #17277 ) ;
#27241 = CARTESIAN_POINT ( 'NONE',  ( 22.75668780360189203, -3.280807789042111899, -22.27935141650941375 ) ) ;
#27242 = CARTESIAN_POINT ( 'NONE',  ( 37.03605016780974069, -10.92602907108481958, 13.92931973827803738 ) ) ;
#27243 = ORIENTED_EDGE ( 'NONE', *, *, #4886, .T. ) ;
#27244 = CARTESIAN_POINT ( 'NONE',  ( -11.65184672540978639, 34.81748849094240228, 15.13084544680287813 ) ) ;
#27245 = CARTESIAN_POINT ( 'NONE',  ( 5.799013854623458641, -17.87737810982027398, 20.50957957746029336 ) ) ;
#27246 = EDGE_CURVE ( 'NONE', #30103, #32913, #11764, .T. ) ;
#27247 = DIRECTION ( 'NONE',  ( 1.000000000000000000, 0.000000000000000000, 0.000000000000000000 ) ) ;
#27248 = EDGE_CURVE ( 'NONE', #17958, #14918, #14210, .T. ) ;
#27249 = CARTESIAN_POINT ( 'NONE',  ( 6.855490822441819176, 29.74656830693212939, 20.25080042701566896 ) ) ;
#27250 = VECTOR ( 'NONE', #39205, 1000.000000000000114 ) ;
#27251 = DIRECTION ( 'NONE',  ( -0.000000000000000000, -0.000000000000000000, -1.000000000000000000 ) ) ;
#27252 = ORIENTED_EDGE ( 'NONE', *, *, #33333, .T. ) ;
#27253 = CARTESIAN_POINT ( 'NONE',  ( -17.28285333400955182, 27.30382183500235627, 12.14047268033097815 ) ) ;
#27254 = CARTESIAN_POINT ( 'NONE',  ( 13.86830325120613594, 20.48707633493483371, 7.500000000000010658 ) ) ;
#27255 = CIRCLE ( 'NONE', #24670, 15.00000000000000000 ) ;
#27256 = CARTESIAN_POINT ( 'NONE',  ( 7.928258658476393883, 35.05882616698742282, -8.896045816660139494 ) ) ;
#27257 = DIRECTION ( 'NONE',  ( -0.000000000000000000, -0.000000000000000000, -1.000000000000000000 ) ) ;
#27258 = CARTESIAN_POINT ( 'NONE',  ( 25.38348611796501686, -5.460896781496693997, 20.69868183039781329 ) ) ;
#27259 = CARTESIAN_POINT ( 'NONE',  ( 19.27831178257280698, -25.27455051888069804, -11.31654119470542064 ) ) ;
#27260 = CARTESIAN_POINT ( 'NONE',  ( -7.591957726968679765, 38.93640765974109996, 10.99999999999981348 ) ) ;
#27261 = B_SPLINE_CURVE_WITH_KNOTS ( 'NONE', 3,
 ( #34159, #31700, #6111, #37002, #21955, #822 ),
 .UNSPECIFIED., .F., .F.,
 ( 4, 2, 4 ),
 ( 0.000000000000000000, 0.5000000000000000000, 1.000000000000000000 ),
 .UNSPECIFIED. ) ;
#27262 = CARTESIAN_POINT ( 'NONE',  ( -12.88757880222275887, 15.63670317852396074, 10.99387789255782266 ) ) ;
#27263 = CARTESIAN_POINT ( 'NONE',  ( 10.10646936306337729, 32.94553861768082470, 10.49999999999999645 ) ) ;
#27264 = ORIENTED_EDGE ( 'NONE', *, *, #23441, .F. ) ;
#27265 = EDGE_CURVE ( 'NONE', #34434, #1614, #32404, .T. ) ;
#27266 = CARTESIAN_POINT ( 'NONE',  ( 11.63972795867577936, 18.95610267478247479, -22.72707233481362721 ) ) ;
#27267 = VERTEX_POINT ( 'NONE', #8718 ) ;
#27268 = CARTESIAN_POINT ( 'NONE',  ( -15.59869368156687486, 26.13660472685725722, -5.474064220111173995 ) ) ;
#27269 = AXIS2_PLACEMENT_3D ( 'NONE', #34946, #10763, #4861 ) ;
#27270 = CARTESIAN_POINT ( 'NONE',  ( -21.96133346275663456, -24.83662088761592202, 18.42518152272072740 ) ) ;
#27271 = CARTESIAN_POINT ( 'NONE',  ( 14.80295835475978627, -25.81819152709282505, -9.710063844406016997 ) ) ;
#27272 = ADVANCED_FACE ( 'NONE', ( #18071 ), #11570, .T. ) ;
#27273 = CARTESIAN_POINT ( 'NONE',  ( 4.003810537522394242, 8.420815593655317954, 10.49999999999999822 ) ) ;
#27274 = CARTESIAN_POINT ( 'NONE',  ( 11.16022610508474067, 17.44351855606713642, -27.45452920518326678 ) ) ;
#27275 = VERTEX_POINT ( 'NONE', #23754 ) ;
#27276 = CARTESIAN_POINT ( 'NONE',  ( 30.53904149796068879, -19.36372090394836931, -10.17381678346307972 ) ) ;
#27277 = ORIENTED_EDGE ( 'NONE', *, *, #33229, .T. ) ;
#27279 = CARTESIAN_POINT ( 'NONE',  ( 7.741055489194820893, 10.14404956260389667, 10.49999999999999822 ) ) ;
#27278 = CARTESIAN_POINT ( 'NONE',  ( -10.92505544481902469, 18.33161101182201236, -24.96188984657137055 ) ) ;
#27280 = CARTESIAN_POINT ( 'NONE',  ( -15.65190729232149280, -24.80065730001655666, -12.43069847511498338 ) ) ;
#27281 = CARTESIAN_POINT ( 'NONE',  ( 11.39463915635820612, 18.33192650902018883, 6.000000000000000000 ) ) ;
#27282 = ORIENTED_EDGE ( 'NONE', *, *, #28529, .T. ) ;
#27283 = EDGE_CURVE ( 'NONE', #25293, #27469, #32111, .T. ) ;
#27284 = CARTESIAN_POINT ( 'NONE',  ( -34.95683723113188535, -12.02710497262000366, -7.574730441631502664 ) ) ;
#27285 = CARTESIAN_POINT ( 'NONE',  ( -9.435257979599080969, -18.55952215190476551, -26.85164704141170589 ) ) ;
#27286 = DIRECTION ( 'NONE',  ( 0.000000000000000000, 0.000000000000000000, 1.000000000000000000 ) ) ;
#27287 = EDGE_LOOP ( 'NONE', ( #25060, #507, #24037, #35011 ) ) ;
#27288 = CARTESIAN_POINT ( 'NONE',  ( 29.53226466533872596, 1.120089121006105692, -7.363481725902196295 ) ) ;
#27289 = CYLINDRICAL_SURFACE ( 'NONE', #29074, 1.000000000000000888 ) ;
#27290 = CYLINDRICAL_SURFACE ( 'NONE', #36158, 1.000000000000000000 ) ;
#27291 = AXIS2_PLACEMENT_3D ( 'NONE', #1985, #20671, #33068 ) ;
#27292 = ORIENTED_EDGE ( 'NONE', *, *, #3618, .T. ) ;
#27293 = CARTESIAN_POINT ( 'NONE',  ( -30.91306671499135916, -0.08701806214385847393, -5.945400134279025472 ) ) ;
#27294 = VERTEX_POINT ( 'NONE', #36151 ) ;
#27295 = CARTESIAN_POINT ( 'NONE',  ( 31.33932419087585330, -1.338176013559867261, -8.697177606183496223 ) ) ;
#27296 = CARTESIAN_POINT ( 'NONE',  ( 33.92416433109537621, -10.98373637526195168, 17.92354375535250455 ) ) ;
#27297 = ORIENTED_EDGE ( 'NONE', *, *, #24492, .T. ) ;
#27298 = CARTESIAN_POINT ( 'NONE',  ( -25.48877880442670474, 2.684454445128169997, -14.63412680931335430 ) ) ;
#27299 = EDGE_CURVE ( 'NONE', #21130, #8575, #21400, .T. ) ;
#27300 = CARTESIAN_POINT ( 'NONE',  ( -10.72918489117944674, 32.98258515686310943, 7.500000000000004441 ) ) ;
#27301 = EDGE_CURVE ( 'NONE', #28965, #25600, #7114, .T. ) ;
#27302 = CYLINDRICAL_SURFACE ( 'NONE', #36232, 60.00000000000007105 ) ;
#27303 = CARTESIAN_POINT ( 'NONE',  ( 0.000000000000000000, 0.000000000000000000, 7.000000000000000000 ) ) ;
#27304 = CARTESIAN_POINT ( 'NONE',  ( 15.26584437371809955, 27.13525491562438319, 13.00000000000000178 ) ) ;
#27305 = FACE_BOUND ( 'NONE', #1213, .T. ) ;
#27306 = DIRECTION ( 'NONE',  ( -0.8660254037844364872, 0.5000000000000038858, -0.000000000000000000 ) ) ;
#27307 = ORIENTED_EDGE ( 'NONE', *, *, #20330, .T. ) ;
#27308 = CARTESIAN_POINT ( 'NONE',  ( -25.27117276387230760, 5.256176016299023424, -10.79590797945013492 ) ) ;
#27309 = DIRECTION ( 'NONE',  ( 0.000000000000000000, 0.000000000000000000, 1.000000000000000000 ) ) ;
#27310 = CARTESIAN_POINT ( 'NONE',  ( 0.000000000000000000, 22.50000000000000355, 0.000000000000000000 ) ) ;
#27311 = CARTESIAN_POINT ( 'NONE',  ( 15.13892795146889192, -13.95385527665263403, -28.49116766414493185 ) ) ;
#27312 = FACE_OUTER_BOUND ( 'NONE', #14704, .T. ) ;
#27313 = CARTESIAN_POINT ( 'NONE',  ( 10.83909553179808860, 18.00096194490589951, -26.18758634457435264 ) ) ;
#27314 = CARTESIAN_POINT ( 'NONE',  ( 5.146739273647275681, -25.63390596715193936, 15.13084544680213739 ) ) ;
#27315 = ORIENTED_EDGE ( 'NONE', *, *, #1203, .T. ) ;
#27316 = CARTESIAN_POINT ( 'NONE',  ( -13.42818987338513459, 17.16911081534734862, -22.99155224325752300 ) ) ;
#27317 = CARTESIAN_POINT ( 'NONE',  ( -25.43307211745671736, -8.368469763667990335, 20.94377226548378346 ) ) ;
#27318 = EDGE_CURVE ( 'NONE', #28310, #37355, #17679, .T. ) ;
#27319 = CYLINDRICAL_SURFACE ( 'NONE', #39312, 0.4999999999999995559 ) ;
#27320 = CARTESIAN_POINT ( 'NONE',  ( 15.43121851897235786, 26.72868093004962020, -4.999999999999998224 ) ) ;
#27321 = EDGE_LOOP ( 'NONE', ( #2349, #23277, #36279, #35234, #31575 ) ) ;
#27322 = DIRECTION ( 'NONE',  ( -0.8090169943749510040, -0.5877852522924683631, 0.000000000000000000 ) ) ;
#27323 = EDGE_LOOP ( 'NONE', ( #3546, #25713, #30523 ) ) ;
#27325 = CARTESIAN_POINT ( 'NONE',  ( -37.48557158514997667, -11.24999999999982414, 3.000000000000000000 ) ) ;
#27324 = CARTESIAN_POINT ( 'NONE',  ( -13.95668707828244059, 24.11263528183340554, -13.49652051132212094 ) ) ;
#27326 = CARTESIAN_POINT ( 'NONE',  ( -14.07101309938052403, -24.61591519948004603, -12.54868197112087103 ) ) ;
#27327 = CARTESIAN_POINT ( 'NONE',  ( -9.343266739736648674, 17.68301270189230578, 10.00000000000000000 ) ) ;
#27328 = AXIS2_PLACEMENT_3D ( 'NONE', #1472, #7351, #17125 ) ;
#27329 = CARTESIAN_POINT ( 'NONE',  ( -29.19019149203798591, -16.43308044909656829, -12.88835385468937744 ) ) ;
#27330 = CARTESIAN_POINT ( 'NONE',  ( -9.622411929345382475, -22.55102273573495353, -16.66494747511510610 ) ) ;
#27331 = FACE_OUTER_BOUND ( 'NONE', #19677, .T. ) ;
#27332 = CARTESIAN_POINT ( 'NONE',  ( 15.09791029636327764, 22.51266978359509707, -12.62702112920867847 ) ) ;
#27333 = ORIENTED_EDGE ( 'NONE', *, *, #17421, .F. ) ;
#27334 = CARTESIAN_POINT ( 'NONE',  ( 24.22245084703565610, 6.361410862367799623, -11.80793526373495261 ) ) ;
#27335 = AXIS2_PLACEMENT_3D ( 'NONE', #8158, #39237, #20564 ) ;
#27336 = CARTESIAN_POINT ( 'NONE',  ( -8.806982162272252168, 13.84996144622306247, 6.000000000000000000 ) ) ;
#27337 = DIRECTION ( 'NONE',  ( 1.000000000000000000, 0.000000000000000000, 0.000000000000000000 ) ) ;
#27338 = DIRECTION ( 'NONE',  ( 1.000000000000000000, 0.000000000000000000, 0.000000000000000000 ) ) ;
#27339 = EDGE_LOOP ( 'NONE', ( #26665, #23089, #22433, #26384 ) ) ;
#27340 = CARTESIAN_POINT ( 'NONE',  ( -24.47322330375783039, -0.9128233859311521980, -19.31502028455822639 ) ) ;
#27341 = CARTESIAN_POINT ( 'NONE',  ( 27.86069736982781464, 0.03076757672864667559, -13.49648488625461340 ) ) ;
#27342 = DIRECTION ( 'NONE',  ( -1.000000000000000000, 0.000000000000000000, 0.000000000000000000 ) ) ;
#27343 = CARTESIAN_POINT ( 'NONE',  ( 26.67038870798830885, -5.578326634889591240, 20.50957957746141958 ) ) ;
#27344 = CARTESIAN_POINT ( 'NONE',  ( 21.88499642459564143, -5.528038495964486820, -20.11584339644707597 ) ) ;
#27345 = DIRECTION ( 'NONE',  ( -0.6123724356957974679, 0.3535533905932733978, -0.7071067811865451302 ) ) ;
#27346 = ORIENTED_EDGE ( 'NONE', *, *, #4387, .F. ) ;
#27347 = ADVANCED_FACE ( 'NONE', ( #30257 ), #5068, .F. ) ;
#27348 = DIRECTION ( 'NONE',  ( -0.9135454576426059736, -0.4067366430757888285, 0.000000000000000000 ) ) ;
#27349 = AXIS2_PLACEMENT_3D ( 'NONE', #13807, #25800, #38197 ) ;
#27350 = DIRECTION ( 'NONE',  ( -0.000000000000000000, -0.000000000000000000, -1.000000000000000000 ) ) ;
#27351 = CARTESIAN_POINT ( 'NONE',  ( 33.62187204924162387, 0.04418559750794539415, -5.000000000000002665 ) ) ;
#27352 = CARTESIAN_POINT ( 'NONE',  ( 3.669446457248423332, 35.72068143852440869, -10.18510980848603253 ) ) ;
#27353 = AXIS2_PLACEMENT_3D ( 'NONE', #17275, #4665, #38588 ) ;
#27354 = PLANE ( 'NONE',  #11370 ) ;
#27355 = CARTESIAN_POINT ( 'NONE',  ( 15.87271491999988804, 26.91186955879557985, 15.72805884748939143 ) ) ;
#27356 = EDGE_CURVE ( 'NONE', #3290, #26362, #11026, .T. ) ;
#27357 = DIRECTION ( 'NONE',  ( -0.000000000000000000, -0.000000000000000000, 1.000000000000000000 ) ) ;
#27358 = CARTESIAN_POINT ( 'NONE',  ( -3.211402178667006169, 32.38366924255629442, 13.00000000000000178 ) ) ;
#27359 = DIRECTION ( 'NONE',  ( -0.000000000000000000, -0.000000000000000000, 1.000000000000000000 ) ) ;
#27360 = LINE ( 'NONE', #18226, #21644 ) ;
#27361 = CARTESIAN_POINT ( 'NONE',  ( 14.82527878907322538, 28.13924469978218923, -6.856551512622178990 ) ) ;
#27362 = CARTESIAN_POINT ( 'NONE',  ( 13.42604558747167864, 21.08886574588663620, 7.000000000000000000 ) ) ;
#27363 = ORIENTED_EDGE ( 'NONE', *, *, #4272, .T. ) ;
#27365 = FACE_OUTER_BOUND ( 'NONE', #29688, .T. ) ;
#27364 = CARTESIAN_POINT ( 'NONE',  ( -16.15483981359775001, 13.22461535667768473, -25.46561888468577806 ) ) ;
#27366 = CARTESIAN_POINT ( 'NONE',  ( -13.81505241748936541, 27.51451374705156638, 10.96580508970282253 ) ) ;
#27367 = CARTESIAN_POINT ( 'NONE',  ( 15.42709217669442090, -26.65236356593726796, -6.416988218343957939 ) ) ;
#27368 = CARTESIAN_POINT ( 'NONE',  ( -21.08265500991413788, -26.45952537750927291, -8.564919882568894138 ) ) ;
#27369 = CARTESIAN_POINT ( 'NONE',  ( 23.05386822411318803, -7.747535282638377652, 20.99999999999999645 ) ) ;
#27370 = CARTESIAN_POINT ( 'NONE',  ( 15.40434907611582638, 26.82505288294843027, -4.999999999999998224 ) ) ;
#27371 = VERTEX_POINT ( 'NONE', #39591 ) ;
#27372 = DIRECTION ( 'NONE',  ( 0.000000000000000000, 0.000000000000000000, 1.000000000000000000 ) ) ;
#27373 = DIRECTION ( 'NONE',  ( 0.000000000000000000, 0.000000000000000000, 1.000000000000000000 ) ) ;
#27374 = CARTESIAN_POINT ( 'NONE',  ( -16.86820373146711205, -13.17562041779036441, -25.62346928861798290 ) ) ;
#27375 = CARTESIAN_POINT ( 'NONE',  ( -0.3862909676465622333, -24.66147537587169225, -7.427960836158034930 ) ) ;
#27376 = CARTESIAN_POINT ( 'NONE',  ( 15.50752910295250864, 26.03341394949190857, -6.889194152022838580 ) ) ;
#27377 = CARTESIAN_POINT ( 'NONE',  ( 21.38745727808766617, 11.90858952770566503, -8.901519087829083077 ) ) ;
#27378 = DIRECTION ( 'NONE',  ( 1.000000000000000000, 0.000000000000000000, 0.000000000000000000 ) ) ;
#27379 = ADVANCED_FACE ( 'NONE', ( #37346 ), #9319, .T. ) ;
#27380 = CARTESIAN_POINT ( 'NONE',  ( -3.058361328855125905, 21.76692312865797518, -24.27252685025706924 ) ) ;
#27381 = ORIENTED_EDGE ( 'NONE', *, *, #36702, .F. ) ;
#27382 = CARTESIAN_POINT ( 'NONE',  ( -30.62108498763855380, -5.687012903234330174, -13.09446411654519160 ) ) ;
#27383 = CARTESIAN_POINT ( 'NONE',  ( -20.33644687577595178, 12.50987689638972356, 7.499999999999997335 ) ) ;
#27384 = VERTEX_POINT ( 'NONE', #6455 ) ;
#27385 = DIRECTION ( 'NONE',  ( 0.9781476007338041345, -0.2079116908177664202, 0.000000000000000000 ) ) ;
#27386 = CARTESIAN_POINT ( 'NONE',  ( -8.118377661053488126, 10.47536095541708967, 7.500000000000000888 ) ) ;
#27387 = B_SPLINE_CURVE_WITH_KNOTS ( 'NONE', 3,
 ( #36608, #30915, #34363, #2680, #2879, #24613 ),
 .UNSPECIFIED., .F., .F.,
 ( 4, 2, 4 ),
 ( 0.000000000000000000, 0.5000000000000000000, 1.000000000000000000 ),
 .UNSPECIFIED. ) ;
#27388 = CARTESIAN_POINT ( 'NONE',  ( -30.06895585930082149, 0.4279890562384842112, -7.831005020092066893 ) ) ;
#27389 = CARTESIAN_POINT ( 'NONE',  ( 21.31962645927955435, -7.874799234479001875, -23.07151141173847364 ) ) ;
#27390 = ADVANCED_FACE ( 'NONE', ( #18268 ), #18817, .T. ) ;
#27391 = ORIENTED_EDGE ( 'NONE', *, *, #15617, .F. ) ;
#27392 = AXIS2_PLACEMENT_3D ( 'NONE', #22930, #26179, #32495 ) ;
#27393 = DIRECTION ( 'NONE',  ( 0.8090169943749503378, 0.5877852522924691403, 0.000000000000000000 ) ) ;
#27394 = EDGE_LOOP ( 'NONE', ( #22815, #12146, #18713 ) ) ;
#27395 = CARTESIAN_POINT ( 'NONE',  ( -19.48557158514985588, -11.25000000000002309, 6.000000000000000000 ) ) ;
#27396 = CARTESIAN_POINT ( 'NONE',  ( 20.66414367075948277, 17.76245163070630184, 10.99999999999898037 ) ) ;
#27397 = PRODUCT_DEFINITION ( 'UNKNOWN', '', #15190, #33399 ) ;
#27398 = AXIS2_PLACEMENT_3D ( 'NONE', #14540, #8242, #17810 ) ;
#27399 = DIRECTION ( 'NONE',  ( 0.5877852522924690293, -0.8090169943749503378, 0.000000000000000000 ) ) ;
#27400 = ORIENTED_EDGE ( 'NONE', *, *, #4933, .F. ) ;
#27401 = ADVANCED_FACE ( 'NONE', ( #21702 ), #5863, .T. ) ;
#27402 = FACE_OUTER_BOUND ( 'NONE', #31208, .T. ) ;
#27403 = CARTESIAN_POINT ( 'NONE',  ( -2.525645716490711123, 8.212903943950955465, 11.00000000000000000 ) ) ;
#27404 = ADVANCED_FACE ( 'NONE', ( #34103 ), #27802, .T. ) ;
#27405 = DIRECTION ( 'NONE',  ( -0.000000000000000000, -0.000000000000000000, -1.000000000000000000 ) ) ;
#27406 = CARTESIAN_POINT ( 'NONE',  ( 30.06306975117524871, -23.11802603997359284, -6.283344179835762766 ) ) ;
#27407 = CARTESIAN_POINT ( 'NONE',  ( 17.66171978117526109, 15.32956390713761685, -15.88260630329942025 ) ) ;
#27408 = CARTESIAN_POINT ( 'NONE',  ( 8.281587164622539632, 23.34602691232715088, -19.97899749236660938 ) ) ;
#27409 = ORIENTED_EDGE ( 'NONE', *, *, #24947, .T. ) ;
#27410 = CARTESIAN_POINT ( 'NONE',  ( -19.92126674643909823, 9.807663499646920968, -19.05809710863068318 ) ) ;
#27411 = CARTESIAN_POINT ( 'NONE',  ( 8.927394655428276593, 11.06314620770945290, 9.000000000000001776 ) ) ;
#27412 = AXIS2_PLACEMENT_3D ( 'NONE', #28102, #21806, #12070 ) ;
#27413 = CARTESIAN_POINT ( 'NONE',  ( -1.358232629781535916, 33.31072022568110924, 6.000000000000000000 ) ) ;
#27414 = CARTESIAN_POINT ( 'NONE',  ( 9.734775949363912773, -18.28479368612017808, -27.43959765210956547 ) ) ;
#27415 = CARTESIAN_POINT ( 'NONE',  ( 8.505700342264139735, 22.10876900990906435, 9.000000000000001776 ) ) ;
#27416 = CARTESIAN_POINT ( 'NONE',  ( 22.52744239175980923, -0.1803094636422790109, -20.90349153981001606 ) ) ;
#27417 = CARTESIAN_POINT ( 'NONE',  ( -13.46909128543195777, 22.86125717629003873, -15.44550393738605187 ) ) ;
#27418 = CARTESIAN_POINT ( 'NONE',  ( -20.30842559917252288, -22.79334907695596613, -14.00205457863687997 ) ) ;
#27419 = CARTESIAN_POINT ( 'NONE',  ( 9.644836438174420934, -23.72159211153909908, -13.69389272877596575 ) ) ;
#27420 = EDGE_CURVE ( 'NONE', #32326, #8749, #31055, .T. ) ;
#27421 = AXIS2_PLACEMENT_3D ( 'NONE', #14248, #36389, #7945 ) ;
#27422 = CARTESIAN_POINT ( 'NONE',  ( -39.48531003256149319, -11.24999992065011156, 11.00000000000000000 ) ) ;
#27423 = EDGE_CURVE ( 'NONE', #30133, #1553, #3874, .T. ) ;
#27424 = EDGE_LOOP ( 'NONE', ( #38262, #35351, #652, #28991 ) ) ;
#27425 = ORIENTED_EDGE ( 'NONE', *, *, #27775, .T. ) ;
#27426 = CARTESIAN_POINT ( 'NONE',  ( -10.14280199068175214, 30.64235453448604218, -12.13460695665965972 ) ) ;
#27427 = CARTESIAN_POINT ( 'NONE',  ( 0.9658050764552033041, 37.18846563620834189, 10.49999999999999822 ) ) ;
#27428 = CARTESIAN_POINT ( 'NONE',  ( -0.6417741116369681809, 11.68927977431952137, 6.000000000000000000 ) ) ;
#27429 = VECTOR ( 'NONE', #26483, 1000.000000000000000 ) ;
#27430 = CARTESIAN_POINT ( 'NONE',  ( -9.415016184005896349, 11.18446770392341350, 10.49999999999999822 ) ) ;
#27431 = ORIENTED_EDGE ( 'NONE', *, *, #28641, .T. ) ;
#27432 = CARTESIAN_POINT ( 'NONE',  ( 26.50276232455322400, 0.2790718576921050187, -15.45068151253284761 ) ) ;
#27433 = DIRECTION ( 'NONE',  ( 1.000000000000000000, 0.000000000000000000, 0.000000000000000000 ) ) ;
#27434 = CARTESIAN_POINT ( 'NONE',  ( 14.06524961900336734, 27.71236540882597410, 7.000000000000000000 ) ) ;
#27435 = VERTEX_POINT ( 'NONE', #24747 ) ;
#27436 = CARTESIAN_POINT ( 'NONE',  ( -30.32473157615882542, 0.02510865282379010077, -8.297974377023098924 ) ) ;
#27437 = DIRECTION ( 'NONE',  ( -0.6691306063588576825, 0.7431448254773946882, 0.000000000000000000 ) ) ;
#27438 = ORIENTED_EDGE ( 'NONE', *, *, #18791, .T. ) ;
#27439 = CARTESIAN_POINT ( 'NONE',  ( 32.94587109690223059, -4.956964677168978817, -9.466786290515122104 ) ) ;
#27440 = ORIENTED_EDGE ( 'NONE', *, *, #20930, .T. ) ;
#27441 = CARTESIAN_POINT ( 'NONE',  ( 13.65033576027476414, 34.08684981564654493, 12.73282698324863738 ) ) ;
#27442 = CARTESIAN_POINT ( 'NONE',  ( 11.73759695151994009, -17.78600041297262635, 20.69868183039754328 ) ) ;
#27443 = DIRECTION ( 'NONE',  ( -0.2079116908177533474, 0.9781476007338067991, -0.000000000000000000 ) ) ;
#27444 = ADVANCED_FACE ( 'NONE', ( #15609 ), #21310, .T. ) ;
#27445 = CARTESIAN_POINT ( 'NONE',  ( -4.528037020496219256, 32.30201321073018050, 19.99202127657103389 ) ) ;
#27446 = AXIS2_PLACEMENT_3D ( 'NONE', #33327, #2240, #14628 ) ;
#27447 = DIRECTION ( 'NONE',  ( 0.000000000000000000, 0.000000000000000000, 1.000000000000000000 ) ) ;
#27448 = ORIENTED_EDGE ( 'NONE', *, *, #38667, .T. ) ;
#27449 = CARTESIAN_POINT ( 'NONE',  ( 19.48557158514988075, -11.24999999999998224, 3.000000000000000000 ) ) ;
#27450 = AXIS2_PLACEMENT_3D ( 'NONE', #28112, #18580, #40104 ) ;
#27451 = CYLINDRICAL_SURFACE ( 'NONE', #14337, 1.000000000000000888 ) ;
#27452 = CARTESIAN_POINT ( 'NONE',  ( 3.517372515104220998, 21.68025459727664384, -24.29102002352656697 ) ) ;
#27453 = VECTOR ( 'NONE', #4664, 999.9999999999998863 ) ;
#27454 = DIRECTION ( 'NONE',  ( 1.000000000000000000, 0.000000000000000000, 0.000000000000000000 ) ) ;
#27455 = CARTESIAN_POINT ( 'NONE',  ( 16.89748511972537770, 9.755767582501292168, 19.99202127657103389 ) ) ;
#27456 = CARTESIAN_POINT ( 'NONE',  ( 16.88935835353887427, -24.86429512234964534, -12.34860920598776168 ) ) ;
#27457 = CARTESIAN_POINT ( 'NONE',  ( -9.911438049898041669, 11.24107483890965575, 7.000000000000000000 ) ) ;
#27458 = CARTESIAN_POINT ( 'NONE',  ( -6.354454053420248272, 35.54304081427989814, 7.000000000000000000 ) ) ;
#27459 = CARTESIAN_POINT ( 'NONE',  ( 9.593266739736579396, 18.11602540378440196, 10.50000000000000178 ) ) ;
#27460 = EDGE_LOOP ( 'NONE', ( #38328, #3724, #25384, #14429, #13897, #7827, #10828 ) ) ;
#27461 = AXIS2_PLACEMENT_3D ( 'NONE', #8272, #5226, #39550 ) ;
#27462 = ORIENTED_EDGE ( 'NONE', *, *, #17005, .T. ) ;
#27463 = CARTESIAN_POINT ( 'NONE',  ( -14.75406920065014482, 25.34787871228437695, -10.65428902387546728 ) ) ;
#27464 = CIRCLE ( 'NONE', #28095, 60.00000000000002132 ) ;
#27465 = CARTESIAN_POINT ( 'NONE',  ( -32.91936639158274858, -8.047070124328334018, 18.42518152272033660 ) ) ;
#27466 = CARTESIAN_POINT ( 'NONE',  ( 10.46763271599406053, -19.59569900990302571, -22.74339197413747371 ) ) ;
#27467 = CARTESIAN_POINT ( 'NONE',  ( -14.06932099033139849, 26.54566839026276170, 11.00000000000000000 ) ) ;
#27468 = VERTEX_POINT ( 'NONE', #21896 ) ;
#27469 = VERTEX_POINT ( 'NONE', #16009 ) ;
#27471 = CARTESIAN_POINT ( 'NONE',  ( 8.347978306607052090, 10.15934277794823437, 10.82238861112330497 ) ) ;
#27470 = CARTESIAN_POINT ( 'NONE',  ( -13.23108492885968523, 26.81331637706469806, -12.36580983879895612 ) ) ;
#27472 = CARTESIAN_POINT ( 'NONE',  ( -14.75978416138969962, -21.06827879612096055, -18.13044228312590178 ) ) ;
#27473 = CARTESIAN_POINT ( 'NONE',  ( 1.693998953219503667, 12.12549434688615513, 10.00000000000000000 ) ) ;
#27474 = EDGE_CURVE ( 'NONE', #35589, #25619, #9117, .T. ) ;
#27475 = CIRCLE ( 'NONE', #13872, 1.000000000000000000 ) ;
#27476 = ORIENTED_EDGE ( 'NONE', *, *, #28253, .T. ) ;
#27477 = CARTESIAN_POINT ( 'NONE',  ( -31.75624639457006637, -11.96584483983997771, -12.01004037356029031 ) ) ;
#27478 = CARTESIAN_POINT ( 'NONE',  ( -14.17779411611103946, -25.03930879169686108, -11.60410842717421609 ) ) ;
#27479 = CARTESIAN_POINT ( 'NONE',  ( 38.66460482714475688, -17.32098561216329458, 11.00000000000000000 ) ) ;
#27480 = EDGE_LOOP ( 'NONE', ( #8369, #29170, #29512, #30169 ) ) ;
#27481 = CARTESIAN_POINT ( 'NONE',  ( 21.96305308675481172, 3.028777170395801299, -21.88341145178896596 ) ) ;
#27482 = LINE ( 'NONE', #25231, #34277 ) ;
#27483 =( GEOMETRIC_REPRESENTATION_CONTEXT ( 3 ) GLOBAL_UNCERTAINTY_ASSIGNED_CONTEXT ( ( #8593 ) ) GLOBAL_UNIT_ASSIGNED_CONTEXT ( ( #11767, #35956, #24153 ) ) REPRESENTATION_CONTEXT ( 'NONE', 'WORKASPACE' ) );
#27484 = CARTESIAN_POINT ( 'NONE',  ( 10.49474413300068854, 21.89971208337374975, 11.00000000000000000 ) ) ;
#27485 = EDGE_LOOP ( 'NONE', ( #6917, #24291, #16343, #2147 ) ) ;
#27486 = CARTESIAN_POINT ( 'NONE',  ( -23.34921024300090053, 0.4641876397533150622, -20.52991899298079659 ) ) ;
#27487 = ORIENTED_EDGE ( 'NONE', *, *, #22993, .T. ) ;
#27488 = CARTESIAN_POINT ( 'NONE',  ( 20.86070950977947547, 0.1829700343765511272, -26.78014837192183251 ) ) ;
#27489 = AXIS2_PLACEMENT_3D ( 'NONE', #9516, #15805, #167 ) ;
#27490 = CARTESIAN_POINT ( 'NONE',  ( 32.65234849725225530, -15.41672394535051893, 18.42518152272110044 ) ) ;
#27491 = ORIENTED_EDGE ( 'NONE', *, *, #28654, .T. ) ;
#27492 = CARTESIAN_POINT ( 'NONE',  ( -21.64712599719590713, 2.830533044877102000, -22.97171106603809321 ) ) ;
#27493 = PLANE ( 'NONE',  #22912 ) ;
#27494 = ADVANCED_FACE ( 'NONE', ( #376 ), #28194, .F. ) ;
#27495 = CARTESIAN_POINT ( 'NONE',  ( -12.05736835487443415, 14.38397459621567442, 10.49999999999999822 ) ) ;
#27496 = CIRCLE ( 'NONE', #15175, 15.00000000000000000 ) ;
#27497 = CARTESIAN_POINT ( 'NONE',  ( -16.60464863832890003, -22.41657912773202099, 19.66345542862528717 ) ) ;
#27498 = EDGE_CURVE ( 'NONE', #16093, #27094, #24556, .T. ) ;
#27499 = CYLINDRICAL_SURFACE ( 'NONE', #27936, 0.5000000000000004441 ) ;
#27500 = AXIS2_PLACEMENT_3D ( 'NONE', #26659, #36409, #5519 ) ;
#27501 = EDGE_CURVE ( 'NONE', #12231, #18928, #25146, .T. ) ;
#27502 = FACE_BOUND ( 'NONE', #34892, .T. ) ;
#27503 = CARTESIAN_POINT ( 'NONE',  ( -11.41268156625113406, 18.79179606750104981, 6.000000000000000000 ) ) ;
#27504 = ORIENTED_EDGE ( 'NONE', *, *, #36174, .T. ) ;
#27505 = CARTESIAN_POINT ( 'NONE',  ( -20.58226371439221225, 7.343079615373506286, -21.10892354972650509 ) ) ;
#27506 = CARTESIAN_POINT ( 'NONE',  ( -11.03641663870442713, 15.85735326529964873, 12.00000000000000000 ) ) ;
#27507 = CARTESIAN_POINT ( 'NONE',  ( -13.01838097023000707, 23.73363068877903359, 6.000000000000000000 ) ) ;
#27508 = CARTESIAN_POINT ( 'NONE',  ( 25.01399590262306205, -25.94755112289962895, -7.176433082738011393 ) ) ;
#27509 = CARTESIAN_POINT ( 'NONE',  ( -11.03641663870442713, 15.85735326529964873, 6.000000000000000000 ) ) ;
#27510 = CARTESIAN_POINT ( 'NONE',  ( 11.10459398110999629, 18.19651370294324977, -24.98634877528791876 ) ) ;
#27511 = CARTESIAN_POINT ( 'NONE',  ( 15.03860650580597991, -28.48662463501975139, 12.73282698324853257 ) ) ;
#27512 = ORIENTED_EDGE ( 'NONE', *, *, #20532, .T. ) ;
#27513 = CIRCLE ( 'NONE', #29454, 6.000000000000003553 ) ;
#27514 = CARTESIAN_POINT ( 'NONE',  ( -14.01353083633360441, 19.92937566205294786, -17.60551373979553347 ) ) ;
#27515 = CARTESIAN_POINT ( 'NONE',  ( -21.62094419769859144, -18.41873747672905282, 20.82122704794093693 ) ) ;
#27516 = DIRECTION ( 'NONE',  ( -0.000000000000000000, -0.000000000000000000, -1.000000000000000000 ) ) ;
#27517 = CARTESIAN_POINT ( 'NONE',  ( 12.67211246595664598, 21.02606612804661879, -18.45550099276037415 ) ) ;
#27518 = ORIENTED_EDGE ( 'NONE', *, *, #29360, .T. ) ;
#27519 = CARTESIAN_POINT ( 'NONE',  ( -6.651296319737220131, 27.81603774131167839, 7.000000000000000000 ) ) ;
#27520 = EDGE_CURVE ( 'NONE', #18869, #12427, #24645, .T. ) ;
#27521 = ORIENTED_EDGE ( 'NONE', *, *, #12857, .F. ) ;
#27523 = CARTESIAN_POINT ( 'NONE',  ( -4.348113209407908464, 9.835177808069893501, 12.00000000000000000 ) ) ;
#27522 = CARTESIAN_POINT ( 'NONE',  ( -13.69293301799758034, 23.56752051744286192, -14.45830943805128932 ) ) ;
#27524 = EDGE_CURVE ( 'NONE', #13055, #18790, #6648, .T. ) ;
#27525 = CARTESIAN_POINT ( 'NONE',  ( -9.658050167131792207, -18.22926657306539866, -28.07251639296444168 ) ) ;
#27526 = CARTESIAN_POINT ( 'NONE',  ( 9.080802685385512163, 10.85199816882120416, 10.94611345180490680 ) ) ;
#27527 = EDGE_CURVE ( 'NONE', #15652, #23393, #11964, .T. ) ;
#27528 = CARTESIAN_POINT ( 'NONE',  ( -34.06221145678576079, -17.84677894165469070, -4.999999999999999112 ) ) ;
#27529 = AXIS2_PLACEMENT_3D ( 'NONE', #13760, #13560, #38751 ) ;
#27530 = CARTESIAN_POINT ( 'NONE',  ( -10.58748765286974702, -24.15557699858428009, -12.67670956590171016 ) ) ;
#27531 = LINE ( 'NONE', #9241, #15075 ) ;
#27532 = CARTESIAN_POINT ( 'NONE',  ( 16.13774221630713157, 23.57012646024468339, -7.846364408462076057 ) ) ;
#27533 = ORIENTED_EDGE ( 'NONE', *, *, #17159, .T. ) ;
#27534 = CARTESIAN_POINT ( 'NONE',  ( 24.60615563309142573, 7.381059274176844376, -6.443417821428254477 ) ) ;
#27535 = CARTESIAN_POINT ( 'NONE',  ( 13.63581098909227052, 27.45627467658428600, 9.500000000000000000 ) ) ;
#27536 = DIRECTION ( 'NONE',  ( 0.000000000000000000, 0.000000000000000000, 1.000000000000000000 ) ) ;
#27537 = DIRECTION ( 'NONE',  ( 1.000000000000000000, 0.000000000000000000, 0.000000000000000000 ) ) ;
#27538 = VERTEX_POINT ( 'NONE', #2819 ) ;
#27539 = CARTESIAN_POINT ( 'NONE',  ( -21.05108527408817665, -0.1996147791734167454, -26.13566238484483506 ) ) ;
#27540 = AXIS2_PLACEMENT_3D ( 'NONE', #23813, #11226, #8380 ) ;
#27541 = CARTESIAN_POINT ( 'NONE',  ( 30.05477332892332498, -0.03847789688773560479, -9.234382374539894300 ) ) ;
#27542 = CARTESIAN_POINT ( 'NONE',  ( 11.41267482483262619, 26.20820393249957192, 12.00000000000000000 ) ) ;
#27543 = CARTESIAN_POINT ( 'NONE',  ( 26.17801803039862918, -8.007547698857949925, 20.82122704794080903 ) ) ;
#27544 = CARTESIAN_POINT ( 'NONE',  ( 16.24796006241085422, 15.88921519459651144, -30.00000000000001421 ) ) ;
#27545 = EDGE_CURVE ( 'NONE', #38699, #10050, #27601, .T. ) ;
#27546 = CARTESIAN_POINT ( 'NONE',  ( 4.211395437248501850, 12.61633075744433796, 6.000000000000000000 ) ) ;
#27547 = CIRCLE ( 'NONE', #2267, 0.5000000000000004441 ) ;
#27548 = ADVANCED_FACE ( 'NONE', ( #36951 ), #21501, .T. ) ;
#27549 = ORIENTED_EDGE ( 'NONE', *, *, #9525, .T. ) ;
#27550 = DIRECTION ( 'NONE',  ( 1.000000000000000000, 0.000000000000000000, 0.000000000000000000 ) ) ;
#27551 = CARTESIAN_POINT ( 'NONE',  ( 2.620168631248871005, 12.57794293788735729, 10.74999999999999289 ) ) ;
#27552 = CARTESIAN_POINT ( 'NONE',  ( 14.04783364825886238, 26.18819932152407404, 10.66666666666666607 ) ) ;
#27553 = CARTESIAN_POINT ( 'NONE',  ( 2.739358956307748727, 38.25484015033369189, -5.856888471774574612 ) ) ;
#27554 = DIRECTION ( 'NONE',  ( 0.3090169943749573322, 0.9510565162951504226, -0.000000000000000000 ) ) ;
#27555 = CARTESIAN_POINT ( 'NONE',  ( 5.982165713378432059, 28.55918256678898715, 9.000000000000001776 ) ) ;
#27556 = CARTESIAN_POINT ( 'NONE',  ( -9.705584749708384251, 11.06314620770957013, 7.221809905720049549 ) ) ;
#27557 = CARTESIAN_POINT ( 'NONE',  ( 11.48173768534036121, 32.16538668264416145, 7.000000000000000000 ) ) ;
#27558 = CARTESIAN_POINT ( 'NONE',  ( -3.503793317224518145, 8.420815634768723967, 11.00000000000000000 ) ) ;
#27559 = CARTESIAN_POINT ( 'NONE',  ( -5.537946624085890335, 36.44027069998196566, 7.500000000000000888 ) ) ;
#27560 = AXIS2_PLACEMENT_3D ( 'NONE', #26613, #14423, #39207 ) ;
#27561 = CARTESIAN_POINT ( 'NONE',  ( 10.27379371539876907, 17.74076016529687649, -29.33306961566889015 ) ) ;
#27562 = CARTESIAN_POINT ( 'NONE',  ( 11.94134295108989363, 16.18301270189217078, 7.000000000000000000 ) ) ;
#27563 = ORIENTED_EDGE ( 'NONE', *, *, #25042, .T. ) ;
#27565 = DIRECTION ( 'NONE',  ( -0.9135454576426059736, -0.4067366430757888285, 0.000000000000000000 ) ) ;
#27564 = CARTESIAN_POINT ( 'NONE',  ( -18.73768915581330674, 17.66930787322032259, -5.479690743329737046 ) ) ;
#27566 = CARTESIAN_POINT ( 'NONE',  ( -13.67979938750370650, 27.47056737363399392, 10.99999999999999289 ) ) ;
#27567 = CARTESIAN_POINT ( 'NONE',  ( 14.05380968864566071, -24.61301880703936362, -12.55008158153441578 ) ) ;
#27568 = CARTESIAN_POINT ( 'NONE',  ( -16.28627583843819693, -20.60454327135679975, -17.98998692793695398 ) ) ;
#27569 = CARTESIAN_POINT ( 'NONE',  ( 15.23218277980887159, 26.40650644525699775, -7.827771362956433165 ) ) ;
#27570 = CARTESIAN_POINT ( 'NONE',  ( 10.96431188987212479, 17.32148673788787718, -30.00000000000000355 ) ) ;
#27571 = EDGE_LOOP ( 'NONE', ( #7740, #20783, #28388, #3623 ) ) ;
#27572 = CIRCLE ( 'NONE', #13288, 0.9999999999999992228 ) ;
#27573 = DIRECTION ( 'NONE',  ( -1.000000000000000000, 0.000000000000000000, 0.000000000000000000 ) ) ;
#27574 = CARTESIAN_POINT ( 'NONE',  ( -14.42035624161473883, 26.65972665747678860, 7.000000000000000000 ) ) ;
#27575 = CARTESIAN_POINT ( 'NONE',  ( -20.72701401736282989, -28.35932241216953287, 14.53008259254010959 ) ) ;
#27576 = VECTOR ( 'NONE', #24750, 1000.000000000000000 ) ;
#27577 = CARTESIAN_POINT ( 'NONE',  ( -28.40992215798796039, -23.67713899482849627, -7.998235878429071910 ) ) ;
#27578 = CARTESIAN_POINT ( 'NONE',  ( -0.3593151151631351348, -23.72602201120211518, -12.88856356360667199 ) ) ;
#27579 = CARTESIAN_POINT ( 'NONE',  ( 14.53668546275618567, 23.85743596623326823, -12.57427534489166021 ) ) ;
#27580 = CARTESIAN_POINT ( 'NONE',  ( 17.58908954919914436, 10.72208735757384979, -27.73727666948197879 ) ) ;
#27581 = CARTESIAN_POINT ( 'NONE',  ( 14.47283171447379502, 21.48159823030311344, 7.000000000000000000 ) ) ;
#27582 = ADVANCED_FACE ( 'NONE', ( #34692 ), #569, .F. ) ;
#27583 = CARTESIAN_POINT ( 'NONE',  ( -3.525063703014029048, 20.58869973712754842, -27.01785507751000637 ) ) ;
#27584 = ORIENTED_EDGE ( 'NONE', *, *, #7561, .F. ) ;
#27585 = CARTESIAN_POINT ( 'NONE',  ( -33.08849987016296978, -5.231495020973413901, -9.455626480001546597 ) ) ;
#27586 = CARTESIAN_POINT ( 'NONE',  ( -32.18944385490033255, 1.219497045965482140, 12.73282698324853079 ) ) ;
#27587 = ORIENTED_EDGE ( 'NONE', *, *, #9790, .F. ) ;
#27588 = DIRECTION ( 'NONE',  ( 1.000000000000000000, 0.000000000000000000, 0.000000000000000000 ) ) ;
#27589 = LINE ( 'NONE', #27984, #5066 ) ;
#27590 = CARTESIAN_POINT ( 'NONE',  ( -30.04950648410215308, 0.8457024189327569941, -5.000000000000000000 ) ) ;
#27591 = CARTESIAN_POINT ( 'NONE',  ( 27.95927371423643848, -10.27070572539359716, -15.74113732760950413 ) ) ;
#27592 = AXIS2_PLACEMENT_3D ( 'NONE', #14381, #26768, #39158 ) ;
#27593 = EDGE_LOOP ( 'NONE', ( #31725, #8931, #6982, #10703 ) ) ;
#27594 = DIRECTION ( 'NONE',  ( 1.000000000000000000, 0.000000000000000000, 0.000000000000000000 ) ) ;
#27595 = ORIENTED_EDGE ( 'NONE', *, *, #22762, .T. ) ;
#27596 = LINE ( 'NONE', #33905, #36565 ) ;
#27597 = VECTOR ( 'NONE', #9433, 1000.000000000000000 ) ;
#27598 = CARTESIAN_POINT ( 'NONE',  ( 11.11016527260166420, 31.83082137946473367, 11.00000000000000000 ) ) ;
#27599 = AXIS2_PLACEMENT_3D ( 'NONE', #36309, #12118, #36902 ) ;
#27600 = CIRCLE ( 'NONE', #1015, 0.4999999999999997780 ) ;
#27601 = LINE ( 'NONE', #15213, #14911 ) ;
#27602 = ORIENTED_EDGE ( 'NONE', *, *, #37481, .T. ) ;
#27603 = CARTESIAN_POINT ( 'NONE',  ( -1.631256786664503577, 20.52137151614312316, -28.45067076138309403 ) ) ;
#27604 = DIRECTION ( 'NONE',  ( 0.8090169943749503378, 0.5877852522924690293, 0.000000000000000000 ) ) ;
#27605 = PLANE ( 'NONE',  #23468 ) ;
#27606 = CARTESIAN_POINT ( 'NONE',  ( 26.21828973787456007, -21.49016925214971963, -12.01153406443311766 ) ) ;
#27607 = CARTESIAN_POINT ( 'NONE',  ( 17.12406237791118357, 13.45638816638915358, -21.13750791658128847 ) ) ;
#27608 = CARTESIAN_POINT ( 'NONE',  ( 13.73220224370217579, 30.78478150535875457, -4.999999999999995559 ) ) ;
#27609 = ORIENTED_EDGE ( 'NONE', *, *, #38260, .F. ) ;
#27610 = CARTESIAN_POINT ( 'NONE',  ( -21.15916498104113685, 10.31847808661841626, -13.90054347323569139 ) ) ;
#27611 = PLANE ( 'NONE',  #15307 ) ;
#27612 = CARTESIAN_POINT ( 'NONE',  ( 9.721599711338530625, -18.19680360149917320, -28.06894580268500405 ) ) ;
#27613 = LINE ( 'NONE', #33731, #2254 ) ;
#27614 = CARTESIAN_POINT ( 'NONE',  ( 33.62187204924162387, 0.04418559750795045954, -13.79123840944733992 ) ) ;
#27615 = CARTESIAN_POINT ( 'NONE',  ( -15.09127514311057716, 26.17197197711360346, -8.766134727060833853 ) ) ;
#27616 = CARTESIAN_POINT ( 'NONE',  ( -14.12043127772994922, -15.90989924622459384, -25.81352569219153281 ) ) ;
#27617 = CARTESIAN_POINT ( 'NONE',  ( 8.584620562788320086, -18.61902014996657684, -30.00000000000000000 ) ) ;
#27618 = EDGE_CURVE ( 'NONE', #1914, #7168, #35295, .T. ) ;
#27619 = DIRECTION ( 'NONE',  ( 0.000000000000000000, -0.000000000000000000, 1.000000000000000000 ) ) ;
#27620 = EDGE_LOOP ( 'NONE', ( #13396, #10754, #32800 ) ) ;
#27621 = ORIENTED_EDGE ( 'NONE', *, *, #26343, .F. ) ;
#27622 = CARTESIAN_POINT ( 'NONE',  ( -10.17671610307063546, 34.24920776341300410, -7.617059711015554235 ) ) ;
#27623 = CONICAL_SURFACE ( 'NONE', #25675, 1.000000000000004441, 0.7853981633974526089 ) ;
#27624 = FACE_OUTER_BOUND ( 'NONE', #29967, .T. ) ;
#27625 = CARTESIAN_POINT ( 'NONE',  ( 12.68475447279711510, 27.14725768220934299, 10.50000000000000000 ) ) ;
#27626 = AXIS2_PLACEMENT_3D ( 'NONE', #6553, #3516, #474 ) ;
#27627 = CONICAL_SURFACE ( 'NONE', #10110, 1.000000000000004441, 0.7853981633974548293 ) ;
#27628 = DIRECTION ( 'NONE',  ( 0.000000000000000000, 0.000000000000000000, -1.000000000000000000 ) ) ;
#27629 = ORIENTED_EDGE ( 'NONE', *, *, #2123, .F. ) ;
#27630 = CARTESIAN_POINT ( 'NONE',  ( 30.60837755444375929, -0.01021490497896947874, -7.357883460921571306 ) ) ;
#27631 = EDGE_CURVE ( 'NONE', #37992, #21619, #23101, .T. ) ;
#27632 = CARTESIAN_POINT ( 'NONE',  ( -15.41558956984166251, 26.78481017248024898, -5.000000000000000000 ) ) ;
#27633 = AXIS2_PLACEMENT_3D ( 'NONE', #28355, #10272, #18826 ) ;
#27634 = CARTESIAN_POINT ( 'NONE',  ( -8.927394655428429360, 11.06314620770957013, 7.000000000000000000 ) ) ;
#27635 = ADVANCED_FACE ( 'NONE', ( #37743 ), #7050, .T. ) ;
#27636 = ORIENTED_EDGE ( 'NONE', *, *, #14923, .F. ) ;
#27637 = CARTESIAN_POINT ( 'NONE',  ( -30.14882232463217804, 0.05009394220924950902, -8.768162902875424436 ) ) ;
#27638 = CARTESIAN_POINT ( 'NONE',  ( 23.05386822411318803, -7.747535282638377652, 23.00000000000000000 ) ) ;
#27639 = ORIENTED_EDGE ( 'NONE', *, *, #31867, .T. ) ;
#27640 = CARTESIAN_POINT ( 'NONE',  ( 33.62754581830257194, -6.995946598033712327, -9.406918306848506717 ) ) ;
#27641 = ORIENTED_EDGE ( 'NONE', *, *, #24248, .F. ) ;
#27642 = CARTESIAN_POINT ( 'NONE',  ( 3.827636526755794577, 39.84991882288247211, 13.32518128616622555 ) ) ;
#27643 = CARTESIAN_POINT ( 'NONE',  ( -5.869341256201681567, -17.04122685614420263, 20.69868183039781684 ) ) ;
#27644 = CARTESIAN_POINT ( 'NONE',  ( -22.57322471865059299, -29.08065073755651042, -4.999999999999997335 ) ) ;
#27645 = CARTESIAN_POINT ( 'NONE',  ( 8.810137414575107684, 27.17888719461359415, 20.25080042701567251 ) ) ;
#27646 = CARTESIAN_POINT ( 'NONE',  ( 5.458865582155095986, 18.48521636184714012, 13.00000000000000178 ) ) ;
#27647 = EDGE_LOOP ( 'NONE', ( #14211, #21350, #28806, #23848 ) ) ;
#27648 = CARTESIAN_POINT ( 'NONE',  ( 7.713869163865849643, 10.18146832927074996, 7.500000000000000888 ) ) ;
#27649 = CARTESIAN_POINT ( 'NONE',  ( -17.01882136418225500, 27.23043334310857588, 13.32518128616609054 ) ) ;
#27650 = EDGE_CURVE ( 'NONE', #19611, #22765, #29836, .T. ) ;
#27651 = FACE_OUTER_BOUND ( 'NONE', #38382, .T. ) ;
#27652 = EDGE_CURVE ( 'NONE', #10849, #6755, #25283, .T. ) ;
#27653 = CARTESIAN_POINT ( 'NONE',  ( 6.651296319737277862, 27.81603774131160023, 7.000000000000000000 ) ) ;
#27654 = CARTESIAN_POINT ( 'NONE',  ( 7.126104678631604905, 36.82515065381944197, -5.439468800721699360 ) ) ;
#27655 = CIRCLE ( 'NONE', #27025, 0.5000000000000000000 ) ;
#27656 = FACE_OUTER_BOUND ( 'NONE', #13227, .T. ) ;
#27657 = CIRCLE ( 'NONE', #30197, 6.000000000000003553 ) ;
#27658 = CARTESIAN_POINT ( 'NONE',  ( 17.23496854698099057, -26.67902877899678060, -8.224554605899342619 ) ) ;
#27659 = CARTESIAN_POINT ( 'NONE',  ( -3.992867117591420545, 8.524771480177605554, 9.500000000000000000 ) ) ;
#27660 = DIRECTION ( 'NONE',  ( 0.000000000000000000, 0.000000000000000000, 1.000000000000000000 ) ) ;
#27661 = DIRECTION ( 'NONE',  ( -0.000000000000000000, -0.000000000000000000, 1.000000000000000000 ) ) ;
#27662 = ORIENTED_EDGE ( 'NONE', *, *, #13011, .T. ) ;
#27663 = CARTESIAN_POINT ( 'NONE',  ( -12.28379231215668810, 19.74341564248685899, -20.56797969728914310 ) ) ;
#27664 = CARTESIAN_POINT ( 'NONE',  ( -33.25367603495013213, -15.60696645162129315, 17.92354375535250810 ) ) ;
#27665 = CARTESIAN_POINT ( 'NONE',  ( 14.08933265271751978, -25.02402006024204084, -11.60661225095639715 ) ) ;
#27666 = CARTESIAN_POINT ( 'NONE',  ( 11.89031559783845005, 11.79390851039467236, 13.00000000000000178 ) ) ;
#27667 = ORIENTED_EDGE ( 'NONE', *, *, #4197, .T. ) ;
#27668 = ORIENTED_EDGE ( 'NONE', *, *, #32366, .F. ) ;
#27669 = CARTESIAN_POINT ( 'NONE',  ( -14.28732406086307449, 29.23536459232070328, -7.289172933315514413 ) ) ;
#27670 = CARTESIAN_POINT ( 'NONE',  ( -19.47283267323017597, -27.28889818631711250, -5.458695607782805048 ) ) ;
#27671 = EDGE_CURVE ( 'NONE', #17473, #2121, #33743, .T. ) ;
#27672 = CARTESIAN_POINT ( 'NONE',  ( 13.58430815669644254, 27.61478409596681516, 10.83333333333333215 ) ) ;
#27673 = ORIENTED_EDGE ( 'NONE', *, *, #22653, .T. ) ;
#27674 = CARTESIAN_POINT ( 'NONE',  ( -35.47307300072858283, -9.938437602308624719, -5.000000000000004441 ) ) ;
#27675 = CARTESIAN_POINT ( 'NONE',  ( -13.21629450091423053, -23.60900218953552354, -14.48483131059268558 ) ) ;
#27676 = CARTESIAN_POINT ( 'NONE',  ( 31.08218589456554071, -27.68808744834075597, 11.00000000000000000 ) ) ;
#27677 = ORIENTED_EDGE ( 'NONE', *, *, #19305, .F. ) ;
#27678 = CARTESIAN_POINT ( 'NONE',  ( 25.25749706778072579, 1.346561751027687936, -16.53357011407651456 ) ) ;
#27679 = FACE_OUTER_BOUND ( 'NONE', #35296, .T. ) ;
#27680 = CARTESIAN_POINT ( 'NONE',  ( 6.354454053420411697, 35.54304081427980577, 7.000000000000000000 ) ) ;
#27681 = ORIENTED_EDGE ( 'NONE', *, *, #24649, .F. ) ;
#27682 = CARTESIAN_POINT ( 'NONE',  ( -26.56841411643160455, 0.1811368447264279369, -15.43893401616002947 ) ) ;
#27683 = ORIENTED_EDGE ( 'NONE', *, *, #162, .T. ) ;
#27684 = CARTESIAN_POINT ( 'NONE',  ( 20.64823133129570110, -0.2909966358367886974, -28.02009057262635139 ) ) ;
#27685 = AXIS2_PLACEMENT_3D ( 'NONE', #38870, #17549, #1493 ) ;
#27686 = CARTESIAN_POINT ( 'NONE',  ( 24.51396478725026640, -11.15767879383071026, 21.00000000000001066 ) ) ;
#27687 = CARTESIAN_POINT ( 'NONE',  ( 33.86703583613424939, -12.56047426484072993, 17.92354375535250455 ) ) ;
#27688 = EDGE_LOOP ( 'NONE', ( #19933, #5724 ) ) ;
#27689 = CARTESIAN_POINT ( 'NONE',  ( -20.52618863457681542, 3.592373843541286416, -26.42718072739731028 ) ) ;
#27690 = PLANE ( 'NONE',  #219 ) ;
#27691 = DIRECTION ( 'NONE',  ( -0.000000000000000000, -0.000000000000000000, -1.000000000000000000 ) ) ;
#27692 = CARTESIAN_POINT ( 'NONE',  ( -33.88090307477148855, -0.3823557797707961003, 10.99999999999973355 ) ) ;
#27693 = CARTESIAN_POINT ( 'NONE',  ( -2.871208588069141143, 13.69667159339610762, 13.00000000000000178 ) ) ;
#27694 = EDGE_CURVE ( 'NONE', #6928, #9314, #26590, .T. ) ;
#27695 = CARTESIAN_POINT ( 'NONE',  ( -6.651296319737220131, 27.81603774131167839, 9.000000000000001776 ) ) ;
#27696 = CARTESIAN_POINT ( 'NONE',  ( 32.18944385490472371, 1.219497045960946657, 12.73282698324853257 ) ) ;
#27697 = ORIENTED_EDGE ( 'NONE', *, *, #36311, .F. ) ;
#27698 = CARTESIAN_POINT ( 'NONE',  ( -24.12023144843434252, 8.019543126731839777, -6.929311169682339511 ) ) ;
#27699 = CARTESIAN_POINT ( 'NONE',  ( -6.330077540933487512, 17.71145523154927659, 13.00000000000000178 ) ) ;
#27700 = DIRECTION ( 'NONE',  ( -0.000000000000000000, -0.000000000000000000, -1.000000000000000000 ) ) ;
#27701 = CARTESIAN_POINT ( 'NONE',  ( 13.79453690055875370, -15.27553076837868495, -28.53576636504390152 ) ) ;
#27702 = DIRECTION ( 'NONE',  ( -0.000000000000000000, -0.000000000000000000, -1.000000000000000000 ) ) ;
#27703 = CARTESIAN_POINT ( 'NONE',  ( 15.21680204932512304, 26.78069555836370697, -7.350879659809681499 ) ) ;
#27704 = CIRCLE ( 'NONE', #16054, 1.000000000000000888 ) ;
#27705 = VERTEX_POINT ( 'NONE', #6847 ) ;
#27707 = AXIS2_PLACEMENT_3D ( 'NONE', #32689, #7480, #1803 ) ;
#27706 = CARTESIAN_POINT ( 'NONE',  ( -12.84546241753605855, 16.03363458260228924, -28.77567867939699653 ) ) ;
#27708 = CARTESIAN_POINT ( 'NONE',  ( -21.38319344285576662, -17.62079982023109181, 20.94377226548387938 ) ) ;
#27709 = DIRECTION ( 'NONE',  ( -1.000000000000000000, 0.000000000000000000, 0.000000000000000000 ) ) ;
#27710 = CARTESIAN_POINT ( 'NONE',  ( 11.05637708650255036, 17.41422535994987086, -28.07838520724235565 ) ) ;
#27711 = ORIENTED_EDGE ( 'NONE', *, *, #24165, .T. ) ;
#27712 = CARTESIAN_POINT ( 'NONE',  ( -2.485571585149885632, -11.24999999999987566, 10.00000000000000000 ) ) ;
#27713 = EDGE_LOOP ( 'NONE', ( #30660, #16244, #25925 ) ) ;
#27714 = AXIS2_PLACEMENT_3D ( 'NONE', #33505, #11556, #38980 ) ;
#27716 = FACE_OUTER_BOUND ( 'NONE', #27424, .T. ) ;
#27715 = CARTESIAN_POINT ( 'NONE',  ( -12.00916977197048752, 20.06877922548516935, -20.51635596422970664 ) ) ;
#27717 = B_SPLINE_CURVE_WITH_KNOTS ( 'NONE', 3,
 ( #21336, #11988, #21925, #36775, #3248, #30880 ),
 .UNSPECIFIED., .F., .F.,
 ( 4, 2, 4 ),
 ( 0.000000000000000000, 0.5000000000000000000, 1.000000000000000000 ),
 .UNSPECIFIED. ) ;
#27718 = CARTESIAN_POINT ( 'NONE',  ( -10.93634242917226373, -19.96742847112642849, -21.60398965136151972 ) ) ;
#27719 = EDGE_CURVE ( 'NONE', #6401, #29611, #1073, .T. ) ;
#27720 = DIRECTION ( 'NONE',  ( -0.000000000000000000, -0.000000000000000000, -1.000000000000000000 ) ) ;
#27721 = VECTOR ( 'NONE', #1783, 1000.000000000000000 ) ;
#27722 = CARTESIAN_POINT ( 'NONE',  ( -21.14746589409385535, -12.76649274373130183, -20.68958427074545980 ) ) ;
#27723 = CARTESIAN_POINT ( 'NONE',  ( -11.22534350456744612, -25.23047905509118394, -9.287595664362980230 ) ) ;
#27724 = CYLINDRICAL_SURFACE ( 'NONE', #31291, 6.000000000000001776 ) ;
#27725 = CARTESIAN_POINT ( 'NONE',  ( 11.87983786580489820, 16.84351847752386178, -28.12481558007895899 ) ) ;
#27727 = ADVANCED_FACE ( 'NONE', ( #4211 ), #31643, .F. ) ;
#27726 = ORIENTED_EDGE ( 'NONE', *, *, #13717, .T. ) ;
#27728 = CARTESIAN_POINT ( 'NONE',  ( 19.82805615916967312, 5.207665154685882314, -29.40699823107372524 ) ) ;
#27729 = DIRECTION ( 'NONE',  ( 0.9781476007338042455, -0.2079116908177663370, -0.000000000000000000 ) ) ;
#27730 = ADVANCED_FACE ( 'NONE', ( #17017 ), #28995, .F. ) ;
#27731 = CARTESIAN_POINT ( 'NONE',  ( -7.824485034907249670, 10.87986945260456295, 7.000000000000000000 ) ) ;
#27732 = CARTESIAN_POINT ( 'NONE',  ( 4.524139159579314118, 31.43208625488810171, 10.49999999999999822 ) ) ;
#27733 = ORIENTED_EDGE ( 'NONE', *, *, #29289, .T. ) ;
#27734 = CARTESIAN_POINT ( 'NONE',  ( -31.19464554439533899, -0.7868789741791578640, -7.795315093382260585 ) ) ;
#27735 = CARTESIAN_POINT ( 'NONE',  ( 21.28465047978626146, 0.7165814371454377607, -25.00808991143824755 ) ) ;
#27736 = EDGE_CURVE ( 'NONE', #4444, #27240, #16407, .T. ) ;
#27737 = DIRECTION ( 'NONE',  ( 1.000000000000000000, 0.000000000000000000, 0.000000000000000000 ) ) ;
#27738 = CARTESIAN_POINT ( 'NONE',  ( 21.12676075887526750, -20.25532016563445481, 20.50957957746029692 ) ) ;
#27739 = ORIENTED_EDGE ( 'NONE', *, *, #8420, .T. ) ;
#27740 = CARTESIAN_POINT ( 'NONE',  ( 22.45323650136968396, -2.382502413133517738, -20.55760979252983134 ) ) ;
#27741 = CARTESIAN_POINT ( 'NONE',  ( -6.064571727552472424, 31.45661825943146894, 12.00000000000000000 ) ) ;
#27742 = AXIS2_PLACEMENT_3D ( 'NONE', #31285, #18106, #9555 ) ;
#27743 = VECTOR ( 'NONE', #35685, 1000.000000000000000 ) ;
#27744 = ORIENTED_EDGE ( 'NONE', *, *, #13619, .T. ) ;
#27745 = EDGE_CURVE ( 'NONE', #3843, #31103, #29198, .T. ) ;
#27746 = CARTESIAN_POINT ( 'NONE',  ( -10.09922753093611192, -27.41777246569288451, -4.999999999999999112 ) ) ;
#27747 = AXIS2_PLACEMENT_3D ( 'NONE', #8864, #39930, #9463 ) ;
#27748 = EDGE_CURVE ( 'NONE', #19049, #26207, #32252, .T. ) ;
#27749 = EDGE_CURVE ( 'NONE', #9605, #35819, #5189, .T. ) ;
#27750 = CARTESIAN_POINT ( 'NONE',  ( -6.462764152204137247, 17.91932574235844555, 23.00000000000000000 ) ) ;
#27751 = DIRECTION ( 'NONE',  ( 0.000000000000000000, 0.000000000000000000, 1.000000000000000000 ) ) ;
#27752 = CARTESIAN_POINT ( 'NONE',  ( 0.8308715916267807033, 20.49243450554475743, -29.21251993523028290 ) ) ;
#27753 = CARTESIAN_POINT ( 'NONE',  ( 16.00000000000000000, 22.50000000000000711, 10.00000000000000000 ) ) ;
#27754 = CARTESIAN_POINT ( 'NONE',  ( 6.429307333185271034, 14.50146843380299977, 10.74999999999999289 ) ) ;
#27755 = DIRECTION ( 'NONE',  ( 1.000000000000000000, 0.000000000000000000, 0.000000000000000000 ) ) ;
#27756 = DIRECTION ( 'NONE',  ( 0.000000000000000000, 0.000000000000000000, 1.000000000000000000 ) ) ;
#27757 = DIRECTION ( 'NONE',  ( -0.000000000000000000, -0.000000000000000000, -1.000000000000000000 ) ) ;
#27758 = DIRECTION ( 'NONE',  ( 0.4067366430757884399, -0.9135454576426061957, 0.000000000000000000 ) ) ;
#27759 = CARTESIAN_POINT ( 'NONE',  ( 10.33186281181274424, 17.87145931443220093, -28.03536056408174915 ) ) ;
#27760 = DIRECTION ( 'NONE',  ( 0.000000000000000000, 0.000000000000000000, 1.000000000000000000 ) ) ;
#27761 = ORIENTED_EDGE ( 'NONE', *, *, #15860, .T. ) ;
#27763 = DIRECTION ( 'NONE',  ( 1.000000000000000000, 0.000000000000000000, 0.000000000000000000 ) ) ;
#27762 = CARTESIAN_POINT ( 'NONE',  ( -16.21686205092897026, 15.87015845977987638, -18.92977423509347190 ) ) ;
#27764 = DIRECTION ( 'NONE',  ( 0.000000000000000000, 0.000000000000000000, 1.000000000000000000 ) ) ;
#27765 = CARTESIAN_POINT ( 'NONE',  ( 9.504747149499191750, -18.16341882422712573, -30.00000000000000000 ) ) ;
#27766 = CARTESIAN_POINT ( 'NONE',  ( -15.20277289067466420, -19.27049939871586304, -20.06318638457704395 ) ) ;
#27767 = CARTESIAN_POINT ( 'NONE',  ( 13.76661467574959907, 23.40248112065832231, -14.47560752045290755 ) ) ;
#27768 = CARTESIAN_POINT ( 'NONE',  ( 13.76109791490951473, 23.41500128713417439, -14.47428817913493582 ) ) ;
#27769 = ORIENTED_EDGE ( 'NONE', *, *, #10345, .T. ) ;
#27770 = FACE_OUTER_BOUND ( 'NONE', #25011, .T. ) ;
#27771 = CARTESIAN_POINT ( 'NONE',  ( -15.41457889571365669, -26.69797501666770145, -5.946085984683254999 ) ) ;
#27772 = ADVANCED_FACE ( 'NONE', ( #34895 ), #1306, .T. ) ;
#27773 = CARTESIAN_POINT ( 'NONE',  ( -36.59387134601861646, -14.69446750445176342, 13.92931973827808712 ) ) ;
#27774 = AXIS2_PLACEMENT_3D ( 'NONE', #27386, #6051, #39777 ) ;
#27775 = EDGE_CURVE ( 'NONE', #2697, #33983, #16817, .T. ) ;
#27776 = AXIS2_PLACEMENT_3D ( 'NONE', #6975, #26075, #37867 ) ;
#27777 = CARTESIAN_POINT ( 'NONE',  ( -28.71250260137452059, -23.91295777942312739, -7.138176182773029232 ) ) ;
#27778 = CARTESIAN_POINT ( 'NONE',  ( -2.553198430222350712, -24.56346249274959348, -8.406762110482494776 ) ) ;
#27779 = CARTESIAN_POINT ( 'NONE',  ( 15.61108509054414917, 26.00910297926085235, -5.946291585397761814 ) ) ;
#27780 = EDGE_CURVE ( 'NONE', #33109, #4829, #3246, .T. ) ;
#27781 = CARTESIAN_POINT ( 'NONE',  ( 20.01029315168119282, 12.29792661527229569, -13.90631728972765124 ) ) ;
#27782 = DIRECTION ( 'NONE',  ( 0.000000000000000000, 0.000000000000000000, 1.000000000000000000 ) ) ;
#27783 = CARTESIAN_POINT ( 'NONE',  ( -4.379796608956421977, 30.71736661111763667, -14.76804172563591777 ) ) ;
#27784 = AXIS2_PLACEMENT_3D ( 'NONE', #33807, #21995, #21402 ) ;
#27785 = ORIENTED_EDGE ( 'NONE', *, *, #23586, .T. ) ;
#27786 = CARTESIAN_POINT ( 'NONE',  ( -34.83329005959444657, -6.589775719143758259, -5.448933541975200967 ) ) ;
#27787 = AXIS2_PLACEMENT_3D ( 'NONE', #34730, #20098, #16443 ) ;
#27788 = CARTESIAN_POINT ( 'NONE',  ( -17.89938016360686390, 22.15910768086194693, 14.53008259255394208 ) ) ;
#27789 = ORIENTED_EDGE ( 'NONE', *, *, #18881, .T. ) ;
#27790 = DIRECTION ( 'NONE',  ( 0.000000000000000000, 0.000000000000000000, 1.000000000000000000 ) ) ;
#27791 = CARTESIAN_POINT ( 'NONE',  ( 13.48130249190479368, 27.93180293473185927, 10.49999999999999822 ) ) ;
#27792 = CARTESIAN_POINT ( 'NONE',  ( -25.00566865627084923, 0.7636625105755581178, -17.47633105975672052 ) ) ;
#27793 = CARTESIAN_POINT ( 'NONE',  ( 30.70933288805361983, -12.32817769576170441, -12.91955702887979562 ) ) ;
#27794 = ORIENTED_EDGE ( 'NONE', *, *, #39941, .T. ) ;
#27795 = DIRECTION ( 'NONE',  ( 0.000000000000000000, 0.000000000000000000, 1.000000000000000000 ) ) ;
#27796 = VERTEX_POINT ( 'NONE', #32862 ) ;
#27797 = DIRECTION ( 'NONE',  ( 0.7431448254773954654, 0.6691306063588569053, -0.000000000000000000 ) ) ;
#27798 = CARTESIAN_POINT ( 'NONE',  ( 30.33922525720639030, 6.243664897696307392, 11.00000000000000000 ) ) ;
#27799 = EDGE_CURVE ( 'NONE', #37025, #14056, #2378, .T. ) ;
#27800 = AXIS2_PLACEMENT_3D ( 'NONE', #8707, #31235, #18058 ) ;
#27801 = VECTOR ( 'NONE', #13637, 1000.000000000000114 ) ;
#27802 = CYLINDRICAL_SURFACE ( 'NONE', #18165, 17.00000000000000711 ) ;
#27803 = ORIENTED_EDGE ( 'NONE', *, *, #12564, .T. ) ;
#27804 = CARTESIAN_POINT ( 'NONE',  ( -1.923949180127531466, 38.42603324025853340, -5.435599845266582797 ) ) ;
#27805 = DIRECTION ( 'NONE',  ( -1.000000000000000000, 0.000000000000000000, 0.000000000000000000 ) ) ;
#27806 = CARTESIAN_POINT ( 'NONE',  ( -6.811226782241547539, 35.33967249274200384, 11.00000000000000000 ) ) ;
#27807 = VECTOR ( 'NONE', #24550, 1000.000000000000000 ) ;
#27808 = PLANE ( 'NONE',  #10456 ) ;
#27809 = CARTESIAN_POINT ( 'NONE',  ( 27.76036423759017424, -22.74041533840534157, -9.756283338662747440 ) ) ;
#27810 = CARTESIAN_POINT ( 'NONE',  ( 16.30176999113392355, 13.74177821074143147, -23.26433688756818086 ) ) ;
#27811 = AXIS2_PLACEMENT_3D ( 'NONE', #25134, #27790, #40174 ) ;
#27812 = CARTESIAN_POINT ( 'NONE',  ( 12.46298602409325618, 29.89662867798026369, -10.40118216561738151 ) ) ;
#27813 = VERTEX_POINT ( 'NONE', #14767 ) ;
#27814 = CARTESIAN_POINT ( 'NONE',  ( -20.71763460597477291, 13.68537009249746461, -5.482835118453670553 ) ) ;
#27815 = CARTESIAN_POINT ( 'NONE',  ( -3.456468065140151591, 26.15323006594331545, 23.00000000000000000 ) ) ;
#27816 = CARTESIAN_POINT ( 'NONE',  ( 13.54728634190223779, -23.64058435204617226, -14.45986489698174182 ) ) ;
#27817 = CARTESIAN_POINT ( 'NONE',  ( -1.000000000000000000, 37.00000000000000711, 9.500000000000000000 ) ) ;
#27818 = CARTESIAN_POINT ( 'NONE',  ( 35.36940577612500647, -20.42053594592275800, -14.51648065752882566 ) ) ;
#27819 = CARTESIAN_POINT ( 'NONE',  ( 7.935770203493858865, 22.34671014717335780, 6.000000000000000000 ) ) ;
#27820 = CARTESIAN_POINT ( 'NONE',  ( -12.63876190530728216, 21.07525087859380974, -18.44901738601522467 ) ) ;
#27821 = CARTESIAN_POINT ( 'NONE',  ( -19.05194404211813008, -21.38509357595906124, -15.91629285646954273 ) ) ;
#27822 = CARTESIAN_POINT ( 'NONE',  ( 10.72379324094551833, -25.60257746891399577, -6.426360612472806544 ) ) ;
#27823 = ADVANCED_FACE ( 'NONE', ( #26558 ), #37246, .T. ) ;
#27824 = DIRECTION ( 'NONE',  ( 0.9510565162951544194, 0.3090169943749451198, 0.000000000000000000 ) ) ;
#27825 = ORIENTED_EDGE ( 'NONE', *, *, #37697, .T. ) ;
#27826 = CARTESIAN_POINT ( 'NONE',  ( -6.589341983113207846, 19.77883683989693253, -27.14241267237451538 ) ) ;
#27827 = CARTESIAN_POINT ( 'NONE',  ( 0.5000000000000000000, 37.33905845025569903, 10.87262190630138292 ) ) ;
#27828 = LINE ( 'NONE', #19084, #26298 ) ;
#27829 = AXIS2_PLACEMENT_3D ( 'NONE', #27819, #30873, #21915 ) ;
#27830 = AXIS2_PLACEMENT_3D ( 'NONE', #8474, #20874, #24704 ) ;
#27831 = CARTESIAN_POINT ( 'NONE',  ( 7.659620408498160060, 26.92228390473674793, 7.000000000000000000 ) ) ;
#27832 = ORIENTED_EDGE ( 'NONE', *, *, #20816, .F. ) ;
#27833 = CARTESIAN_POINT ( 'NONE',  ( 20.61009167187485147, 0.8554190281657136907, -28.07775950742859550 ) ) ;
#27834 = DIRECTION ( 'NONE',  ( 1.000000000000000000, 0.000000000000000000, 0.000000000000000000 ) ) ;
#27835 = DIRECTION ( 'NONE',  ( 1.000000000000000000, 0.000000000000000000, 0.000000000000000000 ) ) ;
#27836 = AXIS2_PLACEMENT_3D ( 'NONE', #17325, #29700, #1881 ) ;
#27837 = B_SPLINE_SURFACE_WITH_KNOTS ( 'NONE', 1, 3, ( 
 ( #716, #38083, #37691, #4156, #10256, #37883, #19807, #22436, #3560, #32199 ),
 ( #29150, #1318, #23049, #28338, #520, #13701, #38489, #10665, #34842, #6993 ) ),
 .UNSPECIFIED., .F., .F., .F.,
 ( 2, 2 ),
 ( 4, 2, 2, 2, 4 ),
 ( 0.000000000000000000, 1.000000000000000000 ),
 ( 4.145433333912467155, 4.538132415611192627, 4.930831497309917211, 5.323530579008641794, 5.716229660707366378 ),
 .UNSPECIFIED. ) ;
#27838 = ORIENTED_EDGE ( 'NONE', *, *, #9512, .T. ) ;
#27839 = CARTESIAN_POINT ( 'NONE',  ( -29.94841971816240545, 0.07655252488241326425, -9.239200560549260643 ) ) ;
#27840 = DIRECTION ( 'NONE',  ( -0.000000000000000000, 0.000000000000000000, -1.000000000000000000 ) ) ;
#27841 = ORIENTED_EDGE ( 'NONE', *, *, #6521, .T. ) ;
#27842 = CARTESIAN_POINT ( 'NONE',  ( 34.50778285978141469, -6.214036658931777701, -6.771707614261031516 ) ) ;
#27843 = VERTEX_POINT ( 'NONE', #27156 ) ;
#27844 = CARTESIAN_POINT ( 'NONE',  ( -13.54523449123470691, 33.99770581697566740, 13.32518128616629483 ) ) ;
#27845 = CARTESIAN_POINT ( 'NONE',  ( -17.00801676778996097, -20.85310720624647374, 20.25080042701566541 ) ) ;
#27846 = CARTESIAN_POINT ( 'NONE',  ( -0.6897330713185921836, 37.48434185086841808, 7.485646746502371940 ) ) ;
#27847 = CARTESIAN_POINT ( 'NONE',  ( -5.145977874761546111, 31.04572515097865804, 20.25080042701513960 ) ) ;
#27848 = DIRECTION ( 'NONE',  ( -0.000000000000000000, 0.000000000000000000, 1.000000000000000000 ) ) ;
#27849 = VERTEX_POINT ( 'NONE', #30205 ) ;
#27850 = CARTESIAN_POINT ( 'NONE',  ( 0.000000000000000000, 22.50000000000000355, 13.00000000000000178 ) ) ;
#27851 = EDGE_CURVE ( 'NONE', #39330, #33798, #10925, .T. ) ;
#27852 = CARTESIAN_POINT ( 'NONE',  ( -10.21799113078971466, 32.82168114676807136, 10.66666666666666252 ) ) ;
#27853 = CARTESIAN_POINT ( 'NONE',  ( 5.082600654608392610, 21.41965916404854298, 6.000000000000000000 ) ) ;
#27854 = DIRECTION ( 'NONE',  ( 0.000000000000000000, 0.000000000000000000, 1.000000000000000000 ) ) ;
#27856 = VECTOR ( 'NONE', #20423, 1000.000000000000000 ) ;
#27855 = CARTESIAN_POINT ( 'NONE',  ( 8.872206882450816678, 34.45812223078402781, -8.912361989433076559 ) ) ;
#27857 = CARTESIAN_POINT ( 'NONE',  ( 3.607749162633204332, 7.931741834401770497, 10.49999999999999822 ) ) ;
#27858 = ADVANCED_FACE ( 'NONE', ( #39541 ), #8059, .F. ) ;
#27859 = CARTESIAN_POINT ( 'NONE',  ( 11.00000970693004554, -17.98380166451403639, -26.10610249844645026 ) ) ;
#27860 = PLANE ( 'NONE',  #30119 ) ;
#27861 = AXIS2_PLACEMENT_3D ( 'NONE', #29447, #26197, #1626 ) ;
#27862 = DIRECTION ( 'NONE',  ( 1.000000000000000000, 0.000000000000000000, 0.000000000000000000 ) ) ;
#27863 = DIRECTION ( 'NONE',  ( 1.000000000000000000, 0.000000000000000000, 0.000000000000000000 ) ) ;
#27864 = ORIENTED_EDGE ( 'NONE', *, *, #20945, .F. ) ;
#27865 = CARTESIAN_POINT ( 'NONE',  ( -11.17092706714288397, 17.24184491651588758, -28.71381065368748509 ) ) ;
#27866 = CARTESIAN_POINT ( 'NONE',  ( -26.47427689499508574, -23.88731992525624293, 17.92354375535214572 ) ) ;
#27867 = CARTESIAN_POINT ( 'NONE',  ( 9.540210792438220011, -18.51136029728062127, -26.84305259188365156 ) ) ;
#27868 = DIRECTION ( 'NONE',  ( 0.000000000000000000, 0.000000000000000000, 1.000000000000000000 ) ) ;
#27869 = ORIENTED_EDGE ( 'NONE', *, *, #5799, .T. ) ;
#27870 = ORIENTED_EDGE ( 'NONE', *, *, #13748, .T. ) ;
#27871 = CARTESIAN_POINT ( 'NONE',  ( -9.821329010893958156, 19.10955050348507456, -24.81548820641463848 ) ) ;
#27872 = CARTESIAN_POINT ( 'NONE',  ( -15.25086691884292911, -21.72593466508776316, -17.12598327003187393 ) ) ;
#27873 = FACE_BOUND ( 'NONE', #13232, .T. ) ;
#27874 = EDGE_LOOP ( 'NONE', ( #4240, #3916, #13541, #37088 ) ) ;
#27875 = CARTESIAN_POINT ( 'NONE',  ( -25.13972300716358532, -7.830238314601142058, -18.75331848047975569 ) ) ;
#27876 = CARTESIAN_POINT ( 'NONE',  ( -10.32636287134091546, -19.63648956442319005, -22.76047509490289400 ) ) ;
#27877 = CARTESIAN_POINT ( 'NONE',  ( 0.4999999999999995559, 37.00000000000000711, 11.00000000000000000 ) ) ;
#27878 = ORIENTED_EDGE ( 'NONE', *, *, #2893, .F. ) ;
#27879 = CARTESIAN_POINT ( 'NONE',  ( 27.56524107966918535, 0.4215817824878217990, -13.52655066544985729 ) ) ;
#27880 = DIRECTION ( 'NONE',  ( 1.000000000000000000, 0.000000000000000000, 0.000000000000000000 ) ) ;
#27881 = DIRECTION ( 'NONE',  ( 0.07391278520354631343, -0.7032331762534066444, 0.7071067811865472397 ) ) ;
#27882 = EDGE_CURVE ( 'NONE', #23702, #4851, #29861, .T. ) ;
#27883 = ORIENTED_EDGE ( 'NONE', *, *, #6542, .F. ) ;
#27884 = CARTESIAN_POINT ( 'NONE',  ( -26.53893653578703038, 0.2251345205519453829, -15.44439873174107980 ) ) ;
#27885 = ORIENTED_EDGE ( 'NONE', *, *, #5019, .T. ) ;
#27886 = CARTESIAN_POINT ( 'NONE',  ( 21.40780153129764685, -0.3772474073816712292, -24.88848197966343889 ) ) ;
#27887 = VECTOR ( 'NONE', #34206, 1000.000000000000000 ) ;
#27888 = CARTESIAN_POINT ( 'NONE',  ( -7.961096663582920563, -18.90310754077565747, -30.00000000000000355 ) ) ;
#27889 = CARTESIAN_POINT ( 'NONE',  ( 26.16909114927596747, -23.33537003677559696, 18.42518152272070253 ) ) ;
#27890 = ORIENTED_EDGE ( 'NONE', *, *, #13414, .F. ) ;
#27891 = CARTESIAN_POINT ( 'NONE',  ( -23.15794617311298254, 4.315003200217033985, -17.77638817182914721 ) ) ;
#27892 = AXIS2_PLACEMENT_3D ( 'NONE', #13553, #13148, #25539 ) ;
#27893 = DIRECTION ( 'NONE',  ( -0.000000000000000000, -0.000000000000000000, 1.000000000000000000 ) ) ;
#27894 = CARTESIAN_POINT ( 'NONE',  ( 0.000000000000000000, 22.50000000000000355, 10.00000000000000000 ) ) ;
#27895 = LINE ( 'NONE', #9415, #26542 ) ;
#27896 = LINE ( 'NONE', #9016, #34437 ) ;
#27897 = EDGE_CURVE ( 'NONE', #32004, #29377, #16914, .T. ) ;
#27898 = FACE_BOUND ( 'NONE', #8044, .T. ) ;
#27899 = CARTESIAN_POINT ( 'NONE',  ( 28.74551992320437321, 4.923758765711149010, 12.14047268032575211 ) ) ;
#27900 = CARTESIAN_POINT ( 'NONE',  ( -19.59498488650715231, 6.415608140812385507, -27.69164703474022815 ) ) ;
#27901 = DIRECTION ( 'NONE',  ( 0.9945218953682730678, -0.1045284632676570929, 0.000000000000000000 ) ) ;
#27902 = ADVANCED_FACE ( 'NONE', ( #23311 ), #35705, .F. ) ;
#27903 = DIRECTION ( 'NONE',  ( 0.000000000000000000, 0.000000000000000000, 1.000000000000000000 ) ) ;
#27904 = CARTESIAN_POINT ( 'NONE',  ( 13.74558791142738734, -15.22183123319549125, -30.00000000000000355 ) ) ;
#27905 = B_SPLINE_CURVE_WITH_KNOTS ( 'NONE', 3,
 ( #19621, #10896, #38512, #23279, #19221, #32015 ),
 .UNSPECIFIED., .F., .F.,
 ( 4, 2, 4 ),
 ( 0.000000000000000000, 0.5000000000000000000, 1.000000000000000000 ),
 .UNSPECIFIED. ) ;
#27906 = CARTESIAN_POINT ( 'NONE',  ( -7.530592408761007661, 11.28437794979203090, 10.50000000000000000 ) ) ;
#27907 = CARTESIAN_POINT ( 'NONE',  ( 13.37007945456113411, 23.06071637790597251, -15.42265832664474878 ) ) ;
#27908 = ORIENTED_EDGE ( 'NONE', *, *, #36353, .T. ) ;
#27909 = CARTESIAN_POINT ( 'NONE',  ( -15.75218124485975757, 24.12653032028219258, -8.789014821092310470 ) ) ;
#27910 = CARTESIAN_POINT ( 'NONE',  ( -26.24102572421938362, -17.42682220599465737, 20.50957957746029692 ) ) ;
#27911 = CARTESIAN_POINT ( 'NONE',  ( 7.111215932167701759, 17.81698729810774751, 9.000000000000001776 ) ) ;
#27912 = CARTESIAN_POINT ( 'NONE',  ( 11.01299302568612859, 17.29057472414998742, -29.34897105029772746 ) ) ;
#27913 = ORIENTED_EDGE ( 'NONE', *, *, #11994, .F. ) ;
#27914 = PLANE ( 'NONE',  #25489 ) ;
#27915 = VECTOR ( 'NONE', #10869, 1000.000000000000000 ) ;
#27916 = ORIENTED_EDGE ( 'NONE', *, *, #36427, .F. ) ;
#27918 = DIRECTION ( 'NONE',  ( 0.000000000000000000, 0.000000000000000000, 1.000000000000000000 ) ) ;
#27917 = CARTESIAN_POINT ( 'NONE',  ( -14.44494323251225865, 25.21727681637074170, -11.58053765247176514 ) ) ;
#27919 = CARTESIAN_POINT ( 'NONE',  ( -15.18541056174788650, -26.03681117208375539, -9.228366842610254750 ) ) ;
#27920 = DIRECTION ( 'NONE',  ( 0.000000000000000000, 0.000000000000000000, 1.000000000000000000 ) ) ;
#27921 = VERTEX_POINT ( 'NONE', #17828 ) ;
#27922 = CARTESIAN_POINT ( 'NONE',  ( -18.51744266559586904, -9.015907171310754364, -28.44847492086340424 ) ) ;
#27923 = CARTESIAN_POINT ( 'NONE',  ( -8.819735198518117159, -18.71328657623911340, -27.50136144446895514 ) ) ;
#27924 = CARTESIAN_POINT ( 'NONE',  ( 10.06946225350410984, 32.23940090176269990, 7.499999999999997335 ) ) ;
#27925 = CARTESIAN_POINT ( 'NONE',  ( 16.00132168787127540, 24.22562490985221118, -7.367879038845686068 ) ) ;
#27926 = ORIENTED_EDGE ( 'NONE', *, *, #1203, .F. ) ;
#27927 = CARTESIAN_POINT ( 'NONE',  ( 26.24647792831409632, 4.660060628212018941, -8.835378462270252697 ) ) ;
#27928 = DIRECTION ( 'NONE',  ( 0.000000000000000000, 0.000000000000000000, -1.000000000000000000 ) ) ;
#27929 = EDGE_CURVE ( 'NONE', #17936, #17600, #12348, .T. ) ;
#27930 = CYLINDRICAL_SURFACE ( 'NONE', #12773, 0.4999999999999988898 ) ;
#27931 = EDGE_CURVE ( 'NONE', #28556, #7248, #27255, .T. ) ;
#27932 = DIRECTION ( 'NONE',  ( 1.000000000000000000, 0.000000000000000000, 0.000000000000000000 ) ) ;
#27933 = ORIENTED_EDGE ( 'NONE', *, *, #22920, .T. ) ;
#27934 = CARTESIAN_POINT ( 'NONE',  ( -29.68641950918352990, -0.3073957355675461245, -10.62315473450874315 ) ) ;
#27935 = CARTESIAN_POINT ( 'NONE',  ( 26.05478663030475062, 0.0009985127382727311540, -16.40327240360535299 ) ) ;
#27936 = AXIS2_PLACEMENT_3D ( 'NONE', #5562, #21404, #12456 ) ;
#27937 = CARTESIAN_POINT ( 'NONE',  ( -4.984135866956333594, 36.15314577889358105, 10.49999999999999822 ) ) ;
#27938 = CARTESIAN_POINT ( 'NONE',  ( 25.62037635619481790, -16.85925998830611761, 20.69868183039799803 ) ) ;
#27939 = ORIENTED_EDGE ( 'NONE', *, *, #17749, .F. ) ;
#27940 = DIRECTION ( 'NONE',  ( -0.000000000000000000, -0.000000000000000000, -1.000000000000000000 ) ) ;
#27941 = PLANE ( 'NONE',  #30345 ) ;
#27942 = EDGE_LOOP ( 'NONE', ( #12211, #2845, #15098, #39385 ) ) ;
#27943 = CIRCLE ( 'NONE', #21483, 0.5000000000000007772 ) ;
#27944 = DIRECTION ( 'NONE',  ( 0.5877852522924690293, -0.8090169943749503378, 0.000000000000000000 ) ) ;
#27945 = EDGE_CURVE ( 'NONE', #36183, #13580, #11716, .T. ) ;
#27946 = CARTESIAN_POINT ( 'NONE',  ( -22.48079666814428634, 18.61591633949074520, 22.99999999999999645 ) ) ;
#27947 = DIRECTION ( 'NONE',  ( 1.000000000000000000, 0.000000000000000000, 0.000000000000000000 ) ) ;
#27948 = CARTESIAN_POINT ( 'NONE',  ( 2.699333757401777500, 37.52124286414814236, -7.975407974893957253 ) ) ;
#27949 = CARTESIAN_POINT ( 'NONE',  ( 7.126083911573384277, 10.99048532364570185, 10.00000000000000000 ) ) ;
#27950 = DIRECTION ( 'NONE',  ( -0.000000000000000000, -0.000000000000000000, -1.000000000000000000 ) ) ;
#27951 = CARTESIAN_POINT ( 'NONE',  ( -1.485571585149857210, -11.24999999999982236, 3.000000000000000000 ) ) ;
#27952 = DIRECTION ( 'NONE',  ( 0.000000000000000000, 0.000000000000000000, 1.000000000000000000 ) ) ;
#27953 = CARTESIAN_POINT ( 'NONE',  ( 11.54666566735224364, 32.07468077621332725, 7.499999999999997335 ) ) ;
#27954 = DIRECTION ( 'NONE',  ( 0.000000000000000000, 0.000000000000000000, 1.000000000000000000 ) ) ;
#27955 = CARTESIAN_POINT ( 'NONE',  ( 11.81616528917939668, 21.22289557514309877, -19.38120235366460875 ) ) ;
#27956 = DIRECTION ( 'NONE',  ( 0.3090169943749560000, 0.9510565162951507556, 0.000000000000000000 ) ) ;
#27957 = ORIENTED_EDGE ( 'NONE', *, *, #8503, .T. ) ;
#27958 = AXIS2_PLACEMENT_3D ( 'NONE', #30708, #5716, #8973 ) ;
#27960 = DIRECTION ( 'NONE',  ( 0.5877852522924690293, -0.8090169943749503378, 0.000000000000000000 ) ) ;
#27959 = CARTESIAN_POINT ( 'NONE',  ( -18.50828174693830519, 17.38258355848637393, -8.870643964797142900 ) ) ;
#27961 = CARTESIAN_POINT ( 'NONE',  ( 13.10100158617407295, 15.51348347675824435, 10.87262190629279779 ) ) ;
#27962 = AXIS2_PLACEMENT_3D ( 'NONE', #14051, #38842, #23403 ) ;
#27963 = CARTESIAN_POINT ( 'NONE',  ( 9.522022774849094873, -18.20502493181615122, -28.70691128024250105 ) ) ;
#27964 = CARTESIAN_POINT ( 'NONE',  ( -12.53503680232439699, -17.06533640674901164, -25.95590166166768853 ) ) ;
#27965 = CARTESIAN_POINT ( 'NONE',  ( 28.78471548569376282, -2.122417091767359931, 18.87996532025784546 ) ) ;
#27966 = CARTESIAN_POINT ( 'NONE',  ( 10.97317656914242967, 17.31587133052951089, -30.00000000000000000 ) ) ;
#27967 = ORIENTED_EDGE ( 'NONE', *, *, #5399, .F. ) ;
#27968 = CARTESIAN_POINT ( 'NONE',  ( -10.80698216227225394, 13.84996144622306247, 6.000000000000000000 ) ) ;
#27969 = CARTESIAN_POINT ( 'NONE',  ( -11.81623611950272412, -21.49189391620961942, -18.46105202309505344 ) ) ;
#27970 = CARTESIAN_POINT ( 'NONE',  ( -22.57842393431380756, -28.22498519091902125, 14.53008259253967971 ) ) ;
#27971 = CARTESIAN_POINT ( 'NONE',  ( -31.45852298323876539, -21.70319895717350533, -6.278571233013221509 ) ) ;
#27972 = CARTESIAN_POINT ( 'NONE',  ( -0.3222516639411605599, -22.43452379100889615, -18.01744884572263672 ) ) ;
#27973 = CARTESIAN_POINT ( 'NONE',  ( 15.11639032187935072, 25.24504664587892222, -9.717601439789641304 ) ) ;
#27974 = CARTESIAN_POINT ( 'NONE',  ( 21.63149483547664076, 10.84510153107085095, -10.88148262729828453 ) ) ;
#27975 = CARTESIAN_POINT ( 'NONE',  ( -9.197066986886744289, 11.25907462514039814, 10.66666666666666785 ) ) ;
#27976 = CIRCLE ( 'NONE', #20861, 1.000000000000000000 ) ;
#27977 = CARTESIAN_POINT ( 'NONE',  ( -4.212426069905327530, 37.97930161814787198, -4.999999999999994671 ) ) ;
#27978 = ORIENTED_EDGE ( 'NONE', *, *, #34375, .T. ) ;
#27979 = CARTESIAN_POINT ( 'NONE',  ( -29.56208081133425836, -4.613024107137377428, -14.07453195671733504 ) ) ;
#27980 = ADVANCED_FACE ( 'NONE', ( #1778 ), #15616, .T. ) ;
#27981 = CARTESIAN_POINT ( 'NONE',  ( -14.97058623677449773, 26.66112013779128986, 16.87380292611441490 ) ) ;
#27982 = EDGE_LOOP ( 'NONE', ( #30655, #36716, #34747, #8415 ) ) ;
#27983 = DIRECTION ( 'NONE',  ( 0.000000000000000000, 0.000000000000000000, 1.000000000000000000 ) ) ;
#27984 = CARTESIAN_POINT ( 'NONE',  ( -6.282361020112263716, 14.70372268239681190, 10.50000000000000533 ) ) ;
#27985 = CARTESIAN_POINT ( 'NONE',  ( -23.11816775549578651, 1.104452855686005375, -20.60762089766639704 ) ) ;
#27986 = CARTESIAN_POINT ( 'NONE',  ( 22.31642213958092924, -7.486323157245182713, -21.96314972916734831 ) ) ;
#27987 = CARTESIAN_POINT ( 'NONE',  ( 32.43957513061237563, -23.09559191376027343, 13.92931973827834113 ) ) ;
#27988 = VECTOR ( 'NONE', #24955, 1000.000000000000114 ) ;
#27989 = AXIS2_PLACEMENT_3D ( 'NONE', #19101, #20311, #35546 ) ;
#27990 = EDGE_LOOP ( 'NONE', ( #16574, #23197, #11877, #37542, #8954 ) ) ;
#27991 = FACE_OUTER_BOUND ( 'NONE', #20387, .T. ) ;
#27992 = ORIENTED_EDGE ( 'NONE', *, *, #33340, .F. ) ;
#27993 = FACE_OUTER_BOUND ( 'NONE', #11558, .T. ) ;
#27994 = CARTESIAN_POINT ( 'NONE',  ( 8.315274455032099610, 10.01576150750513072, 7.000000000000000000 ) ) ;
#27995 = EDGE_CURVE ( 'NONE', #11401, #1059, #12700, .T. ) ;
#27996 = CARTESIAN_POINT ( 'NONE',  ( 0.5000000000000012212, 31.00000000000000355, 9.000000000000001776 ) ) ;
#27997 = ORIENTED_EDGE ( 'NONE', *, *, #5416, .F. ) ;
#27998 = EDGE_CURVE ( 'NONE', #31785, #31854, #12507, .T. ) ;
#27999 = CARTESIAN_POINT ( 'NONE',  ( -2.493496152838000857, 22.65825999365475951, -23.01938064764903302 ) ) ;
#28000 = CARTESIAN_POINT ( 'NONE',  ( -4.577399223880545875, 35.23960032125098252, 10.50000000000000000 ) ) ;
#28001 = CARTESIAN_POINT ( 'NONE',  ( -0.6237384431625470071, 19.56555719779890978, 13.00000000000000178 ) ) ;
#28002 = CIRCLE ( 'NONE', #10492, 1.000000000000000888 ) ;
#28003 = LINE ( 'NONE', #31255, #17625 ) ;
#28004 = DIRECTION ( 'NONE',  ( 0.6691306063588671194, 0.7431448254773863615, -0.000000000000000000 ) ) ;
#28005 = CARTESIAN_POINT ( 'NONE',  ( 9.081295331449249275, 19.56124383720467108, -24.72641353342787340 ) ) ;
#28006 = ORIENTED_EDGE ( 'NONE', *, *, #12854, .T. ) ;
#28007 = EDGE_CURVE ( 'NONE', #31457, #37999, #22719, .T. ) ;
#28008 = CARTESIAN_POINT ( 'NONE',  ( -20.94101416334770249, 12.52813585024752463, -9.396077220118929318 ) ) ;
#28009 = CARTESIAN_POINT ( 'NONE',  ( -14.78578095943786153, 19.97317811133652654, 7.339470489435494294 ) ) ;
#28010 = CARTESIAN_POINT ( 'NONE',  ( 9.808763409072279060, -18.38515136357905888, -26.82030050216148709 ) ) ;
#28011 = CARTESIAN_POINT ( 'NONE',  ( -5.473344025737326035, 14.11593743010433677, 10.50000000000000178 ) ) ;
#28012 = CARTESIAN_POINT ( 'NONE',  ( 11.06964067281062825, 17.65134693061273907, -26.82519749397791031 ) ) ;
#28013 = CARTESIAN_POINT ( 'NONE',  ( -20.55563217186186620, -29.52600041847739831, -13.99876745781540777 ) ) ;
#28014 = LINE ( 'NONE', #24969, #30424 ) ;
#28015 = CARTESIAN_POINT ( 'NONE',  ( -12.91061715790210407, 21.68268698219946344, -17.43355264670666926 ) ) ;
#28016 = CIRCLE ( 'NONE', #31900, 1.000000000000000000 ) ;
#28017 = CARTESIAN_POINT ( 'NONE',  ( -14.77834355681148715, -14.73733460233652437, -27.08378865361848042 ) ) ;
#28018 = CARTESIAN_POINT ( 'NONE',  ( 8.691294114719063657, -18.77241989521133902, -27.50980908539149183 ) ) ;
#28019 = CARTESIAN_POINT ( 'NONE',  ( 15.14522103274069131, 25.99557503532075842, -8.769033976177988521 ) ) ;
#28020 = CARTESIAN_POINT ( 'NONE',  ( 28.45022969918851885, -19.27983063241365969, -11.98101230249146099 ) ) ;
#28021 = LINE ( 'NONE', #28219, #16384 ) ;
#28022 = VERTEX_POINT ( 'NONE', #21648 ) ;
#28023 = CARTESIAN_POINT ( 'NONE',  ( -6.508188039552276649, 19.52556562270282470, -28.54081524349888355 ) ) ;
#28024 = ADVANCED_FACE ( 'NONE', ( #31196 ), #34253, .T. ) ;
#28025 = CARTESIAN_POINT ( 'NONE',  ( 14.23945615837883949, -31.58416516429907972, 0.000000000000000000 ) ) ;
#28026 = CARTESIAN_POINT ( 'NONE',  ( -13.05736835487441994, 16.11602540378456183, 10.49999999999999822 ) ) ;
#28027 = ADVANCED_FACE ( 'NONE', ( #34052 ), #6210, .F. ) ;
#28028 = DIRECTION ( 'NONE',  ( 0.8660254037844364872, -0.5000000000000038858, 0.000000000000000000 ) ) ;
#28029 = ORIENTED_EDGE ( 'NONE', *, *, #7716, .F. ) ;
#28030 = CARTESIAN_POINT ( 'NONE',  ( 20.48067366615298468, 0.8901913013804809705, -29.34893421961264082 ) ) ;
#28031 = CARTESIAN_POINT ( 'NONE',  ( 14.46401681939182993, 26.47472063362052808, 7.485699520496980952 ) ) ;
#28032 = AXIS2_PLACEMENT_3D ( 'NONE', #5051, #32287, #4448 ) ;
#28033 = CARTESIAN_POINT ( 'NONE',  ( 3.607749162633204332, 7.931741834401770497, 11.00000000000000000 ) ) ;
#28034 = ORIENTED_EDGE ( 'NONE', *, *, #20915, .F. ) ;
#28035 = CARTESIAN_POINT ( 'NONE',  ( -20.48102978849703604, 0.8817738089609834518, -30.00000000000000000 ) ) ;
#28036 = DIRECTION ( 'NONE',  ( 1.000000000000000000, 0.000000000000000000, 0.000000000000000000 ) ) ;
#28037 = ORIENTED_EDGE ( 'NONE', *, *, #27299, .T. ) ;
#28038 = CARTESIAN_POINT ( 'NONE',  ( 34.12941852828814149, -7.118180197318186408, -8.515197907227713969 ) ) ;
#28039 = VERTEX_POINT ( 'NONE', #31003 ) ;
#28040 = CARTESIAN_POINT ( 'NONE',  ( 7.565838454495062315, 38.87983827381772528, 12.14047268033080407 ) ) ;
#28041 = LINE ( 'NONE', #3658, #4758 ) ;
#28042 = LINE ( 'NONE', #28441, #37709 ) ;
#28043 = EDGE_CURVE ( 'NONE', #7967, #40046, #26614, .T. ) ;
#28044 = CARTESIAN_POINT ( 'NONE',  ( -2.905187527479620613, 31.12430299512148935, 20.50957957746028626 ) ) ;
#28045 = CARTESIAN_POINT ( 'NONE',  ( -2.568190708544554557, 12.82247983807085134, 10.50000000000000533 ) ) ;
#28046 = VERTEX_POINT ( 'NONE', #18811 ) ;
#28047 = ADVANCED_FACE ( 'NONE', ( #3362 ), #15754, .F. ) ;
#28048 = DIRECTION ( 'NONE',  ( 0.000000000000000000, 0.000000000000000000, 1.000000000000000000 ) ) ;
#28049 = CARTESIAN_POINT ( 'NONE',  ( -14.87461375695690791, 14.12245287598898535, -30.00000000000001776 ) ) ;
#28050 = CARTESIAN_POINT ( 'NONE',  ( 12.51556656179726801, 14.23165457969784597, 7.381627713044569106 ) ) ;
#28051 = CARTESIAN_POINT ( 'NONE',  ( -7.096882951594430722, 29.56287847632736288, 10.49999999999999822 ) ) ;
#28052 = CARTESIAN_POINT ( 'NONE',  ( 4.547395191718751839, 20.23153756940337900, -27.77134476049675627 ) ) ;
#28053 = VECTOR ( 'NONE', #23992, 999.9999999999998863 ) ;
#28054 = CARTESIAN_POINT ( 'NONE',  ( 11.21391615930829211, -18.27285559791526381, -24.86675532714961534 ) ) ;
#28055 = DIRECTION ( 'NONE',  ( 0.8660254037844363761, -0.5000000000000039968, -0.000000000000000000 ) ) ;
#28056 = B_SPLINE_CURVE_WITH_KNOTS ( 'NONE', 3,
 ( #15786, #27975, #31620, #150 ),
 .UNSPECIFIED., .F., .F.,
 ( 4, 4 ),
 ( 0.000000000000000000, 1.000000000000000000 ),
 .UNSPECIFIED. ) ;
#28057 = FACE_OUTER_BOUND ( 'NONE', #964, .T. ) ;
#28058 = ORIENTED_EDGE ( 'NONE', *, *, #16400, .F. ) ;
#28059 = CARTESIAN_POINT ( 'NONE',  ( -15.43019833371434579, 26.73233873233005653, -5.474191317994603345 ) ) ;
#28060 = VECTOR ( 'NONE', #4951, 1000.000000000000000 ) ;
#28061 = CARTESIAN_POINT ( 'NONE',  ( -15.89892447185300917, -25.15199583021655272, 17.92354375535250810 ) ) ;
#28062 = CARTESIAN_POINT ( 'NONE',  ( 10.74482040370065228, -20.01237387469337392, -21.62860023531220577 ) ) ;
#28063 = DIRECTION ( 'NONE',  ( -0.2079116908177532363, 0.9781476007338070211, 0.000000000000000000 ) ) ;
#28064 = VERTEX_POINT ( 'NONE', #36704 ) ;
#28065 = ORIENTED_EDGE ( 'NONE', *, *, #31991, .T. ) ;
#28066 = CARTESIAN_POINT ( 'NONE',  ( -13.82240055979716686, 28.15033208048753011, -10.03898445905979209 ) ) ;
#28067 = CARTESIAN_POINT ( 'NONE',  ( -19.47283267323017597, -27.28889818631711250, -4.999999999999996447 ) ) ;
#28068 = SHAPE_REPRESENTATION ( 'Dual-Edge Stainless Steel Rotary Blade', ( #24238 ), #11913 ) ;
#28069 = FACE_BOUND ( 'NONE', #1808, .T. ) ;
#28070 = EDGE_LOOP ( 'NONE', ( #36533, #28565, #34144, #497 ) ) ;
#28071 = CARTESIAN_POINT ( 'NONE',  ( -19.56896045557411767, -6.106514739740910969, -30.00000000000000711 ) ) ;
#28072 = CARTESIAN_POINT ( 'NONE',  ( -15.29981816934335548, -26.62016922504712468, -6.417125710678260653 ) ) ;
#28073 = CARTESIAN_POINT ( 'NONE',  ( 23.09341953181412421, -31.04079623447207581, 11.00000000000000000 ) ) ;
#28074 = VERTEX_POINT ( 'NONE', #8868 ) ;
#28075 = CARTESIAN_POINT ( 'NONE',  ( 24.08789872664181786, 1.422585201480351724, -18.55812312260739105 ) ) ;
#28076 = PLANE ( 'NONE',  #13495 ) ;
#28077 = DIRECTION ( 'NONE',  ( -0.000000000000000000, -0.000000000000000000, -1.000000000000000000 ) ) ;
#28078 = ADVANCED_FACE ( 'NONE', ( #21258 ), #5816, .F. ) ;
#28079 = ORIENTED_EDGE ( 'NONE', *, *, #2669, .F. ) ;
#28080 = CARTESIAN_POINT ( 'NONE',  ( -30.23117059640172144, -0.03771030696743234156, -8.764896985320813627 ) ) ;
#28081 = ORIENTED_EDGE ( 'NONE', *, *, #19484, .T. ) ;
#28082 = CARTESIAN_POINT ( 'NONE',  ( 32.24877215592500335, -1.831602888277810814, -6.842981059139255251 ) ) ;
#28083 = FACE_OUTER_BOUND ( 'NONE', #28070, .T. ) ;
#28084 = CARTESIAN_POINT ( 'NONE',  ( 31.14237565978548616, -19.77424633423373024, 17.92354375535250455 ) ) ;
#28085 = ORIENTED_EDGE ( 'NONE', *, *, #4667, .F. ) ;
#28086 = CIRCLE ( 'NONE', #2144, 16.00000000000000000 ) ;
#28087 = CARTESIAN_POINT ( 'NONE',  ( -22.72592367914349509, 4.308210353041426188, -18.81253349342975056 ) ) ;
#28088 = FACE_OUTER_BOUND ( 'NONE', #28996, .T. ) ;
#28089 = DIRECTION ( 'NONE',  ( 1.000000000000000000, 3.469446951953563307E-15, 0.000000000000000000 ) ) ;
#28090 = VECTOR ( 'NONE', #17389, 1000.000000000000000 ) ;
#28091 = DIRECTION ( 'NONE',  ( 0.000000000000000000, 0.000000000000000000, 1.000000000000000000 ) ) ;
#28092 = DIRECTION ( 'NONE',  ( 0.5000000000000038858, 0.8660254037844363761, 0.000000000000000000 ) ) ;
#28093 = CIRCLE ( 'NONE', #15779, 1.000000000000000000 ) ;
#28094 = FACE_BOUND ( 'NONE', #581, .T. ) ;
#28095 = AXIS2_PLACEMENT_3D ( 'NONE', #17632, #17018, #39343 ) ;
#28096 = CARTESIAN_POINT ( 'NONE',  ( 16.52773037515250465, 27.09393310381576114, 14.53008259254011136 ) ) ;
#28097 = CARTESIAN_POINT ( 'NONE',  ( -24.85289228938016493, 7.121634862230863838, -5.000000000000001776 ) ) ;
#28098 = CARTESIAN_POINT ( 'NONE',  ( 7.645071344821493753, 9.594463043616155318, 7.000000000000000000 ) ) ;
#28099 = EDGE_CURVE ( 'NONE', #7567, #27126, #33860, .T. ) ;
#28100 = CARTESIAN_POINT ( 'NONE',  ( -9.363324537585850038, 32.27640801132209702, 10.00000000000000000 ) ) ;
#28101 = CARTESIAN_POINT ( 'NONE',  ( 14.25810169807962424, -14.84648812655576045, -28.51942066398886055 ) ) ;
#28102 = CARTESIAN_POINT ( 'NONE',  ( 9.665073660139013256, 25.11464168560187460, 10.50000000000000533 ) ) ;
#28103 = CARTESIAN_POINT ( 'NONE',  ( 13.89677717944467794, 24.25367973778722686, -13.48336797208005677 ) ) ;
#28104 = AXIS2_PLACEMENT_3D ( 'NONE', #17287, #23569, #29857 ) ;
#28105 = ORIENTED_EDGE ( 'NONE', *, *, #19818, .F. ) ;
#28106 = CARTESIAN_POINT ( 'NONE',  ( -12.90278709585224348, 16.14496159291350352, -27.57500629962238747 ) ) ;
#28107 = CARTESIAN_POINT ( 'NONE',  ( -24.27776115474302543, -18.04224162735225079, 20.69868183039780973 ) ) ;
#28108 = MECHANICAL_DESIGN_GEOMETRIC_PRESENTATION_REPRESENTATION (  '', ( #34607 ), #26844 ) ;
#28109 = DIRECTION ( 'NONE',  ( -1.000000000000000000, 0.000000000000000000, 0.000000000000000000 ) ) ;
#28110 = CARTESIAN_POINT ( 'NONE',  ( 15.35804996106242193, 26.54817030761798335, -6.888046620688911936 ) ) ;
#28111 = ORIENTED_EDGE ( 'NONE', *, *, #11757, .T. ) ;
#28112 = CARTESIAN_POINT ( 'NONE',  ( 7.530592408760855783, 11.28437794979193498, 10.50000000000000000 ) ) ;
#28113 = VERTEX_POINT ( 'NONE', #36899 ) ;
#28115 = DIRECTION ( 'NONE',  ( 0.6691306063588571273, -0.7431448254773953543, 0.000000000000000000 ) ) ;
#28114 = CARTESIAN_POINT ( 'NONE',  ( -11.76301876381887368, 19.51941272550443429, -21.59238037788203357 ) ) ;
#28116 = CARTESIAN_POINT ( 'NONE',  ( -15.47508831886704250, -26.54255591950745341, -7.353815494023745458 ) ) ;
#28117 = DIRECTION ( 'NONE',  ( 0.1045284632676570929, 0.9945218953682730678, 0.000000000000000000 ) ) ;
#28118 = AXIS2_PLACEMENT_3D ( 'NONE', #30656, #27004, #11762 ) ;
#28119 = ORIENTED_EDGE ( 'NONE', *, *, #36845, .T. ) ;
#28120 = CARTESIAN_POINT ( 'NONE',  ( -30.95555434509626025, -15.01264802092781281, -11.97973923657508699 ) ) ;
#28121 = CARTESIAN_POINT ( 'NONE',  ( -14.53723555501347242, -26.50432973120043911, -5.000000000000000888 ) ) ;
#28122 = DIRECTION ( 'NONE',  ( 0.1045284632676415082, -0.9945218953682745111, 0.000000000000000000 ) ) ;
#28123 = CARTESIAN_POINT ( 'NONE',  ( 12.70988183501878055, 16.20822673541097458, -28.16655794507315491 ) ) ;
#28124 = ORIENTED_EDGE ( 'NONE', *, *, #30939, .T. ) ;
#28125 = CARTESIAN_POINT ( 'NONE',  ( 23.45594209662042573, 4.561666950054395819, -16.77008761711584128 ) ) ;
#28126 = EDGE_CURVE ( 'NONE', #15410, #13580, #21452, .T. ) ;
#28127 = CARTESIAN_POINT ( 'NONE',  ( -11.11016527260153630, 31.83082137946488643, 7.000000000000000000 ) ) ;
#28128 = CARTESIAN_POINT ( 'NONE',  ( -8.339609403135948895, 11.87216320208451137, 9.500000000000000000 ) ) ;
#28129 = DIRECTION ( 'NONE',  ( 0.000000000000000000, 0.000000000000000000, 1.000000000000000000 ) ) ;
#28130 = ORIENTED_EDGE ( 'NONE', *, *, #3414, .F. ) ;
#28131 = CARTESIAN_POINT ( 'NONE',  ( -31.27312981421062688, -0.4309787749141145707, -4.999999999999999112 ) ) ;
#28132 = CARTESIAN_POINT ( 'NONE',  ( 31.15015558338321711, -0.2976252405140638602, -5.000000000000000888 ) ) ;
#28133 = CIRCLE ( 'NONE', #3480, 1.000000000000000000 ) ;
#28134 = EDGE_CURVE ( 'NONE', #28389, #26241, #30805, .T. ) ;
#28135 = CARTESIAN_POINT ( 'NONE',  ( 26.32839453010175035, -14.27099112026796135, 20.82122704794079837 ) ) ;
#28136 = ORIENTED_EDGE ( 'NONE', *, *, #1106, .F. ) ;
#28137 = ADVANCED_FACE ( 'NONE', ( #918 ), #7402, .F. ) ;
#28138 = CARTESIAN_POINT ( 'NONE',  ( -7.289639608743034849, -27.06962010326280321, -13.42901749168595060 ) ) ;
#28139 = VECTOR ( 'NONE', #28601, 1000.000000000000000 ) ;
#28140 = CARTESIAN_POINT ( 'NONE',  ( -17.05532387642082526, 7.816133769664412867, 11.00000000000000000 ) ) ;
#28141 = ORIENTED_EDGE ( 'NONE', *, *, #14977, .F. ) ;
#28142 = B_SPLINE_CURVE_WITH_KNOTS ( 'NONE', 3,
 ( #2854, #19090, #16041, #6682, #15844, #37378 ),
 .UNSPECIFIED., .F., .F.,
 ( 4, 2, 4 ),
 ( 0.000000000000000000, 0.5000000000000000000, 1.000000000000000000 ),
 .UNSPECIFIED. ) ;
#28143 = PLANE ( 'NONE',  #13237 ) ;
#28144 = CARTESIAN_POINT ( 'NONE',  ( -22.48079666815685940, 18.61591633949185010, 11.00000000000000000 ) ) ;
#28145 = CARTESIAN_POINT ( 'NONE',  ( -8.312041872459065672, 25.58773265502866678, 6.000000000000000000 ) ) ;
#28146 = CARTESIAN_POINT ( 'NONE',  ( 3.842267464956742096, 37.63229749218292852, -7.124829648924612790 ) ) ;
#28147 = DIRECTION ( 'NONE',  ( -0.000000000000000000, -0.000000000000000000, -1.000000000000000000 ) ) ;
#28148 = EDGE_CURVE ( 'NONE', #6243, #38307, #16156, .T. ) ;
#28149 = DIRECTION ( 'NONE',  ( 0.000000000000000000, 0.000000000000000000, 1.000000000000000000 ) ) ;
#28150 = EDGE_CURVE ( 'NONE', #20144, #25142, #22237, .T. ) ;
#28151 = CARTESIAN_POINT ( 'NONE',  ( 7.766013557953383106, 28.81973365084986938, 10.50000000000000178 ) ) ;
#28152 = FACE_OUTER_BOUND ( 'NONE', #9707, .T. ) ;
#28153 = CARTESIAN_POINT ( 'NONE',  ( 8.541469607472738090, 17.40487552589537401, 6.000000000000000000 ) ) ;
#28154 = CARTESIAN_POINT ( 'NONE',  ( 8.238488885696289898, 24.65111619403943877, 9.000000000000001776 ) ) ;
#28155 = CARTESIAN_POINT ( 'NONE',  ( 14.51296530378405336, 26.99756090190063773, -9.645496975165400499 ) ) ;
#28156 = DIRECTION ( 'NONE',  ( 0.9781476007338042455, -0.2079116908177663370, -0.000000000000000000 ) ) ;
#28157 = ORIENTED_EDGE ( 'NONE', *, *, #9312, .F. ) ;
#28159 = DIRECTION ( 'NONE',  ( 1.000000000000000000, -1.387778780781439522E-14, 0.000000000000000000 ) ) ;
#28158 = CARTESIAN_POINT ( 'NONE',  ( -17.72206997426596686, 16.40768990500343349, -13.83464017129110957 ) ) ;
#28160 = VECTOR ( 'NONE', #7961, 1000.000000000000000 ) ;
#28161 = CARTESIAN_POINT ( 'NONE',  ( 12.84742388243086175, 15.65988663227523325, 11.00000000000000000 ) ) ;
#28162 = CARTESIAN_POINT ( 'NONE',  ( 9.766980772230919428, -18.57228960779583815, -26.22661689184167955 ) ) ;
#28163 = CARTESIAN_POINT ( 'NONE',  ( -21.99343813880628673, -26.08014713514513971, -8.986661558301907604 ) ) ;
#28164 = CARTESIAN_POINT ( 'NONE',  ( 15.41782702884244571, 26.77676039938714325, -5.474246347568364257 ) ) ;
#28165 = CARTESIAN_POINT ( 'NONE',  ( 15.16872908693824407, 26.30108831384980661, -8.297102614751414862 ) ) ;
#28166 = B_SPLINE_SURFACE_WITH_KNOTS ( 'NONE', 1, 3, ( 
 ( #26723, #8441, #24076, #11092, #33638, #29968, #5188, #21031, #17599, #8030 ),
 ( #39109, #17993, #5386, #33039, #20837, #21226, #14735, #27125, #26527, #36669 ) ),
 .UNSPECIFIED., .F., .F., .F.,
 ( 2, 2 ),
 ( 4, 2, 2, 2, 4 ),
 ( 0.000000000000000000, 1.000000000000000000 ),
 ( 4.638205445319954379, 5.030904527018678074, 5.423603608717401769, 5.816302690416126353, 6.209001772114850048 ),
 .UNSPECIFIED. ) ;
#28167 = ORIENTED_EDGE ( 'NONE', *, *, #4304, .T. ) ;
#28168 = CARTESIAN_POINT ( 'NONE',  ( 5.400683141673458643, 15.91724817395916070, 7.000000000000000000 ) ) ;
#28169 = CARTESIAN_POINT ( 'NONE',  ( -9.922080038078478381, -18.83169384875433039, -25.01962877829346965 ) ) ;
#28170 = CARTESIAN_POINT ( 'NONE',  ( -37.03648387062790448, -7.065924075330933363, 12.14047268033043991 ) ) ;
#28171 = AXIS2_PLACEMENT_3D ( 'NONE', #23417, #35809, #33175 ) ;
#28172 = CARTESIAN_POINT ( 'NONE',  ( -21.16141018750222713, -14.58779178538210175, -19.64528038461644499 ) ) ;
#28173 = CARTESIAN_POINT ( 'NONE',  ( -0.3069599879515859109, -21.90886338974817349, -20.12108918057204221 ) ) ;
#28174 = CARTESIAN_POINT ( 'NONE',  ( 15.11801385582561963, 24.79072481137326278, -10.19584184461111143 ) ) ;
#28175 = CARTESIAN_POINT ( 'NONE',  ( 18.36494381186184910, 9.412039940421420781, -27.17404324301481111 ) ) ;
#28176 = CARTESIAN_POINT ( 'NONE',  ( 0.000000000000000000, 22.50000000000000355, 13.00000000000000178 ) ) ;
#28177 = VERTEX_POINT ( 'NONE', #13294 ) ;
#28178 = CARTESIAN_POINT ( 'NONE',  ( -29.25378966048014107, -3.741898191150933695, -14.12891680041362363 ) ) ;
#28179 = EDGE_CURVE ( 'NONE', #24685, #37754, #25888, .T. ) ;
#28180 = AXIS2_PLACEMENT_3D ( 'NONE', #15957, #34639, #34051 ) ;
#28181 = CARTESIAN_POINT ( 'NONE',  ( -20.03472765055071036, 11.56705540218451311, 17.92354375535250810 ) ) ;
#28182 = ORIENTED_EDGE ( 'NONE', *, *, #17627, .F. ) ;
#28183 = CARTESIAN_POINT ( 'NONE',  ( 1.853849799106296548, 7.614518279115737087, 7.102474990965861323 ) ) ;
#28184 = DIRECTION ( 'NONE',  ( 0.2079116908177663370, 0.9781476007338042455, -0.000000000000000000 ) ) ;
#28185 = CARTESIAN_POINT ( 'NONE',  ( -20.46571904345125148, 1.196608941699672135, -29.35443162036549580 ) ) ;
#28186 = CARTESIAN_POINT ( 'NONE',  ( 35.25372542428971201, -14.20602460021386193, -5.437452493555934296 ) ) ;
#28187 = CARTESIAN_POINT ( 'NONE',  ( 20.74852905477029452, -28.65583854707664457, 13.92931973827808356 ) ) ;
#28188 = VERTEX_POINT ( 'NONE', #10458 ) ;
#28189 = CARTESIAN_POINT ( 'NONE',  ( 1.358225888363031819, 11.68927977431952137, 6.000000000000000000 ) ) ;
#28190 = ORIENTED_EDGE ( 'NONE', *, *, #14562, .F. ) ;
#28191 = CARTESIAN_POINT ( 'NONE',  ( -3.835137251120299684, 29.44922644035488446, 12.00000000000000000 ) ) ;
#28192 = FACE_OUTER_BOUND ( 'NONE', #20897, .T. ) ;
#28193 = CIRCLE ( 'NONE', #18463, 1.000000000000000000 ) ;
#28194 = CYLINDRICAL_SURFACE ( 'NONE', #25937, 1.000000000000000000 ) ;
#28195 = ORIENTED_EDGE ( 'NONE', *, *, #28784, .F. ) ;
#28196 = CARTESIAN_POINT ( 'NONE',  ( -2.246677149408780494, 20.47173499388784990, -28.45538990901911447 ) ) ;
#28197 = CARTESIAN_POINT ( 'NONE',  ( -35.48538791413474769, -11.24999995268676933, -5.000000000000001776 ) ) ;
#28198 = LINE ( 'NONE', #27806, #26041 ) ;
#28199 = EDGE_CURVE ( 'NONE', #1436, #11472, #20129, .T. ) ;
#28200 = CIRCLE ( 'NONE', #6786, 1.000000000000000000 ) ;
#28201 = CARTESIAN_POINT ( 'NONE',  ( 13.03640989728592459, 29.14264673470096767, 6.000000000000000000 ) ) ;
#28202 = LINE ( 'NONE', #31256, #39210 ) ;
#28203 = LINE ( 'NONE', #4013, #21610 ) ;
#28204 = CARTESIAN_POINT ( 'NONE',  ( 13.71665722575384194, 30.74286335228606148, -5.909757821034641978 ) ) ;
#28205 = AXIS2_PLACEMENT_3D ( 'NONE', #3953, #27058, #25887 ) ;
#28206 = ORIENTED_EDGE ( 'NONE', *, *, #18839, .F. ) ;
#28207 = CARTESIAN_POINT ( 'NONE',  ( -20.36441849243354696, 12.17262094050481913, -12.89086137884393324 ) ) ;
#28208 = CARTESIAN_POINT ( 'NONE',  ( 13.82587226056084262, 37.11292026376988673, 11.00000000000000000 ) ) ;
#28209 = CARTESIAN_POINT ( 'NONE',  ( 15.21101220493249251, -26.17680776644541041, -8.762161127626081125 ) ) ;
#28210 = CARTESIAN_POINT ( 'NONE',  ( 14.57486473880226008, 26.18419839932902349, 10.49999999999999822 ) ) ;
#28211 = CARTESIAN_POINT ( 'NONE',  ( 12.35927980519502611, 20.53300710371609838, -19.48961259234621934 ) ) ;
#28212 = CARTESIAN_POINT ( 'NONE',  ( 12.33616729053617966, -27.99489201236593416, -5.000000000000000000 ) ) ;
#28213 = CARTESIAN_POINT ( 'NONE',  ( -14.11133924723978161, 27.61078317377194224, 10.49999999999999822 ) ) ;
#28214 = CARTESIAN_POINT ( 'NONE',  ( -23.90157044124041263, -25.28113828194042867, -9.382323413831949566 ) ) ;
#28215 = CARTESIAN_POINT ( 'NONE',  ( 10.81257536403207276, -22.55273985443259477, -16.57830297862439295 ) ) ;
#28216 = CARTESIAN_POINT ( 'NONE',  ( 15.45156861522514369, 26.56435632827706428, -5.946109696244072040 ) ) ;
#28217 = CARTESIAN_POINT ( 'NONE',  ( 21.69387525390884264, -15.65483690961669261, -18.63891047137795098 ) ) ;
#28218 = CARTESIAN_POINT ( 'NONE',  ( 14.11133924723984201, 27.61078317377175040, 10.49999999999999822 ) ) ;
#28219 = CARTESIAN_POINT ( 'NONE',  ( -2.256323172317921788, 14.28970123917155277, 9.000000000000001776 ) ) ;
#28220 = ORIENTED_EDGE ( 'NONE', *, *, #24642, .T. ) ;
#28221 = CARTESIAN_POINT ( 'NONE',  ( -10.25240473134331154, 34.56179556857796342, -6.747403775044807261 ) ) ;
#28222 = CARTESIAN_POINT ( 'NONE',  ( -14.29712391636367563, -26.44587280164909870, -4.999999999999999112 ) ) ;
#28223 = ADVANCED_FACE ( 'NONE', ( #16767 ), #19197, .F. ) ;
#28224 = DIRECTION ( 'NONE',  ( 1.000000000000000000, 0.000000000000000000, 0.000000000000000000 ) ) ;
#28225 = AXIS2_PLACEMENT_3D ( 'NONE', #15578, #36919, #24122 ) ;
#28226 = DIRECTION ( 'NONE',  ( 0.000000000000000000, 0.000000000000000000, 1.000000000000000000 ) ) ;
#28227 = ORIENTED_EDGE ( 'NONE', *, *, #4814, .T. ) ;
#28228 = CARTESIAN_POINT ( 'NONE',  ( 29.56235616742567629, 0.08762005067959190152, -10.18130632035143535 ) ) ;
#28229 = ADVANCED_FACE ( 'NONE', ( #38288 ), #31586, .F. ) ;
#28230 = CARTESIAN_POINT ( 'NONE',  ( -12.26832665498866071, 32.91590888319122854, -4.999999999999996447 ) ) ;
#28231 = ADVANCED_FACE ( 'NONE', ( #28541 ), #27837, .T. ) ;
#28232 = CARTESIAN_POINT ( 'NONE',  ( -37.48531001978128074, -11.24999991186452775, 11.00000000000002309 ) ) ;
#28233 = ORIENTED_EDGE ( 'NONE', *, *, #13717, .F. ) ;
#28234 = AXIS2_PLACEMENT_3D ( 'NONE', #35671, #9634, #24466 ) ;
#28235 = CARTESIAN_POINT ( 'NONE',  ( -30.82577771627267182, 0.002281058920265444448, -5.946086761298152723 ) ) ;
#28236 = CARTESIAN_POINT ( 'NONE',  ( -20.24725037384592952, -26.82317351678327810, -7.696457708727984404 ) ) ;
#28237 = ORIENTED_EDGE ( 'NONE', *, *, #34744, .F. ) ;
#28238 = CARTESIAN_POINT ( 'NONE',  ( 25.22840985194761387, -4.440669541368661655, -18.96303409332410084 ) ) ;
#28239 = VECTOR ( 'NONE', #22103, 999.9999999999998863 ) ;
#28240 = EDGE_CURVE ( 'NONE', #36832, #23885, #19394, .T. ) ;
#28241 = VECTOR ( 'NONE', #5294, 1000.000000000000000 ) ;
#28242 = ORIENTED_EDGE ( 'NONE', *, *, #37077, .T. ) ;
#28243 = CARTESIAN_POINT ( 'NONE',  ( 17.15083734909593360, 27.26712758905532752, 12.73282698324853257 ) ) ;
#28244 = DIRECTION ( 'NONE',  ( 0.000000000000000000, 0.000000000000000000, 1.000000000000000000 ) ) ;
#28245 = LINE ( 'NONE', #421, #22154 ) ;
#28246 = CARTESIAN_POINT ( 'NONE',  ( -7.971538940947521468, 30.92644086613018928, 19.66345542862593376 ) ) ;
#28247 = DIRECTION ( 'NONE',  ( 0.000000000000000000, 0.000000000000000000, 1.000000000000000000 ) ) ;
#28248 = ORIENTED_EDGE ( 'NONE', *, *, #13737, .F. ) ;
#28249 = LINE ( 'NONE', #19300, #20962 ) ;
#28250 = CARTESIAN_POINT ( 'NONE',  ( -20.46375980781524007, 1.787259394981456362, -30.00000000000000711 ) ) ;
#28251 = DIRECTION ( 'NONE',  ( 1.000000000000000000, 0.000000000000000000, 0.000000000000000000 ) ) ;
#28252 = EDGE_CURVE ( 'NONE', #25424, #10554, #16241, .T. ) ;
#28253 = EDGE_CURVE ( 'NONE', #17719, #37972, #31798, .T. ) ;
#28254 = DIRECTION ( 'NONE',  ( 0.000000000000000000, 0.000000000000000000, 1.000000000000000000 ) ) ;
#28255 = ADVANCED_FACE ( 'NONE', ( #31992 ), #28940, .F. ) ;
#28256 = CARTESIAN_POINT ( 'NONE',  ( 17.96157960088948613, 18.73973607591619839, -8.370532139170391517 ) ) ;
#28257 = CARTESIAN_POINT ( 'NONE',  ( 4.686106015904482724, 20.84698696610319146, -25.69044758121691885 ) ) ;
#28258 = CARTESIAN_POINT ( 'NONE',  ( 17.52734727169944406, -27.07761244028429459, -6.386038267470317109 ) ) ;
#28259 = VECTOR ( 'NONE', #8789, 1000.000000000000000 ) ;
#28260 = CARTESIAN_POINT ( 'NONE',  ( 0.6894430450595149251, 37.48435367156681508, 7.485699520496978288 ) ) ;
#28261 = EDGE_LOOP ( 'NONE', ( #28351, #7551, #4510, #15444, #38268 ) ) ;
#28262 = CARTESIAN_POINT ( 'NONE',  ( -11.50355825530538212, 18.42073213090798944, -23.85688228919889653 ) ) ;
#28263 = AXIS2_PLACEMENT_3D ( 'NONE', #8692, #18042, #36726 ) ;
#28264 = CARTESIAN_POINT ( 'NONE',  ( -31.01938180031993753, -21.79666295253727171, 16.87380292611439359 ) ) ;
#28265 = CARTESIAN_POINT ( 'NONE',  ( 12.78263182082741523, -23.08026933373198020, -15.46555305964894167 ) ) ;
#28266 = DIRECTION ( 'NONE',  ( 1.000000000000000000, 0.000000000000000000, 0.000000000000000000 ) ) ;
#28267 = ORIENTED_EDGE ( 'NONE', *, *, #6545, .T. ) ;
#28268 = ORIENTED_EDGE ( 'NONE', *, *, #23047, .F. ) ;
#28269 = CARTESIAN_POINT ( 'NONE',  ( -12.94388269583936513, 26.17419193811465661, -13.31610081608094198 ) ) ;
#28270 = CARTESIAN_POINT ( 'NONE',  ( -17.57421241049386396, -24.84107886702332380, -12.30910806047397088 ) ) ;
#28271 = EDGE_CURVE ( 'NONE', #8524, #11294, #139, .T. ) ;
#28272 = CARTESIAN_POINT ( 'NONE',  ( 14.31603901957230462, 19.98981538725069740, 10.50000000000000533 ) ) ;
#28273 = ORIENTED_EDGE ( 'NONE', *, *, #37956, .F. ) ;
#28274 = CARTESIAN_POINT ( 'NONE',  ( -19.75415558344636580, -5.512529345569482153, -29.24332315753316891 ) ) ;
#28275 = CARTESIAN_POINT ( 'NONE',  ( -9.518731748684004401, -18.39049943551870925, -27.45506815792052180 ) ) ;
#28276 = CARTESIAN_POINT ( 'NONE',  ( -2.806807826039845022, 9.295007390093649846, 7.000000000000000000 ) ) ;
#28277 = ORIENTED_EDGE ( 'NONE', *, *, #29518, .F. ) ;
#28278 = CARTESIAN_POINT ( 'NONE',  ( 29.81424496809705715, 0.2234756960255703251, -9.241590868339290665 ) ) ;
#28279 = EDGE_CURVE ( 'NONE', #2419, #37407, #23373, .T. ) ;
#28280 = CARTESIAN_POINT ( 'NONE',  ( 3.503793317224327186, 8.420815634768674229, 7.499999999999990230 ) ) ;
#28281 = DIRECTION ( 'NONE',  ( 0.4067366430758010409, 0.9135454576426005335, -0.000000000000000000 ) ) ;
#28282 = ORIENTED_EDGE ( 'NONE', *, *, #11486, .T. ) ;
#28283 = CARTESIAN_POINT ( 'NONE',  ( -25.88842680114331785, 0.2780094573818647219, -16.43839041040183702 ) ) ;
#28284 = ORIENTED_EDGE ( 'NONE', *, *, #17363, .F. ) ;
#28285 = CARTESIAN_POINT ( 'NONE',  ( 21.07046404024911013, -0.6704196337341807865, -26.09432862330225333 ) ) ;
#28286 = CARTESIAN_POINT ( 'NONE',  ( 24.49409870379991716, -11.70597971641862856, 21.00000000000001776 ) ) ;
#28287 = CARTESIAN_POINT ( 'NONE',  ( 32.10122455788091145, -20.47530094824173474, 16.87380292611440424 ) ) ;
#28288 = ORIENTED_EDGE ( 'NONE', *, *, #13207, .F. ) ;
#28289 = AXIS2_PLACEMENT_3D ( 'NONE', #32325, #18487, #1 ) ;
#28290 = CARTESIAN_POINT ( 'NONE',  ( 14.44277748876681855, 26.55045409923015853, 7.500000000000000888 ) ) ;
#28291 = CARTESIAN_POINT ( 'NONE',  ( 3.428976547226190608, 28.19475011768619055, 20.94377226548378346 ) ) ;
#28292 = VECTOR ( 'NONE', #24115, 1000.000000000000000 ) ;
#28293 = AXIS2_PLACEMENT_3D ( 'NONE', #17850, #24329, #14788 ) ;
#28294 = CARTESIAN_POINT ( 'NONE',  ( 14.26377478793847509, 19.49255443956654688, 7.000000000000000000 ) ) ;
#28295 = AXIS2_PLACEMENT_3D ( 'NONE', #7064, #1186, #34709 ) ;
#28296 = CARTESIAN_POINT ( 'NONE',  ( -13.39464589777671044, 26.66807349098043289, 13.00000000000000178 ) ) ;
#28297 = FACE_BOUND ( 'NONE', #29259, .T. ) ;
#28298 = DIRECTION ( 'NONE',  ( 0.000000000000000000, 0.000000000000000000, -1.000000000000000000 ) ) ;
#28299 = CARTESIAN_POINT ( 'NONE',  ( -20.76109417526653544, 8.238746406137220646, -19.01874696799055897 ) ) ;
#28300 = CARTESIAN_POINT ( 'NONE',  ( 13.97675284653878691, -15.47333779752018756, -27.13317248147880534 ) ) ;
#28301 = DIRECTION ( 'NONE',  ( 1.000000000000000000, 0.000000000000000000, 0.000000000000000000 ) ) ;
#28302 = CARTESIAN_POINT ( 'NONE',  ( 13.13589401999236550, 22.37095606609392462, -16.42714977293202949 ) ) ;
#28303 = ORIENTED_EDGE ( 'NONE', *, *, #39922, .T. ) ;
#28304 = CARTESIAN_POINT ( 'NONE',  ( -16.06107056606509786, 23.80089718141779898, -7.844701006372616803 ) ) ;
#28305 = CARTESIAN_POINT ( 'NONE',  ( -27.53764137322051297, -17.13852093243013996, 20.25080042701539540 ) ) ;
#28306 = CARTESIAN_POINT ( 'NONE',  ( 10.79197459925287816, 32.88995393992981775, 10.68306085400109495 ) ) ;
#28307 = CARTESIAN_POINT ( 'NONE',  ( 11.07396762549639746, 17.40261846349473984, -28.07943001733049115 ) ) ;
#28308 = ORIENTED_EDGE ( 'NONE', *, *, #3598, .T. ) ;
#28309 = DIRECTION ( 'NONE',  ( 1.000000000000000000, 0.000000000000000000, 0.000000000000000000 ) ) ;
#28310 = VERTEX_POINT ( 'NONE', #12216 ) ;
#28312 = CARTESIAN_POINT ( 'NONE',  ( 5.440829913680675034, 10.60893893836775348, 13.00000000000000178 ) ) ;
#28311 = CARTESIAN_POINT ( 'NONE',  ( -10.86943063858312364, 17.38123995523577037, -29.99999999999998934 ) ) ;
#28313 = CARTESIAN_POINT ( 'NONE',  ( -14.95650897399027990, -25.69867652498056643, -10.16863992578564613 ) ) ;
#28314 = CARTESIAN_POINT ( 'NONE',  ( 12.71633695260870844, 14.58086916811563150, 10.68306085400105943 ) ) ;
#28315 = AXIS2_PLACEMENT_3D ( 'NONE', #31814, #10483, #28566 ) ;
#28316 = EDGE_LOOP ( 'NONE', ( #7383, #28528, #9464, #27609 ) ) ;
#28317 = CARTESIAN_POINT ( 'NONE',  ( -20.52236299606704151, -9.986717880826434524, -22.99756460869029340 ) ) ;
#28318 = CARTESIAN_POINT ( 'NONE',  ( -10.90147648380924927, -21.05887150913213191, -19.56414284889322630 ) ) ;
#28319 = CARTESIAN_POINT ( 'NONE',  ( 15.00099999999999767, 36.00000000000000711, 9.500000000000000000 ) ) ;
#28320 = CARTESIAN_POINT ( 'NONE',  ( 13.45249047345274640, 17.67863091976945000, -21.86233792381201724 ) ) ;
#28321 = ORIENTED_EDGE ( 'NONE', *, *, #352, .F. ) ;
#28322 = CARTESIAN_POINT ( 'NONE',  ( 21.14860408002057568, 5.266143715497261013, -22.06585488323975142 ) ) ;
#28323 = CIRCLE ( 'NONE', #23137, 15.00000000000000000 ) ;
#28324 = DIRECTION ( 'NONE',  ( 0.000000000000000000, 0.000000000000000000, 1.000000000000000000 ) ) ;
#28325 = DIRECTION ( 'NONE',  ( -0.000000000000000000, -0.000000000000000000, -1.000000000000000000 ) ) ;
#28326 = DIRECTION ( 'NONE',  ( -0.000000000000000000, -0.000000000000000000, -1.000000000000000000 ) ) ;
#28327 = VERTEX_POINT ( 'NONE', #26505 ) ;
#28328 = CARTESIAN_POINT ( 'NONE',  ( -24.22435077138248616, -0.2007882836984510588, -19.40349160117432703 ) ) ;
#28329 = CARTESIAN_POINT ( 'NONE',  ( 24.71184492219473228, 0.1155084257449812690, -18.40944145481854832 ) ) ;
#28330 = CARTESIAN_POINT ( 'NONE',  ( 29.45937559703822473, -11.06631500863537454, 20.25080042701566185 ) ) ;
#28331 = ORIENTED_EDGE ( 'NONE', *, *, #28959, .F. ) ;
#28332 = CARTESIAN_POINT ( 'NONE',  ( -5.636483973512888213, -22.01575377102104625, -29.99999999999999645 ) ) ;
#28333 = DIRECTION ( 'NONE',  ( 1.000000000000000000, 0.000000000000000000, 0.000000000000000000 ) ) ;
#28334 = ORIENTED_EDGE ( 'NONE', *, *, #21690, .F. ) ;
#28335 = PLANE ( 'NONE',  #1569 ) ;
#28336 = AXIS2_PLACEMENT_3D ( 'NONE', #200, #15638, #24380 ) ;
#28337 = AXIS2_PLACEMENT_3D ( 'NONE', #22409, #32381, #22210 ) ;
#28338 = CARTESIAN_POINT ( 'NONE',  ( -11.61617238037479538, 31.85261655609473408, 10.49999999999999822 ) ) ;
#28339 = CARTESIAN_POINT ( 'NONE',  ( 3.503793317224329851, 8.420815634768676006, 9.000000000000001776 ) ) ;
#28340 = CARTESIAN_POINT ( 'NONE',  ( 4.649262579009291407, 28.36936852218387983, -16.68779215659397153 ) ) ;
#28341 = DIRECTION ( 'NONE',  ( 0.000000000000000000, 0.000000000000000000, 1.000000000000000000 ) ) ;
#28342 = ADVANCED_FACE ( 'NONE', ( #33020 ), #1728, .T. ) ;
#28343 = CARTESIAN_POINT ( 'NONE',  ( 0.000000000000000000, 22.50000000000000355, 11.00000000000000178 ) ) ;
#28344 = DIRECTION ( 'NONE',  ( 0.8660254037844363761, -0.5000000000000039968, 0.000000000000000000 ) ) ;
#28345 = FACE_OUTER_BOUND ( 'NONE', #10223, .T. ) ;
#28346 = DIRECTION ( 'NONE',  ( 0.000000000000000000, 0.000000000000000000, 1.000000000000000000 ) ) ;
#28347 = DIRECTION ( 'NONE',  ( 0.000000000000000000, -0.7071067811865474617, -0.7071067811865474617 ) ) ;
#28348 = CARTESIAN_POINT ( 'NONE',  ( 11.04586147422109477, 19.50284389929768381, -22.62640361410345236 ) ) ;
#28349 = AXIS2_PLACEMENT_3D ( 'NONE', #39942, #33672, #3568 ) ;
#28350 = CARTESIAN_POINT ( 'NONE',  ( 5.440908595777814050, 35.94977745735560859, 7.000000000000000000 ) ) ;
#28351 = ORIENTED_EDGE ( 'NONE', *, *, #4512, .T. ) ;
#28353 = CARTESIAN_POINT ( 'NONE',  ( 2.061816823438564761, 8.019625857903918131, 10.49999999999999822 ) ) ;
#28352 = CARTESIAN_POINT ( 'NONE',  ( -18.23749494249763003, 18.64175607586350480, -6.439786763766045752 ) ) ;
#28354 = EDGE_CURVE ( 'NONE', #8840, #25521, #8421, .T. ) ;
#28355 = CARTESIAN_POINT ( 'NONE',  ( 21.39877161664088590, 15.54711762656346075, 11.00000000000000000 ) ) ;
#28356 = CARTESIAN_POINT ( 'NONE',  ( 14.34475445268075156, -25.06822468207680288, -11.59938494084682326 ) ) ;
#28357 = EDGE_CURVE ( 'NONE', #21780, #2164, #7606, .T. ) ;
#28358 = DIRECTION ( 'NONE',  ( -0.000000000000000000, -0.000000000000000000, -1.000000000000000000 ) ) ;
#28359 = CARTESIAN_POINT ( 'NONE',  ( 13.49046931713162145, 22.81729818279096023, -15.45058010560173045 ) ) ;
#28360 = CARTESIAN_POINT ( 'NONE',  ( 13.47891791608170209, 22.84109221470872697, -15.44783060290720300 ) ) ;
#28361 = EDGE_LOOP ( 'NONE', ( #17644, #16969, #18314, #23340 ) ) ;
#28362 = CYLINDRICAL_SURFACE ( 'NONE', #4924, 6.000000000000003553 ) ;
#28363 = CARTESIAN_POINT ( 'NONE',  ( -9.719952024558851988, -18.59326785210745925, -26.23105664925188307 ) ) ;
#28364 = CARTESIAN_POINT ( 'NONE',  ( -35.50541758542772186, -3.488475578028477742, 12.73282698324853257 ) ) ;
#28365 = CARTESIAN_POINT ( 'NONE',  ( -31.58328445775233106, -21.78494312990649462, -5.436021537729467390 ) ) ;
#28366 = CARTESIAN_POINT ( 'NONE',  ( -4.072631098700577823, -22.66826574189022381, -16.93478912211341481 ) ) ;
#28367 = CARTESIAN_POINT ( 'NONE',  ( 15.55049802031632034, 25.65338682851541563, -7.361195678376786233 ) ) ;
#28368 = ORIENTED_EDGE ( 'NONE', *, *, #13515, .F. ) ;
#28369 = CARTESIAN_POINT ( 'NONE',  ( 22.79531528405124163, 10.15988774222570434, -4.999999999999998224 ) ) ;
#28370 = LINE ( 'NONE', #3202, #19950 ) ;
#28371 = CARTESIAN_POINT ( 'NONE',  ( -11.91493164750346700, 32.61411734499214532, 16.87380292611442201 ) ) ;
#28372 = ORIENTED_EDGE ( 'NONE', *, *, #32753, .T. ) ;
#28373 = CARTESIAN_POINT ( 'NONE',  ( -33.52901403654990276, -3.501605748354566394, -5.000000000000002665 ) ) ;
#28374 = AXIS2_PLACEMENT_3D ( 'NONE', #6534, #28281, #19137 ) ;
#28375 = AXIS2_PLACEMENT_3D ( 'NONE', #14594, #2405, #39369 ) ;
#28376 = CARTESIAN_POINT ( 'NONE',  ( -18.42861860568109833, 16.71074749267419435, 16.87380292611394239 ) ) ;
#28377 = ORIENTED_EDGE ( 'NONE', *, *, #14135, .T. ) ;
#28378 = CARTESIAN_POINT ( 'NONE',  ( -9.997483185316569987, 21.95197631500770896, 10.49999999999999467 ) ) ;
#28379 = ADVANCED_FACE ( 'NONE', ( #17174 ), #29346, .F. ) ;
#28380 = DIRECTION ( 'NONE',  ( -0.1470157664651899898, 0.6916548014802332833, -0.7071067811865417996 ) ) ;
#28381 = EDGE_CURVE ( 'NONE', #5904, #18376, #13909, .T. ) ;
#28382 = CIRCLE ( 'NONE', #21886, 1.000000000000000000 ) ;
#28383 = CARTESIAN_POINT ( 'NONE',  ( -24.37716644428920887, 0.8142858702769540935, -18.49331350387625150 ) ) ;
#28384 = B_SPLINE_CURVE_WITH_KNOTS ( 'NONE', 3,
 ( #1319, #25484, #19004, #28740, #32200, #25298, #10058, #6994, #6794, #22437 ),
 .UNSPECIFIED., .F., .F.,
 ( 4, 2, 2, 2, 4 ),
 ( 0.000000000000000000, 0.2500000000000000000, 0.5000000000000000000, 0.7500000000000000000, 1.000000000000000000 ),
 .UNSPECIFIED. ) ;
#28385 = CARTESIAN_POINT ( 'NONE',  ( 25.71601288570474253, -10.35479112961458092, -17.64613853693563073 ) ) ;
#28387 = AXIS2_PLACEMENT_3D ( 'NONE', #29382, #7843, #1557 ) ;
#28386 = CARTESIAN_POINT ( 'NONE',  ( 37.00900745416906545, -9.025932648522378088, 13.32518128616608877 ) ) ;
#28388 = ORIENTED_EDGE ( 'NONE', *, *, #28357, .F. ) ;
#28389 = VERTEX_POINT ( 'NONE', #38696 ) ;
#28390 = DIRECTION ( 'NONE',  ( 1.000000000000000000, 1.224646799147351235E-16, -0.000000000000000000 ) ) ;
#28391 = DIRECTION ( 'NONE',  ( 1.000000000000000000, 0.000000000000000000, 0.000000000000000000 ) ) ;
#28392 = CARTESIAN_POINT ( 'NONE',  ( -7.468455364333119739, 29.89744377950679421, 10.50000000000000000 ) ) ;
#28393 = ORIENTED_EDGE ( 'NONE', *, *, #24546, .T. ) ;
#28394 = CARTESIAN_POINT ( 'NONE',  ( -2.693587759434362461, 33.22306132784108001, -12.89973256833978787 ) ) ;
#28395 = CYLINDRICAL_SURFACE ( 'NONE', #32777, 1.000000000000000000 ) ;
#28396 = FACE_OUTER_BOUND ( 'NONE', #35227, .T. ) ;
#28397 = VECTOR ( 'NONE', #38158, 1000.000000000000000 ) ;
#28398 = DIRECTION ( 'NONE',  ( -0.9781476007338070211, -0.2079116908177534029, 0.000000000000000000 ) ) ;
#28400 = EDGE_CURVE ( 'NONE', #32508, #15787, #26702, .T. ) ;
#28399 = DIRECTION ( 'NONE',  ( -0.9135454576426004225, 0.4067366430758009854, 0.000000000000000000 ) ) ;
#28401 = DIRECTION ( 'NONE',  ( -0.2185080122243950040, 0.6724985119639662612, 0.7071067811865437980 ) ) ;
#28402 = CIRCLE ( 'NONE', #38793, 1.000000000000000888 ) ;
#28403 = CARTESIAN_POINT ( 'NONE',  ( 12.56655098099258794, 27.87547247283417917, -12.29340594856549984 ) ) ;
#28404 = AXIS2_PLACEMENT_3D ( 'NONE', #33650, #26735, #14947 ) ;
#28405 = ORIENTED_EDGE ( 'NONE', *, *, #20314, .T. ) ;
#28406 = CARTESIAN_POINT ( 'NONE',  ( -18.00818492405559823, 9.835074072281088320, -28.86228936887301089 ) ) ;
#28407 = CARTESIAN_POINT ( 'NONE',  ( -5.644276917315533382, 36.40655018617698602, 11.00000000000000000 ) ) ;
#28408 = CARTESIAN_POINT ( 'NONE',  ( 13.76081720998434221, -24.12408036951367762, -13.50911283364834681 ) ) ;
#28409 = DIRECTION ( 'NONE',  ( 1.000000000000000000, 0.000000000000000000, 0.000000000000000000 ) ) ;
#28410 = CARTESIAN_POINT ( 'NONE',  ( 13.73332615291622005, 23.47756605762641868, -14.46771515761556337 ) ) ;
#28411 = CARTESIAN_POINT ( 'NONE',  ( 11.41987377193677489, -19.41918266173338026, -30.00000000000000000 ) ) ;
#28412 = CYLINDRICAL_SURFACE ( 'NONE', #5122, 17.00000000000000711 ) ;
#28413 = VECTOR ( 'NONE', #39819, 1000.000000000000000 ) ;
#28414 = CARTESIAN_POINT ( 'NONE',  ( -14.21852471880019664, -15.07395324936907954, -27.81797908992425761 ) ) ;
#28415 = CARTESIAN_POINT ( 'NONE',  ( 8.079555417519777905, -24.49239216019507026, -10.79927774074996094 ) ) ;
#28416 = CARTESIAN_POINT ( 'NONE',  ( 15.40046916436526558, 26.40062519190980694, -6.888357274586806689 ) ) ;
#28417 = CARTESIAN_POINT ( 'NONE',  ( 19.98114792981366961, -14.40613482780026722, -20.72081132955061022 ) ) ;
#28418 = CARTESIAN_POINT ( 'NONE',  ( 13.86243997625764557, 27.52991089825170690, 10.94387467463490538 ) ) ;
#28419 = CARTESIAN_POINT ( 'NONE',  ( 11.44473057578109199, 31.45924896672603310, 10.50000000000000178 ) ) ;
#28420 = ORIENTED_EDGE ( 'NONE', *, *, #20615, .T. ) ;
#28421 = CARTESIAN_POINT ( 'NONE',  ( -7.254375287122624805, 27.20239578260290259, -16.79518470217901438 ) ) ;
#28422 = CARTESIAN_POINT ( 'NONE',  ( 12.37435565298211415, 15.93301270189216545, 7.499999999999997335 ) ) ;
#28423 = DIRECTION ( 'NONE',  ( -1.000000000000000000, 0.000000000000000000, 0.000000000000000000 ) ) ;
#28424 = EDGE_LOOP ( 'NONE', ( #28227, #34385, #20024, #10580, #12052, #25308, #27136, #27476, #8304, #22412, #30229, #103, #762, #20556, #17108, #28485, #19515, #30463, #3792, #38614, #27978, #22130, #16378, #36583, #8889, #6021, #27602, #40170, #16979, #27533, #27803, #2100, #20465, #33104, #612, #1171, #809, #33582, #34249, #13149, #40119, #5147, #13259, #38804, #23029, #32634, #17994, #14365, #14088, #31673, #18846, #2, #31810, #18687, #35622, #17219, #20303, #38251, #29674, #14491, #38984, #21416, #32105, #18966, #5754, #29035, #13190, #18894, #11578, #6522, #22258, #12530, #39110, #2269, #16686, #19687, #20541, #27789, #26916, #18798, #1544, #23205, #6780, #37422, #6096, #16602, #24415, #28522, #17124, #37216, #21119, #21352, #36884, #14958, #15595, #17414, #24070, #9080, #27462, #29274, #30160 ) ) ;
#28425 = CARTESIAN_POINT ( 'NONE',  ( 25.23308087229151653, 0.3395914844611204186, -17.43355021032456875 ) ) ;
#28426 = CARTESIAN_POINT ( 'NONE',  ( -8.301277145684272440, 36.28737808747504801, -5.000000000000000000 ) ) ;
#28427 = ADVANCED_FACE ( 'NONE', ( #26904 ), #7810, .F. ) ;
#28428 = CARTESIAN_POINT ( 'NONE',  ( 0.6108529249775871417, 37.48755679569043053, 7.500000000000000888 ) ) ;
#28429 = ADVANCED_FACE ( 'NONE', ( #18317 ), #4969, .T. ) ;
#28430 = VERTEX_POINT ( 'NONE', #27653 ) ;
#28431 = CARTESIAN_POINT ( 'NONE',  ( -28.30077390381833879, 0.1879860857717292055, -12.55250302845952071 ) ) ;
#28432 = CARTESIAN_POINT ( 'NONE',  ( -3.835137251120299684, 29.44922644035488446, 13.00000000000000178 ) ) ;
#28433 = ORIENTED_EDGE ( 'NONE', *, *, #11517, .T. ) ;
#28434 = CARTESIAN_POINT ( 'NONE',  ( 35.00061772621288725, -7.347685171788704395, -5.885183883027742091 ) ) ;
#28435 = AXIS2_PLACEMENT_3D ( 'NONE', #28831, #22328, #35333 ) ;
#28436 = AXIS2_PLACEMENT_3D ( 'NONE', #36038, #8198, #11657 ) ;
#28437 = ORIENTED_EDGE ( 'NONE', *, *, #26694, .T. ) ;
#28438 = CARTESIAN_POINT ( 'NONE',  ( -16.82090372984253435, 29.19711159930247746, 11.55979286843847653 ) ) ;
#28439 = TOROIDAL_SURFACE ( 'NONE', #23928, 16.00000000000000000, 2.000000000000000000 ) ;
#28440 = DIRECTION ( 'NONE',  ( 1.000000000000000000, 0.000000000000000000, 0.000000000000000000 ) ) ;
#28441 = CARTESIAN_POINT ( 'NONE',  ( 15.00099999999999767, 36.50000000000000711, 7.500000000000000888 ) ) ;
#28442 = CARTESIAN_POINT ( 'NONE',  ( 10.24444524355854291, 27.94074263397462232, 19.66345542862530493 ) ) ;
#28443 = VECTOR ( 'NONE', #5253, 1000.000000000000114 ) ;
#28444 = FACE_OUTER_BOUND ( 'NONE', #23173, .T. ) ;
#28445 = ORIENTED_EDGE ( 'NONE', *, *, #8508, .F. ) ;
#28446 = CARTESIAN_POINT ( 'NONE',  ( -3.370709253380788084E-06, 22.50000000000031264, 6.000000000000000000 ) ) ;
#28447 = CARTESIAN_POINT ( 'NONE',  ( 8.988510393147455702, 18.42811980848636821, -30.00000000000000000 ) ) ;
#28448 = DIRECTION ( 'NONE',  ( 1.000000000000000000, 0.000000000000000000, 0.000000000000000000 ) ) ;
#28449 = LINE ( 'NONE', #625, #5879 ) ;
#28450 = ADVANCED_FACE ( 'NONE', ( #23456 ), #8467, .T. ) ;
#28451 = CARTESIAN_POINT ( 'NONE',  ( 17.40746082178494447, 19.58779920104105088, -9.330282795758028769 ) ) ;
#28452 = CARTESIAN_POINT ( 'NONE',  ( 5.245966764456291287, 20.42028367153013235, -26.38657226523553945 ) ) ;
#28453 = ORIENTED_EDGE ( 'NONE', *, *, #5599, .F. ) ;
#28454 = CARTESIAN_POINT ( 'NONE',  ( 16.47100665901824001, -26.88200473344899066, -6.401141426531012257 ) ) ;
#28455 = CARTESIAN_POINT ( 'NONE',  ( 4.441848239913459118, 24.85865334748800137, 21.00000000000001066 ) ) ;
#28456 = CARTESIAN_POINT ( 'NONE',  ( 5.767236651883453469, 13.71142893291679954, 11.00000000000000000 ) ) ;
#28457 = AXIS2_PLACEMENT_3D ( 'NONE', #4810, #38530, #11315 ) ;
#28458 = ORIENTED_EDGE ( 'NONE', *, *, #466, .T. ) ;
#28460 = CONICAL_SURFACE ( 'NONE', #24555, 1.000000000000000888, 0.7853981633974552734 ) ;
#28459 = CARTESIAN_POINT ( 'NONE',  ( -11.69322940238108188, 18.90460750012263347, -22.73643640026262247 ) ) ;
#28461 = CARTESIAN_POINT ( 'NONE',  ( -31.91928157790810516, -18.42860581134450726, 17.92354375535250810 ) ) ;
#28462 = CARTESIAN_POINT ( 'NONE',  ( 9.372336683666530277, -18.28158583912481916, -28.71275810336947742 ) ) ;
#28463 = CARTESIAN_POINT ( 'NONE',  ( 8.160254037844357100, 16.63397459621552699, 10.49999999999999822 ) ) ;
#28464 = ORIENTED_EDGE ( 'NONE', *, *, #37409, .T. ) ;
#28465 = VERTEX_POINT ( 'NONE', #20417 ) ;
#28466 = AXIS2_PLACEMENT_3D ( 'NONE', #22190, #18561, #3310 ) ;
#28467 = CARTESIAN_POINT ( 'NONE',  ( -8.885346522200764596, 20.34420481528383817, -23.48319193123574067 ) ) ;
#28468 = CARTESIAN_POINT ( 'NONE',  ( -13.95683075005229767, 28.08631143191951196, 11.00000000000000000 ) ) ;
#28469 = FACE_BOUND ( 'NONE', #19569, .T. ) ;
#28470 = CARTESIAN_POINT ( 'NONE',  ( -30.09940253797056897, -9.337810905337370571, -13.89521527110805188 ) ) ;
#28471 = CARTESIAN_POINT ( 'NONE',  ( -9.394881763177457046, -18.22048488343288142, -30.00000000000000000 ) ) ;
#28472 = DIRECTION ( 'NONE',  ( 0.4067366430758009299, 0.9135454576426005335, 0.000000000000000000 ) ) ;
#28473 = ORIENTED_EDGE ( 'NONE', *, *, #13131, .F. ) ;
#28474 = CARTESIAN_POINT ( 'NONE',  ( 20.55243914501509650, 1.720701587877496275, -28.11989156925753974 ) ) ;
#28475 = FACE_OUTER_BOUND ( 'NONE', #19458, .T. ) ;
#28476 = LINE ( 'NONE', #19739, #4357 ) ;
#28477 = ORIENTED_EDGE ( 'NONE', *, *, #12718, .F. ) ;
#28478 = EDGE_CURVE ( 'NONE', #38994, #3204, #25967, .T. ) ;
#28479 = CARTESIAN_POINT ( 'NONE',  ( -24.58066270203448411, 0.3884518765734885637, -18.44634674746681569 ) ) ;
#28481 = EDGE_CURVE ( 'NONE', #3501, #35666, #4566, .T. ) ;
#28480 = VERTEX_POINT ( 'NONE', #40036 ) ;
#28482 = CARTESIAN_POINT ( 'NONE',  ( 32.40677704871944087, -1.850583768531564033, -5.924515326665249937 ) ) ;
#28483 = CARTESIAN_POINT ( 'NONE',  ( 23.19735768193467962, -14.64350930037813647, 20.99999999999999289 ) ) ;
#28484 = CARTESIAN_POINT ( 'NONE',  ( 27.04902410904039556, -24.92680750149222746, 16.87380292611402055 ) ) ;
#28485 = ORIENTED_EDGE ( 'NONE', *, *, #13491, .T. ) ;
#28486 = CARTESIAN_POINT ( 'NONE',  ( 1.265502442671760264, 36.24516302788250499, 13.00000000000000178 ) ) ;
#28487 = CARTESIAN_POINT ( 'NONE',  ( 3.003889247183332056, 27.48891118973832448, 20.99999999999999645 ) ) ;
#28488 = AXIS2_PLACEMENT_3D ( 'NONE', #19409, #7966, #14064 ) ;
#28489 = VECTOR ( 'NONE', #27357, 1000.000000000000000 ) ;
#28490 = DIRECTION ( 'NONE',  ( -1.000000000000000000, 0.000000000000000000, 0.000000000000000000 ) ) ;
#28491 = DIRECTION ( 'NONE',  ( 0.6916548014802318400, -0.1470157664651868257, 0.7071067811865437980 ) ) ;
#28492 = AXIS2_PLACEMENT_3D ( 'NONE', #6107, #12609, #37392 ) ;
#28493 = B_SPLINE_SURFACE_WITH_KNOTS ( 'NONE', 3, 3, ( 
 ( #5281, #27219, #2046, #33734 ),
 ( #17695, #17493, #18282, #36563 ),
 ( #36368, #2837, #26818, #21125 ),
 ( #24370, #39404, #33534, #5678 ),
 ( #23972, #18089, #8532, #15228 ),
 ( #15025, #20926, #40000, #33334 ),
 ( #30477, #27614, #27416, #20531 ),
 ( #36766, #5084, #5478, #37564 ),
 ( #31267, #587, #9536, #12575 ),
 ( #12969, #21717, #37761, #391 ),
 ( #12771, #27818, #21518, #9931 ),
 ( #6665, #25359, #19264, #24765 ),
 ( #9734, #21914, #37161, #3429 ),
 ( #3033, #34119, #31664, #33921 ),
 ( #9133, #16024, #15826, #28411 ),
 ( #28212, #34713, #22117, #18876 ),
 ( #22313, #31071, #6077, #6865 ),
 ( #15628, #18481, #34515, #30872 ),
 ( #3830, #16229, #15427, #18679 ),
 ( #13230, #28613, #12376, #3235 ),
 ( #12179, #24573, #36967, #9336 ),
 ( #6276, #28013, #25167, #187 ),
 ( #24967, #37361, #34317, #6471 ),
 ( #19073, #31464, #3629, #10944 ),
 ( #4435, #25559, #23329, #32682 ),
 ( #26369, #16634, #32481, #16838 ),
 ( #13773, #25760, #28815, #35314 ),
 ( #38157, #10734, #32062, #10329 ),
 ( #19880, #35518, #35725, #7266 ),
 ( #4836, #20084, #7877, #38358 ),
 ( #13978, #1595, #22709, #38762 ),
 ( #32269, #29015, #35114, #1191 ),
 ( #10131, #20282, #37960, #13571 ),
 ( #17246, #22506, #4636, #31861 ),
 ( #23119, #13166, #17038, #34917 ),
 ( #13372, #7682, #4232, #19668 ),
 ( #29418, #26166, #7473, #38560 ),
 ( #29219, #783, #10530, #25958 ),
 ( #1389, #22913, #7068, #19466 ),
 ( #4024, #16425, #990, #30024 ),
 ( #38965, #11938, #26575, #2200 ),
 ( #5036, #21083, #35921, #5839 ),
 ( #17448, #29618, #39564, #39160 ),
 ( #32884, #14383, #11740, #11342 ) ),
 .UNSPECIFIED., .T., .F., .F.,
 ( 4, 1, 1, 1, 2, 1, 1, 1, 1, 1, 1, 1, 2, 1, 1, 1, 2, 1, 1, 1, 1, 1, 1, 1, 2, 1, 1, 1, 2, 1, 1, 1, 1, 1, 1, 1, 4 ),
 ( 4, 4 ),
 ( 0.000000000000000000, 0.03553882639362128393, 0.07107765278724256786, 0.1066164791808638657, 0.1421553055744851357, 0.1660525590443411859, 0.1899498125141971805, 0.2138470659840532306, 0.2377443194539092253, 0.2616415729237652754, 0.2855388263936212701, 0.3094360798634773202, 0.3333333333333333703, 0.3688721597269547514, 0.4044109861205760215, 0.4399498125141973470, 0.4754886389078186171, 0.4993858923776745562, 0.5232831458475305508, 0.5471803993173864900, 0.5710776527872425401, 0.5949749062570985902, 0.6188721597269547514, 0.6427694131968104685, 0.6666666666666665186, 0.7022054930602876777, 0.7377443194539090587, 0.7732831458475302178, 0.8088219722411513768, 0.8327192257110074269, 0.8566164791808634771, 0.8805137326507195272, 0.9044109861205756884, 0.9283082395904318496, 0.9522054930602878997, 0.9761027465301439499, 1.000000000000000000 ),
 ( 0.000000000000000000, 1.000000000000000000 ),
 .UNSPECIFIED. ) ;
#28494 = EDGE_CURVE ( 'NONE', #19954, #4096, #37660, .T. ) ;
#28495 = CARTESIAN_POINT ( 'NONE',  ( -11.20744270277957888, 31.91841037101610112, 10.99999999999999822 ) ) ;
#28496 = EDGE_CURVE ( 'NONE', #9639, #2436, #16264, .T. ) ;
#28497 = CARTESIAN_POINT ( 'NONE',  ( 32.33143948541787438, 1.358872982501808435, 11.00000000000000000 ) ) ;
#28498 = CARTESIAN_POINT ( 'NONE',  ( -22.89598029550568015, 9.861910665086448091, -6.936501474781229248 ) ) ;
#28499 = CARTESIAN_POINT ( 'NONE',  ( 22.29802552750217259, -25.97160884719322738, -8.980211844774188990 ) ) ;
#28500 = DIRECTION ( 'NONE',  ( 1.224646799147351235E-16, -1.000000000000000000, 0.000000000000000000 ) ) ;
#28501 = CARTESIAN_POINT ( 'NONE',  ( 13.94130713879165562, 24.14927663816028058, -13.49308697109902511 ) ) ;
#28502 = VERTEX_POINT ( 'NONE', #33955 ) ;
#28503 = CARTESIAN_POINT ( 'NONE',  ( -13.04719345707401779, 18.83419094417813255, -20.69477310159956573 ) ) ;
#28504 = EDGE_CURVE ( 'NONE', #21190, #9720, #37792, .T. ) ;
#28505 = CARTESIAN_POINT ( 'NONE',  ( -20.20329687195632218, -21.14155277498739594, 20.25080042701566541 ) ) ;
#28506 = DIRECTION ( 'NONE',  ( -0.9781476007338041345, 0.2079116908177664202, 0.000000000000000000 ) ) ;
#28507 = CARTESIAN_POINT ( 'NONE',  ( 12.95272860106239499, 21.61356709058502545, -17.44179881794794795 ) ) ;
#28508 = EDGE_LOOP ( 'NONE', ( #28563, #38987, #38941, #36590, #32011 ) ) ;
#28509 = CARTESIAN_POINT ( 'NONE',  ( 31.49474942026707325, -16.12477659677660569, -11.06936912200789180 ) ) ;
#28510 = DIRECTION ( 'NONE',  ( -0.000000000000000000, -0.000000000000000000, -1.000000000000000000 ) ) ;
#28511 = ORIENTED_EDGE ( 'NONE', *, *, #17665, .T. ) ;
#28513 = DIRECTION ( 'NONE',  ( -0.4067366430758009299, -0.9135454576426005335, 0.000000000000000000 ) ) ;
#28512 = CARTESIAN_POINT ( 'NONE',  ( -13.67015811309539153, 23.61746135327068075, -14.45312116646361211 ) ) ;
#28514 = CARTESIAN_POINT ( 'NONE',  ( -11.00685563857638449, -19.43747507878832437, -22.67326838232596131 ) ) ;
#28515 = DIRECTION ( 'NONE',  ( -0.000000000000000000, 0.000000000000000000, 1.000000000000000000 ) ) ;
#28516 = AXIS2_PLACEMENT_3D ( 'NONE', #8219, #8624, #23861 ) ;
#28517 = ORIENTED_EDGE ( 'NONE', *, *, #12061, .F. ) ;
#28518 = CARTESIAN_POINT ( 'NONE',  ( -29.13733599210751990, -14.13474271335126708, -13.81261361319337055 ) ) ;
#28519 = CARTESIAN_POINT ( 'NONE',  ( -14.48060417942811817, -26.41903408085133265, -6.418214492182147346 ) ) ;
#28520 = DIRECTION ( 'NONE',  ( 1.000000000000000000, 0.000000000000000000, 0.000000000000000000 ) ) ;
#28521 = CARTESIAN_POINT ( 'NONE',  ( 16.33296907320687552, 23.02383901948744338, -7.850688138034399799 ) ) ;
#28522 = ORIENTED_EDGE ( 'NONE', *, *, #20329, .T. ) ;
#28523 = CARTESIAN_POINT ( 'NONE',  ( 25.95036642640170754, 5.573903512884414546, -6.435863300068679571 ) ) ;
#28524 = CARTESIAN_POINT ( 'NONE',  ( 12.14716901145161643, 12.46304090461738667, 13.00000000000000178 ) ) ;
#28525 = DIRECTION ( 'NONE',  ( -0.9945218953682729568, 0.1045284632676569680, 0.000000000000000000 ) ) ;
#28526 = CARTESIAN_POINT ( 'NONE',  ( -10.44367147699325749, 33.07775263288209544, 10.49999999999999822 ) ) ;
#28527 = VECTOR ( 'NONE', #24356, 1000.000000000000000 ) ;
#28528 = ORIENTED_EDGE ( 'NONE', *, *, #3090, .T. ) ;
#28529 = EDGE_CURVE ( 'NONE', #16598, #32934, #2637, .T. ) ;
#28530 = CARTESIAN_POINT ( 'NONE',  ( -22.30193131537437168, 0.3262574266873361495, -22.69144778596356460 ) ) ;
#28531 = EDGE_CURVE ( 'NONE', #35565, #37355, #27261, .T. ) ;
#28532 = CARTESIAN_POINT ( 'NONE',  ( 29.89909462720550692, -0.2920382172860754855, -10.15462489924079570 ) ) ;
#28533 = CARTESIAN_POINT ( 'NONE',  ( 25.71034552362537084, -20.07240169439175403, 19.99202127657074257 ) ) ;
#28534 = ORIENTED_EDGE ( 'NONE', *, *, #29703, .F. ) ;
#28535 = CARTESIAN_POINT ( 'NONE',  ( -21.88499642459564498, -5.528038495964382015, -20.11584339644715413 ) ) ;
#28536 = CARTESIAN_POINT ( 'NONE',  ( -11.78894649379783388, 21.72623886970244911, 13.00000000000000178 ) ) ;
#28537 = ORIENTED_EDGE ( 'NONE', *, *, #37481, .F. ) ;
#28538 = B_SPLINE_CURVE_WITH_KNOTS ( 'NONE', 3,
 ( #17427, #33468, #8261, #5814, #39538, #21254, #11717, #23903 ),
 .UNSPECIFIED., .F., .F.,
 ( 4, 2, 2, 4 ),
 ( 0.000000000000000000, 0.0004726692273637239823, 0.0007090038410455826124, 0.0009453384547274412426 ),
 .UNSPECIFIED. ) ;
#28539 = DIRECTION ( 'NONE',  ( 0.7431448254773848072, -0.6691306063588687847, -0.000000000000000000 ) ) ;
#28540 = VECTOR ( 'NONE', #25055, 1000.000000000000000 ) ;
#28541 = FACE_OUTER_BOUND ( 'NONE', #37870, .T. ) ;
#28542 = CARTESIAN_POINT ( 'NONE',  ( -9.806982162272253944, 13.84996144622306247, 12.00000000000000000 ) ) ;
#28543 = CARTESIAN_POINT ( 'NONE',  ( 2.081989859667413345, 20.63897288273475894, -27.71951656526475460 ) ) ;
#28544 = EDGE_CURVE ( 'NONE', #38824, #5904, #18719, .T. ) ;
#28545 = LINE ( 'NONE', #27949, #25012 ) ;
#28546 = ORIENTED_EDGE ( 'NONE', *, *, #27524, .T. ) ;
#28547 = CARTESIAN_POINT ( 'NONE',  ( -6.451376067920914892, 35.76073122304934060, 10.94387467463487873 ) ) ;
#28548 = CARTESIAN_POINT ( 'NONE',  ( 9.183240348400453001, 28.21559575157615996, 6.000000000000000000 ) ) ;
#28549 = CARTESIAN_POINT ( 'NONE',  ( 16.71272696259839918, -12.03478187020944645, -28.45356395895326074 ) ) ;
#28550 = AXIS2_PLACEMENT_3D ( 'NONE', #33666, #11916, #25097 ) ;
#28551 = CARTESIAN_POINT ( 'NONE',  ( -12.05736835487443237, 14.38397459621567442, 7.000000000000000000 ) ) ;
#28552 = DIRECTION ( 'NONE',  ( -0.8090169943749504489, -0.5877852522924689183, 0.000000000000000000 ) ) ;
#28553 = DIRECTION ( 'NONE',  ( 0.000000000000000000, 0.000000000000000000, 1.000000000000000000 ) ) ;
#28554 = CARTESIAN_POINT ( 'NONE',  ( 11.08575732160469052, 18.77318094934662795, -23.79130904447407246 ) ) ;
#28555 = CARTESIAN_POINT ( 'NONE',  ( 2.525645716490518389, 8.212903943950921715, 7.000000000000000000 ) ) ;
#28556 = VERTEX_POINT ( 'NONE', #31107 ) ;
#28558 = CARTESIAN_POINT ( 'NONE',  ( 2.629601561899389761, 7.723830143584008212, 10.49999999999999822 ) ) ;
#28557 = CARTESIAN_POINT ( 'NONE',  ( -18.44765746950383800, 17.30723153088500155, -9.360930369442520771 ) ) ;
#28559 = CARTESIAN_POINT ( 'NONE',  ( 28.24711154207322750, -27.09388640670316661, 11.00000000000010303 ) ) ;
#28560 = CARTESIAN_POINT ( 'NONE',  ( 11.15896920475388043, -20.47308817170501172, -20.54455431084991446 ) ) ;
#28561 = CARTESIAN_POINT ( 'NONE',  ( 12.30736835487432579, 14.81698729810772619, 7.000000000000000000 ) ) ;
#28562 = CARTESIAN_POINT ( 'NONE',  ( 11.07693200130355038, 17.49985971445773458, -27.44810509905307683 ) ) ;
#28563 = ORIENTED_EDGE ( 'NONE', *, *, #34579, .F. ) ;
#28564 = CARTESIAN_POINT ( 'NONE',  ( 14.93061682650073330, 25.81337123915155729, -9.708168291266565220 ) ) ;
#28565 = ORIENTED_EDGE ( 'NONE', *, *, #33374, .T. ) ;
#28566 = DIRECTION ( 'NONE',  ( 0.9510565162951544194, 0.3090169943749450643, 0.000000000000000000 ) ) ;
#28567 = CARTESIAN_POINT ( 'NONE',  ( -9.575915756022620684, -18.36279351651394620, -27.45102388653645065 ) ) ;
#28568 = CARTESIAN_POINT ( 'NONE',  ( -34.78244346405214316, -1.681994768166323428, 12.14047268033058558 ) ) ;
#28569 = AXIS2_PLACEMENT_3D ( 'NONE', #27598, #9517, #3409 ) ;
#28570 = CARTESIAN_POINT ( 'NONE',  ( -30.73942927727400232, -22.61273690771325917, -5.858838859916063235 ) ) ;
#28571 = CARTESIAN_POINT ( 'NONE',  ( -4.793034356438155008, -24.87474678070748269, -6.447031815283989609 ) ) ;
#28572 = CARTESIAN_POINT ( 'NONE',  ( 15.71155925927456742, 25.50991634872312730, -6.418619526760371841 ) ) ;
#28573 = ORIENTED_EDGE ( 'NONE', *, *, #17159, .F. ) ;
#28574 = CARTESIAN_POINT ( 'NONE',  ( 20.22334892891204561, 9.255629639704887168, -19.04855246831971982 ) ) ;
#28575 = DIRECTION ( 'NONE',  ( 0.8090169943749510040, 0.5877852522924683631, 0.000000000000000000 ) ) ;
#28576 = CARTESIAN_POINT ( 'NONE',  ( 14.52022913576961116, 28.28138333486318601, 16.87380292611584665 ) ) ;
#28577 = ORIENTED_EDGE ( 'NONE', *, *, #29376, .T. ) ;
#28578 = CARTESIAN_POINT ( 'NONE',  ( -20.28315073442723460, -3.046437751679770933, -29.27849696980957717 ) ) ;
#28579 = CARTESIAN_POINT ( 'NONE',  ( -27.71565130972192392, -3.171757977838549625, 19.66345542862528717 ) ) ;
#28580 = ORIENTED_EDGE ( 'NONE', *, *, #2395, .F. ) ;
#28581 = FACE_OUTER_BOUND ( 'NONE', #27647, .T. ) ;
#28582 = CARTESIAN_POINT ( 'NONE',  ( 24.51445621669102692, -11.16206880503134080, 23.00000000000000355 ) ) ;
#28583 = EDGE_CURVE ( 'NONE', #25424, #25284, #3668, .T. ) ;
#28584 = AXIS2_PLACEMENT_3D ( 'NONE', #31897, #16467, #7304 ) ;
#28585 = CARTESIAN_POINT ( 'NONE',  ( -25.39634053522611623, 1.114860656254929028, -16.51261428875549697 ) ) ;
#28586 = CARTESIAN_POINT ( 'NONE',  ( 21.10775083282109676, -8.526917100706684849, -23.04258616691868511 ) ) ;
#28587 = CARTESIAN_POINT ( 'NONE',  ( 32.18944385490208759, 1.219497045963512827, 12.73282698324853257 ) ) ;
#28588 = ORIENTED_EDGE ( 'NONE', *, *, #34124, .T. ) ;
#28589 = ORIENTED_EDGE ( 'NONE', *, *, #8528, .F. ) ;
#28590 = FACE_OUTER_BOUND ( 'NONE', #18476, .T. ) ;
#28591 = DIRECTION ( 'NONE',  ( 0.000000000000000000, 0.000000000000000000, 1.000000000000000000 ) ) ;
#28592 = AXIS2_PLACEMENT_3D ( 'NONE', #10412, #16716, #35192 ) ;
#28593 = CARTESIAN_POINT ( 'NONE',  ( 1.247466774197339978, 28.36888560440311480, 6.000000000000000000 ) ) ;
#28594 = EDGE_LOOP ( 'NONE', ( #6204, #33847, #16806, #23876 ) ) ;
#28595 = CARTESIAN_POINT ( 'NONE',  ( -1.044308797982332448, 21.12605994883989879, -26.25946094505387407 ) ) ;
#28596 = AXIS2_PLACEMENT_3D ( 'NONE', #20473, #33273, #5223 ) ;
#28597 = DIRECTION ( 'NONE',  ( -0.4999999999999920064, 0.8660254037844432595, 0.000000000000000000 ) ) ;
#28598 = FACE_OUTER_BOUND ( 'NONE', #23589, .T. ) ;
#28599 = CARTESIAN_POINT ( 'NONE',  ( -12.11016527260154163, 31.83082137946488643, 7.000000000000000000 ) ) ;
#28600 = CARTESIAN_POINT ( 'NONE',  ( 20.23296131041715640, 28.12381335138032412, 0.000000000000000000 ) ) ;
#28601 = DIRECTION ( 'NONE',  ( -0.000000000000000000, -0.000000000000000000, -1.000000000000000000 ) ) ;
#28602 = CARTESIAN_POINT ( 'NONE',  ( 13.99156332179505569, 29.21683596761936741, -8.194172333430742583 ) ) ;
#28603 = CARTESIAN_POINT ( 'NONE',  ( 13.63581098909226874, 27.45627467658428955, 7.500000000000000888 ) ) ;
#28604 = EDGE_LOOP ( 'NONE', ( #38405, #25693, #3535, #9301, #8714, #20110, #5338, #23322, #11065, #15505 ) ) ;
#28606 = DIRECTION ( 'NONE',  ( -0.000000000000000000, -0.000000000000000000, -1.000000000000000000 ) ) ;
#28605 = CARTESIAN_POINT ( 'NONE',  ( -19.96221307476523421, 10.82707266035624372, -16.98081666870033146 ) ) ;
#28607 = CARTESIAN_POINT ( 'NONE',  ( 0.000000000000000000, 22.50000000000000355, 6.000000000000000000 ) ) ;
#28608 = ADVANCED_FACE ( 'NONE', ( #37604 ), #3866, .T. ) ;
#28609 = CARTESIAN_POINT ( 'NONE',  ( 14.93595915082604186, -25.84735051801111894, -9.705674759444587352 ) ) ;
#28610 = DIRECTION ( 'NONE',  ( -0.000000000000000000, -0.000000000000000000, 1.000000000000000000 ) ) ;
#28611 = VECTOR ( 'NONE', #19061, 1000.000000000000000 ) ;
#28612 = CARTESIAN_POINT ( 'NONE',  ( 13.17886393423189162, 22.29227785210140311, -16.43698232960724681 ) ) ;
#28613 = CARTESIAN_POINT ( 'NONE',  ( -12.33616729053607486, -27.99489201236593061, -13.58461195433496194 ) ) ;
#28614 = CARTESIAN_POINT ( 'NONE',  ( 13.47830981910552239, 21.58612669357077607, 9.500000000000000000 ) ) ;
#28615 = CARTESIAN_POINT ( 'NONE',  ( -20.53646817104797506, -21.76128887135726231, -14.90463942194158520 ) ) ;
#28616 = CARTESIAN_POINT ( 'NONE',  ( 8.419895509524939925, -25.16897077364957269, -7.395897382025212075 ) ) ;
#28617 = CARTESIAN_POINT ( 'NONE',  ( 12.51756012225011894, 20.32411358514038113, -19.51841735849092174 ) ) ;
#28618 = CARTESIAN_POINT ( 'NONE',  ( 30.90226151228388574, -22.30983874898413788, -6.280244427829897447 ) ) ;
#28619 = CARTESIAN_POINT ( 'NONE',  ( -75.15099915297791711, 43.38844959084113384, 2.999999999999999112 ) ) ;
#28620 = CARTESIAN_POINT ( 'NONE',  ( 14.31603901957230462, 19.98981538725069740, 11.00000000000000000 ) ) ;
#28621 = B_SPLINE_CURVE_WITH_KNOTS ( 'NONE', 3,
 ( #9206, #3108, #15899, #27888, #22183, #24839, #463, #6736, #25428, #18551, #37825, #3504, #3304, #15501, #37434, #24640, #21590, #60, #5951, #15298, #37237, #6344, #34191, #6540, #30748, #21989, #9608, #18751, #15694, #262, #12649, #25037, #34389, #18945, #12847, #38234, #34991, #25835, #25629, #29088, #35593, #7140, #38027, #26034, #19747, #10201, #29292, #10405, #7750, #26239, #7549, #1061, #19342, #10606, #3899, #28885, #1462, #13847, #13238, #4099 ),
 .UNSPECIFIED., .F., .F.,
 ( 4, 2, 2, 2, 2, 2, 2, 2, 2, 2, 2, 2, 2, 2, 2, 2, 2, 2, 2, 2, 2, 2, 2, 2, 2, 2, 2, 2, 2, 4 ),
 ( 0.000000000000000000, 0.004090388079386704165, 0.006135582119080056247, 0.008180776158773408330, 0.01227116423816010903, 0.01329376125800678550, 0.01431635827785346024, 0.01636155231754680972, 0.02045194039693351215, 0.02249713443662685469, 0.02454232847632019723, 0.02658752251601354671, 0.02863271655570688926, 0.03272310463509358475, 0.03374570165494025775, 0.03476829867478693076, 0.03681349271448028371, 0.04090388079386698961, 0.04192647781371366261, 0.04294907483356033562, 0.04499426887325368857, 0.04703946291294704152, 0.04908465695264038753, 0.05317504503202709343, 0.05522023907172043944, 0.05726543311141379239, 0.06135582119080049829, 0.06237841821064717823, 0.06340101523049386512, 0.06544620927018722500 ),
 .UNSPECIFIED. ) ;
#28622 = ORIENTED_EDGE ( 'NONE', *, *, #29626, .F. ) ;
#28623 = CARTESIAN_POINT ( 'NONE',  ( -8.411768547097867810, 35.89333961072667023, -6.727922225057652028 ) ) ;
#28624 = AXIS2_PLACEMENT_3D ( 'NONE', #22149, #6702, #16060 ) ;
#28625 = CARTESIAN_POINT ( 'NONE',  ( 14.51883047965004891, 21.47676356526602959, 10.99999999999999289 ) ) ;
#28626 = VERTEX_POINT ( 'NONE', #12810 ) ;
#28627 = CARTESIAN_POINT ( 'NONE',  ( 23.94456298200180910, 0.4764677600133929158, -19.49540907187814298 ) ) ;
#28628 = AXIS2_PLACEMENT_3D ( 'NONE', #33162, #8366, #27247 ) ;
#28629 = LINE ( 'NONE', #7697, #17425 ) ;
#28630 = EDGE_CURVE ( 'NONE', #22096, #19611, #28449, .T. ) ;
#28631 = CARTESIAN_POINT ( 'NONE',  ( -31.24272016124700713, 0.2902395683534712556, 15.72805884748939143 ) ) ;
#28632 = ORIENTED_EDGE ( 'NONE', *, *, #37178, .F. ) ;
#28633 = CARTESIAN_POINT ( 'NONE',  ( -20.60555239772964242, 0.9311154778176756741, -28.08151642131643655 ) ) ;
#28634 = DIRECTION ( 'NONE',  ( 1.000000000000000000, 0.000000000000000000, 0.000000000000000000 ) ) ;
#28635 = VERTEX_POINT ( 'NONE', #30907 ) ;
#28636 = CARTESIAN_POINT ( 'NONE',  ( 29.16726107428658565, -7.828744422222867705, -14.86866462477206419 ) ) ;
#28637 = ADVANCED_FACE ( 'NONE', ( #25206 ), #9773, .F. ) ;
#28638 = ORIENTED_EDGE ( 'NONE', *, *, #13515, .T. ) ;
#28639 = CIRCLE ( 'NONE', #36450, 15.00000000000000000 ) ;
#28640 = CARTESIAN_POINT ( 'NONE',  ( -1.473879933410623262E-13, 40.50000000000004974, 11.55979286843934872 ) ) ;
#28641 = EDGE_CURVE ( 'NONE', #3294, #6428, #20158, .T. ) ;
#28642 = FACE_OUTER_BOUND ( 'NONE', #13108, .T. ) ;
#28643 = CARTESIAN_POINT ( 'NONE',  ( 5.706335727061685681, 24.35410196624994583, 13.00000000000000178 ) ) ;
#28644 = CARTESIAN_POINT ( 'NONE',  ( -2.660873612011868339, 34.56296969693360666, 19.27171037444157875 ) ) ;
#28645 = CARTESIAN_POINT ( 'NONE',  ( -0.5000000000000005551, 31.00000000000000355, 9.000000000000001776 ) ) ;
#28646 = ORIENTED_EDGE ( 'NONE', *, *, #5903, .F. ) ;
#28647 = DIRECTION ( 'NONE',  ( 0.9781476007338042455, -0.2079116908177656431, 0.000000000000000000 ) ) ;
#28648 = LINE ( 'NONE', #3470, #29904 ) ;
#28649 = CARTESIAN_POINT ( 'NONE',  ( -8.927394655428429360, 11.06314620770957013, 7.500000000000000888 ) ) ;
#28650 = CARTESIAN_POINT ( 'NONE',  ( 18.14143768169351034, 18.99352574702872687, -5.478296980462506127 ) ) ;
#28651 = CARTESIAN_POINT ( 'NONE',  ( 5.348610690096846199, 23.76848409712731325, -20.84344495567194500 ) ) ;
#28652 = AXIS2_PLACEMENT_3D ( 'NONE', #32308, #8113, #16465 ) ;
#28653 = ORIENTED_EDGE ( 'NONE', *, *, #36473, .T. ) ;
#28654 = EDGE_CURVE ( 'NONE', #4036, #10907, #3471, .T. ) ;
#28655 = EDGE_CURVE ( 'NONE', #12503, #5336, #25995, .T. ) ;
#28656 = CARTESIAN_POINT ( 'NONE',  ( 16.27219429315636390, -26.92618254030204383, -5.000000000000002665 ) ) ;
#28657 = DIRECTION ( 'NONE',  ( 0.9135454576426004225, -0.4067366430758009854, 0.000000000000000000 ) ) ;
#28658 = LINE ( 'NONE', #12621, #24521 ) ;
#28659 = ORIENTED_EDGE ( 'NONE', *, *, #9911, .T. ) ;
#28660 = CARTESIAN_POINT ( 'NONE',  ( -11.00242421671864790, 17.29730523913238827, -29.99999999999999645 ) ) ;
#28661 = CARTESIAN_POINT ( 'NONE',  ( -24.21699896819899678, -27.13078975446515528, 15.72805884748972360 ) ) ;
#28662 = CARTESIAN_POINT ( 'NONE',  ( 11.24122865112338410, -21.01550894017544380, -19.52903937763365150 ) ) ;
#28663 = VECTOR ( 'NONE', #29679, 1000.000000000000227 ) ;
#28664 = CYLINDRICAL_SURFACE ( 'NONE', #8200, 1.000000000000000000 ) ;
#28665 = EDGE_LOOP ( 'NONE', ( #9760, #32499, #17557, #29856 ) ) ;
#28666 = ORIENTED_EDGE ( 'NONE', *, *, #13832, .T. ) ;
#28667 = CARTESIAN_POINT ( 'NONE',  ( -12.95981342954301496, 28.24763295269045926, -11.37950637273800325 ) ) ;
#28668 = CARTESIAN_POINT ( 'NONE',  ( -12.99038105676664934, 15.00000000000012257, 7.000000000000000000 ) ) ;
#28669 = FACE_BOUND ( 'NONE', #24604, .T. ) ;
#28670 = CARTESIAN_POINT ( 'NONE',  ( -21.28402897910519442, -4.571266421688831016, -24.49177716778804381 ) ) ;
#28671 = LINE ( 'NONE', #16490, #35877 ) ;
#28672 = ORIENTED_EDGE ( 'NONE', *, *, #4039, .T. ) ;
#28673 = CARTESIAN_POINT ( 'NONE',  ( 21.68786324554740474, 0.8396193639690311405, -23.86711573477778003 ) ) ;
#28674 = FACE_OUTER_BOUND ( 'NONE', #35452, .T. ) ;
#28675 = CARTESIAN_POINT ( 'NONE',  ( -14.44482798346716201, 26.50521816028930999, 7.499999999999993783 ) ) ;
#28676 = ORIENTED_EDGE ( 'NONE', *, *, #35456, .T. ) ;
#28677 = CARTESIAN_POINT ( 'NONE',  ( -20.48278845350746380, 0.8398715278162421916, -29.34801594207987208 ) ) ;
#28678 = EDGE_CURVE ( 'NONE', #1082, #31776, #13673, .T. ) ;
#28679 = CARTESIAN_POINT ( 'NONE',  ( 9.151574469205250750, 1.945227203041362207, 7.000000000000000000 ) ) ;
#28680 = ORIENTED_EDGE ( 'NONE', *, *, #16819, .T. ) ;
#28681 = CARTESIAN_POINT ( 'NONE',  ( 21.08291815013172155, -1.666117999273566186, -26.00856586672298221 ) ) ;
#28682 = CARTESIAN_POINT ( 'NONE',  ( -4.577399223880544099, 35.23960032125098252, 10.00000000000000000 ) ) ;
#28683 = AXIS2_PLACEMENT_3D ( 'NONE', #11032, #4727, #16927 ) ;
#28684 = CARTESIAN_POINT ( 'NONE',  ( 20.64393337882627577, -27.21432092515273382, 16.30093088680190760 ) ) ;
#28685 = ORIENTED_EDGE ( 'NONE', *, *, #37332, .T. ) ;
#28686 = CARTESIAN_POINT ( 'NONE',  ( 3.569741787452879400, 38.68155838841062888, 15.72805884748945360 ) ) ;
#28687 = ADVANCED_FACE ( 'NONE', ( #9574 ), #13006, .T. ) ;
#28688 = DIRECTION ( 'NONE',  ( -0.000000000000000000, -0.000000000000000000, -1.000000000000000000 ) ) ;
#28689 = CARTESIAN_POINT ( 'NONE',  ( 3.503066876655847040, 27.10955750621999982, 20.99999999999999645 ) ) ;
#28690 = DIRECTION ( 'NONE',  ( 1.000000000000000000, 0.000000000000000000, 0.000000000000000000 ) ) ;
#28691 = CIRCLE ( 'NONE', #29341, 0.9999999999999970024 ) ;
#28692 = CARTESIAN_POINT ( 'NONE',  ( -10.47804177580193041, 33.28010392086039104, 10.49999999999999822 ) ) ;
#28693 = FACE_BOUND ( 'NONE', #18749, .T. ) ;
#28694 = CARTESIAN_POINT ( 'NONE',  ( 17.35626706996901092, 16.20628521381938469, 17.92354375535268929 ) ) ;
#28695 = CARTESIAN_POINT ( 'NONE',  ( -21.15495209035839963, 9.289218443130405234, -15.92845176507750793 ) ) ;
#28696 = ADVANCED_FACE ( 'NONE', ( #13007 ), #36395, .T. ) ;
#28697 = CARTESIAN_POINT ( 'NONE',  ( 17.25312817826965883, -20.19401662141811116, -17.91462702624227532 ) ) ;
#28698 = CARTESIAN_POINT ( 'NONE',  ( 13.46929972531963848, 26.35070966310165375, 9.500000000000000000 ) ) ;
#28699 = ORIENTED_EDGE ( 'NONE', *, *, #30211, .T. ) ;
#28700 = EDGE_CURVE ( 'NONE', #13627, #33602, #18874, .T. ) ;
#28701 = CARTESIAN_POINT ( 'NONE',  ( 10.88003517233900297, 17.37455259072008573, -29.34610220216738696 ) ) ;
#28702 = EDGE_LOOP ( 'NONE', ( #1948, #35030, #23568, #16039 ) ) ;
#28703 = CARTESIAN_POINT ( 'NONE',  ( -15.22475464391910549, 24.92285436334850601, -9.722768853599610850 ) ) ;
#28704 = CARTESIAN_POINT ( 'NONE',  ( -29.45937559703918751, -11.06631500863563922, 20.25080042701617344 ) ) ;
#28705 = CARTESIAN_POINT ( 'NONE',  ( 10.32110986824234544, 33.06327772184302205, 10.49999999999999822 ) ) ;
#28706 = CARTESIAN_POINT ( 'NONE',  ( 11.34078712063792160, 18.01401842891820948, -25.01870591048817261 ) ) ;
#28707 = VERTEX_POINT ( 'NONE', #22150 ) ;
#28708 = CARTESIAN_POINT ( 'NONE',  ( 25.87747567411906502, -13.26005397570095035, -16.62966469873034114 ) ) ;
#28709 = CARTESIAN_POINT ( 'NONE',  ( -19.48557158514988785, -11.24999999999987743, 6.000000000000000000 ) ) ;
#28710 = VERTEX_POINT ( 'NONE', #22346 ) ;
#28712 = DIRECTION ( 'NONE',  ( -0.000000000000000000, -0.000000000000000000, -1.000000000000000000 ) ) ;
#28711 = CARTESIAN_POINT ( 'NONE',  ( -15.27795965409528556, 27.25395738312943195, -5.000000000000000888 ) ) ;
#28713 = CARTESIAN_POINT ( 'NONE',  ( -10.10041478618032151, -18.75911771733305144, -24.99883724396762474 ) ) ;
#28714 = CARTESIAN_POINT ( 'NONE',  ( 9.151574469205250750, 1.945227203041362207, 11.00000000000000000 ) ) ;
#28715 = CIRCLE ( 'NONE', #15753, 1.000000000000000000 ) ;
#28716 = ORIENTED_EDGE ( 'NONE', *, *, #34900, .T. ) ;
#28717 = CARTESIAN_POINT ( 'NONE',  ( -19.51443761669260013, -8.089147095777512675, -26.29262032055718734 ) ) ;
#28718 = CARTESIAN_POINT ( 'NONE',  ( -9.200702945070620586, -18.66544396913702286, -26.87043342310872518 ) ) ;
#28719 = DIRECTION ( 'NONE',  ( 1.000000000000000000, 0.000000000000000000, 0.000000000000000000 ) ) ;
#28720 = CARTESIAN_POINT ( 'NONE',  ( 16.07775879733624080, 22.56051826075340827, -9.762945716588777856 ) ) ;
#28721 = ORIENTED_EDGE ( 'NONE', *, *, #7146, .T. ) ;
#28722 = CARTESIAN_POINT ( 'NONE',  ( 20.01208193039519756, 4.507116686654149440, -30.00000000000000355 ) ) ;
#28723 = CARTESIAN_POINT ( 'NONE',  ( -2.587667106213709101, 35.31811204475769728, 12.00000000000000000 ) ) ;
#28724 = ORIENTED_EDGE ( 'NONE', *, *, #27998, .F. ) ;
#28725 = CARTESIAN_POINT ( 'NONE',  ( -31.18229473435558319, -0.3319675162687186210, -5.472313823790837084 ) ) ;
#28726 = EDGE_CURVE ( 'NONE', #18134, #15610, #37202, .T. ) ;
#28727 = CARTESIAN_POINT ( 'NONE',  ( 31.12965019444430226, -0.3871312522807165979, -6.409569423096037610 ) ) ;
#28728 = VECTOR ( 'NONE', #6724, 1000.000000000000000 ) ;
#28729 = EDGE_CURVE ( 'NONE', #14474, #21424, #684, .T. ) ;
#28730 = CARTESIAN_POINT ( 'NONE',  ( 24.71109915377187605, -20.69862126830684801, 19.99202127657072481 ) ) ;
#28731 = ORIENTED_EDGE ( 'NONE', *, *, #30354, .F. ) ;
#28732 = CARTESIAN_POINT ( 'NONE',  ( -5.636483973512888213, -22.01575377102104270, -21.50719306941231679 ) ) ;
#28733 = AXIS2_PLACEMENT_3D ( 'NONE', #9273, #22056, #34455 ) ;
#28734 = CARTESIAN_POINT ( 'NONE',  ( -8.312041872459065672, 25.58773265502866678, 13.00000000000000178 ) ) ;
#28735 = EDGE_CURVE ( 'NONE', #19934, #20723, #29451, .T. ) ;
#28736 = ORIENTED_EDGE ( 'NONE', *, *, #9616, .T. ) ;
#28737 = FACE_OUTER_BOUND ( 'NONE', #12864, .T. ) ;
#28738 = VECTOR ( 'NONE', #29260, 1000.000000000000000 ) ;
#28739 = DIRECTION ( 'NONE',  ( 0.9135454576426059736, 0.4067366430757888285, 0.000000000000000000 ) ) ;
#28740 = CARTESIAN_POINT ( 'NONE',  ( 24.10033869685532082, 8.113510327255378130, -5.000000000000000888 ) ) ;
#28741 = DIRECTION ( 'NONE',  ( 0.000000000000000000, 0.000000000000000000, 1.000000000000000000 ) ) ;
#28742 = ORIENTED_EDGE ( 'NONE', *, *, #14385, .T. ) ;
#28743 = CARTESIAN_POINT ( 'NONE',  ( -14.47283171447380390, 21.48159823030330884, 7.000000000000000000 ) ) ;
#28744 = AXIS2_PLACEMENT_3D ( 'NONE', #1091, #4330, #16127 ) ;
#28745 = CARTESIAN_POINT ( 'NONE',  ( -12.80736835487441816, 15.68301270189233243, 11.00000000000000000 ) ) ;
#28746 = CARTESIAN_POINT ( 'NONE',  ( 21.57777642674768614, -18.77388931612815171, -16.71433531468114708 ) ) ;
#28747 = ADVANCED_FACE ( 'NONE', ( #13609 ), #4609, .T. ) ;
#28748 = ADVANCED_FACE ( 'NONE', ( #35355 ), #1630, .F. ) ;
#28749 = CARTESIAN_POINT ( 'NONE',  ( 8.633502029282041690, 11.46765470489692795, 7.000000000000000000 ) ) ;
#28750 = DIRECTION ( 'NONE',  ( 0.9781476007338043566, -0.2079116908177657264, 0.000000000000000000 ) ) ;
#28751 = ADVANCED_FACE ( 'NONE', ( #7107 ), #4266, .F. ) ;
#28752 = CARTESIAN_POINT ( 'NONE',  ( 14.64031184850172806, 26.19941073413151500, -10.14528853390185859 ) ) ;
#28753 = CARTESIAN_POINT ( 'NONE',  ( 13.13294332834914790, 16.07239217250469920, 10.49999999999999645 ) ) ;
#28754 = ORIENTED_EDGE ( 'NONE', *, *, #36102, .F. ) ;
#28755 = AXIS2_PLACEMENT_3D ( 'NONE', #34649, #3763, #10265 ) ;
#28757 = CARTESIAN_POINT ( 'NONE',  ( -11.11016527260153808, 31.83082137946488643, 9.000000000000001776 ) ) ;
#28756 = CARTESIAN_POINT ( 'NONE',  ( -14.53439070480614603, 14.74270464415775628, -27.08252300681113667 ) ) ;
#28758 = CARTESIAN_POINT ( 'NONE',  ( -13.31203413219588505, 15.58674249317294525, 7.489426592562537621 ) ) ;
#28759 = CARTESIAN_POINT ( 'NONE',  ( 13.35281424139188999, -23.62076856857055063, -14.47731724256479247 ) ) ;
#28760 = CYLINDRICAL_SURFACE ( 'NONE', #26294, 17.99999999999992895 ) ;
#28761 = CARTESIAN_POINT ( 'NONE',  ( 15.02387404494793088, 25.95058579368609841, -9.238541711895710051 ) ) ;
#28762 = ORIENTED_EDGE ( 'NONE', *, *, #30757, .F. ) ;
#28763 = CARTESIAN_POINT ( 'NONE',  ( 12.38717450789916974, 20.49561646409227578, -19.49553371946326763 ) ) ;
#28764 = EDGE_LOOP ( 'NONE', ( #16193, #13827, #28653, #31876 ) ) ;
#28766 = LINE ( 'NONE', #22464, #8846 ) ;
#28765 = CARTESIAN_POINT ( 'NONE',  ( -12.61875268155488961, 21.10517070559246378, -18.44458008985245456 ) ) ;
#28767 = CARTESIAN_POINT ( 'NONE',  ( -15.27591890422142740, -26.49336055367123066, -7.358011338661719414 ) ) ;
#28768 = VECTOR ( 'NONE', #2339, 1000.000000000000000 ) ;
#28769 = CARTESIAN_POINT ( 'NONE',  ( -32.09165771328245853, 1.123514972296517422, 13.32518128616608699 ) ) ;
#28770 = CARTESIAN_POINT ( 'NONE',  ( -29.20118438018936757, -21.52094793055072230, -9.738337299848499384 ) ) ;
#28771 = VECTOR ( 'NONE', #121, 1000.000000000000114 ) ;
#28772 = CARTESIAN_POINT ( 'NONE',  ( -3.274116759621854111, -20.28896347757955354, -30.00000000000000000 ) ) ;
#28773 = CARTESIAN_POINT ( 'NONE',  ( 12.28356143704143477, 18.96473258983586518, -21.68345190119157806 ) ) ;
#28774 = ORIENTED_EDGE ( 'NONE', *, *, #3542, .F. ) ;
#28775 = CARTESIAN_POINT ( 'NONE',  ( 24.01170615723790647, 8.305688554546300395, -5.962680836947249041 ) ) ;
#28776 = CARTESIAN_POINT ( 'NONE',  ( 4.331888841169166504, 42.14502281828541896, 11.00000000000000000 ) ) ;
#28777 = CARTESIAN_POINT ( 'NONE',  ( -3.110808594360106927, 36.60201144129489137, 17.92354375535252586 ) ) ;
#28778 = ORIENTED_EDGE ( 'NONE', *, *, #38848, .F. ) ;
#28779 = CARTESIAN_POINT ( 'NONE',  ( -20.53764066314045778, -2.436979956095350897, -27.91568385910457906 ) ) ;
#28780 = EDGE_CURVE ( 'NONE', #38309, #2164, #33160, .T. ) ;
#28781 = VECTOR ( 'NONE', #31454, 999.9999999999998863 ) ;
#28782 = CARTESIAN_POINT ( 'NONE',  ( -15.42165057838969666, 26.78649484828442695, 16.30093088680190405 ) ) ;
#28783 = ORIENTED_EDGE ( 'NONE', *, *, #1665, .T. ) ;
#28784 = EDGE_CURVE ( 'NONE', #22892, #1139, #21853, .T. ) ;
#28785 = CARTESIAN_POINT ( 'NONE',  ( 18.76090689389213395, -16.22676322417229500, 20.99999999999999645 ) ) ;
#28786 = PRODUCT_DEFINITION_FORMATION_WITH_SPECIFIED_SOURCE ( 'ANY', '', #37908, .NOT_KNOWN. ) ;
#28787 = FACE_OUTER_BOUND ( 'NONE', #15293, .T. ) ;
#28788 = CARTESIAN_POINT ( 'NONE',  ( 34.65956455088738153, -16.45432426470986798, -5.436012016185657103 ) ) ;
#28789 = CARTESIAN_POINT ( 'NONE',  ( 33.64699323788449448, -0.06984207429561786751, 12.14047268033164073 ) ) ;
#28790 = ORIENTED_EDGE ( 'NONE', *, *, #25883, .T. ) ;
#28791 = ORIENTED_EDGE ( 'NONE', *, *, #24041, .T. ) ;
#28792 = PLANE ( 'NONE',  #8702 ) ;
#28793 = DIRECTION ( 'NONE',  ( 0.000000000000000000, 0.000000000000000000, 1.000000000000000000 ) ) ;
#28794 = DIRECTION ( 'NONE',  ( 1.000000000000000000, 0.000000000000000000, 0.000000000000000000 ) ) ;
#28795 = ORIENTED_EDGE ( 'NONE', *, *, #11640, .T. ) ;
#28796 = VECTOR ( 'NONE', #26252, 1000.000000000000114 ) ;
#28797 = CARTESIAN_POINT ( 'NONE',  ( -1.457936558815239314, 29.04007097956189654, -16.62967044460848598 ) ) ;
#28798 = CARTESIAN_POINT ( 'NONE',  ( -30.90412082983564446, -0.04211290444597337590, -5.000000000000000888 ) ) ;
#28799 = CARTESIAN_POINT ( 'NONE',  ( 1.494936919103933226, 34.23777120880591696, 12.00000000000000000 ) ) ;
#28800 = DIRECTION ( 'NONE',  ( 0.000000000000000000, 0.000000000000000000, 1.000000000000000000 ) ) ;
#28801 = CARTESIAN_POINT ( 'NONE',  ( 8.315274455032101386, 10.01576150750513250, 7.500000000000000888 ) ) ;
#28802 = LINE ( 'NONE', #18867, #28781 ) ;
#28803 = AXIS2_PLACEMENT_3D ( 'NONE', #33773, #21961, #18522 ) ;
#28804 = CARTESIAN_POINT ( 'NONE',  ( 13.32202332345313067, 27.64393215917316482, -11.41592897530081707 ) ) ;
#28805 = DIRECTION ( 'NONE',  ( 1.000000000000000000, 0.000000000000000000, 0.000000000000000000 ) ) ;
#28806 = ORIENTED_EDGE ( 'NONE', *, *, #39443, .F. ) ;
#28808 = CARTESIAN_POINT ( 'NONE',  ( -19.60875595791377535, 15.93339349895804169, 10.00000000000000000 ) ) ;
#28807 = CARTESIAN_POINT ( 'NONE',  ( -18.97453683301921856, 13.61319736012170445, -14.90564131719889218 ) ) ;
#28809 = AXIS2_PLACEMENT_3D ( 'NONE', #9220, #27901, #21605 ) ;
#28810 = CARTESIAN_POINT ( 'NONE',  ( 4.331888854854090809, 42.14502281367550296, 11.00000000000000000 ) ) ;
#28811 = PRODUCT_DEFINITION_FORMATION_WITH_SPECIFIED_SOURCE ( 'ANY', '', #939, .NOT_KNOWN. ) ;
#28812 = CARTESIAN_POINT ( 'NONE',  ( 9.532625661562562414, -18.14880370279404076, -29.34763336998847905 ) ) ;
#28813 = CARTESIAN_POINT ( 'NONE',  ( -8.737320611644010526, -1.152986690174108819, 7.000000000000000000 ) ) ;
#28814 = CARTESIAN_POINT ( 'NONE',  ( 15.34998332328284931, 26.75042238537495720, -6.415952016425999993 ) ) ;
#28815 = CARTESIAN_POINT ( 'NONE',  ( -21.88499642459564498, -5.528038495964382015, -20.11584339644715413 ) ) ;
#28816 = CARTESIAN_POINT ( 'NONE',  ( -18.76572289696387941, -16.22800572947405584, 23.00000000000000355 ) ) ;
#28817 = AXIS2_PLACEMENT_3D ( 'NONE', #9262, #6208, #14260 ) ;
#28818 = CARTESIAN_POINT ( 'NONE',  ( -24.91750628164249903, -24.86351076958389328, -9.360757952822334360 ) ) ;
#28819 = CARTESIAN_POINT ( 'NONE',  ( 6.046104871185695728, -24.56383547664059819, -9.847241658924353658 ) ) ;
#28820 = CARTESIAN_POINT ( 'NONE',  ( 15.42174346112090966, 26.32695858896734364, -6.888516504560381115 ) ) ;
#28821 = CARTESIAN_POINT ( 'NONE',  ( 31.56478557840102539, -21.36326414210120817, -6.699604253589384051 ) ) ;
#28822 = CARTESIAN_POINT ( 'NONE',  ( -19.48557158514998022, -11.24999999999982414, 0.000000000000000000 ) ) ;
#28823 = CARTESIAN_POINT ( 'NONE',  ( 6.348106467989403257, 35.16482219193073178, 6.000000000000000000 ) ) ;
#28824 = EDGE_LOOP ( 'NONE', ( #9513, #11207, #30281, #27277 ) ) ;
#28825 = CARTESIAN_POINT ( 'NONE',  ( -8.315359605991371694, 35.38416871997877422, -8.021598471839368472 ) ) ;
#28826 = AXIS2_PLACEMENT_3D ( 'NONE', #4723, #17129, #29505 ) ;
#28827 = FACE_OUTER_BOUND ( 'NONE', #2301, .T. ) ;
#28828 = ORIENTED_EDGE ( 'NONE', *, *, #13359, .F. ) ;
#28829 = CARTESIAN_POINT ( 'NONE',  ( 20.48245044547724447, 0.8483310608570678868, -29.34817008848411035 ) ) ;
#28830 = DIRECTION ( 'NONE',  ( 0.000000000000000000, 0.000000000000000000, 1.000000000000000000 ) ) ;
#28831 = CARTESIAN_POINT ( 'NONE',  ( 13.95683075005237050, 28.08631143191933432, 11.00000000000000000 ) ) ;
#28832 = ORIENTED_EDGE ( 'NONE', *, *, #12356, .F. ) ;
#28833 = CARTESIAN_POINT ( 'NONE',  ( -28.25918702355578915, 0.2404301350531496129, -12.55492373771259373 ) ) ;
#28834 = FACE_OUTER_BOUND ( 'NONE', #20672, .T. ) ;
#28835 = ORIENTED_EDGE ( 'NONE', *, *, #17489, .T. ) ;
#28836 = CARTESIAN_POINT ( 'NONE',  ( 33.69202569405961611, -9.057028871410325976, -9.807891961042667361 ) ) ;
#28837 = AXIS2_PLACEMENT_3D ( 'NONE', #26412, #11384, #20925 ) ;
#28838 = EDGE_LOOP ( 'NONE', ( #2618, #34786, #37614, #4846 ) ) ;
#28839 = DIRECTION ( 'NONE',  ( 1.000000000000000000, 0.000000000000000000, 0.000000000000000000 ) ) ;
#28840 = CARTESIAN_POINT ( 'NONE',  ( 0.000000000000000000, 22.50000000000000355, 7.000000000000000000 ) ) ;
#28841 = DIRECTION ( 'NONE',  ( 0.9781476007338042455, -0.2079116908177664758, 0.000000000000000000 ) ) ;
#28842 = LINE ( 'NONE', #1020, #24020 ) ;
#28843 = CARTESIAN_POINT ( 'NONE',  ( -9.574495036671709640E-14, 34.03222469610383882, 19.66345542862528362 ) ) ;
#28844 = CIRCLE ( 'NONE', #39232, 21.00000000000001776 ) ;
#28845 = CARTESIAN_POINT ( 'NONE',  ( -11.54200800595901555, 31.54683795827741122, 10.49999999999999645 ) ) ;
#28846 = ORIENTED_EDGE ( 'NONE', *, *, #27356, .F. ) ;
#28847 = SURFACE_SIDE_STYLE ('',( #16462 ) ) ;
#28848 = CARTESIAN_POINT ( 'NONE',  ( 10.44103466624280507, 32.57396620494213124, 7.000000000000000000 ) ) ;
#28849 = FACE_OUTER_BOUND ( 'NONE', #32083, .T. ) ;
#28850 = CARTESIAN_POINT ( 'NONE',  ( 14.36830325120613594, 20.48707633493483371, 7.000000000000000000 ) ) ;
#28851 = CARTESIAN_POINT ( 'NONE',  ( 16.49490170946486955, 16.68252506057627116, -16.84766835659840112 ) ) ;
#28852 = CARTESIAN_POINT ( 'NONE',  ( 6.411709375437181002, 19.84076997167131751, -27.13309934696545511 ) ) ;
#28853 = ORIENTED_EDGE ( 'NONE', *, *, #14027, .T. ) ;
#28854 = CARTESIAN_POINT ( 'NONE',  ( 0.5000000000000035527, 32.50000000000000000, 10.50000000000000178 ) ) ;
#28855 = LINE ( 'NONE', #38203, #21415 ) ;
#28856 = EDGE_CURVE ( 'NONE', #36455, #22772, #20119, .T. ) ;
#28857 = CARTESIAN_POINT ( 'NONE',  ( 10.71550314065649800, -18.98782435281344405, -23.79126320886110690 ) ) ;
#28858 = DIRECTION ( 'NONE',  ( 1.000000000000000000, 0.000000000000000000, 0.000000000000000000 ) ) ;
#28859 = DIRECTION ( 'NONE',  ( 0.000000000000000000, 0.000000000000000000, 1.000000000000000000 ) ) ;
#28860 = CIRCLE ( 'NONE', #18493, 0.5000000000000004441 ) ;
#28861 = ORIENTED_EDGE ( 'NONE', *, *, #8388, .F. ) ;
#28862 = CARTESIAN_POINT ( 'NONE',  ( -12.39972473649186568, 20.47873198151344454, -19.49820881543729101 ) ) ;
#28863 = CARTESIAN_POINT ( 'NONE',  ( -30.06723386280177124, -23.25956985441318636, 16.30093088680191116 ) ) ;
#28864 = CARTESIAN_POINT ( 'NONE',  ( 12.88792179439757568, -23.58175436233876709, -14.50283011526977361 ) ) ;
#28865 = EDGE_CURVE ( 'NONE', #12427, #9089, #4868, .T. ) ;
#28866 = DIRECTION ( 'NONE',  ( -0.8660254037844364872, 0.5000000000000038858, 0.000000000000000000 ) ) ;
#28867 = EDGE_CURVE ( 'NONE', #12667, #8857, #8497, .T. ) ;
#28868 = ORIENTED_EDGE ( 'NONE', *, *, #10861, .T. ) ;
#28869 = ORIENTED_EDGE ( 'NONE', *, *, #189, .F. ) ;
#28870 = CARTESIAN_POINT ( 'NONE',  ( -11.58530453518540959, 27.01100725576757355, -14.14221114289041381 ) ) ;
#28871 = MECHANICAL_DESIGN_GEOMETRIC_PRESENTATION_REPRESENTATION (  '', ( #976 ), #4217 ) ;
#28872 = DIRECTION ( 'NONE',  ( 0.000000000000000000, 0.000000000000000000, 1.000000000000000000 ) ) ;
#28873 = FACE_BOUND ( 'NONE', #37141, .T. ) ;
#28874 = CARTESIAN_POINT ( 'NONE',  ( -29.93877630219436625, -6.466002002613472577, -13.99053332719549658 ) ) ;
#28875 = CARTESIAN_POINT ( 'NONE',  ( -10.44103466624267185, 32.57396620494226624, 7.500000000000004441 ) ) ;
#28876 = ORIENTED_EDGE ( 'NONE', *, *, #20817, .F. ) ;
#28877 = CARTESIAN_POINT ( 'NONE',  ( 28.23010493019885914, 0.2772093697871412799, -12.55662080966007110 ) ) ;
#28878 = CARTESIAN_POINT ( 'NONE',  ( -6.572794801194226544, 16.58182897866500127, 9.000000000000001776 ) ) ;
#28879 = DIRECTION ( 'NONE',  ( 0.5254827454987608393, 0.4731467892558162691, -0.7071067811865451302 ) ) ;
#28880 = ORIENTED_EDGE ( 'NONE', *, *, #16466, .T. ) ;
#28881 = CARTESIAN_POINT ( 'NONE',  ( -30.36177892311615167, -0.01403434324402295062, -8.297102314141014290 ) ) ;
#28882 = CARTESIAN_POINT ( 'NONE',  ( -39.48531003256149319, -11.24999992065011156, 11.00000000000000000 ) ) ;
#28883 = ORIENTED_EDGE ( 'NONE', *, *, #25970, .F. ) ;
#28884 = CARTESIAN_POINT ( 'NONE',  ( 28.41975474895474818, -1.822096834479148386, -14.26935881984800147 ) ) ;
#28885 = CARTESIAN_POINT ( 'NONE',  ( 13.19262166295606775, 15.69476543507642852, -30.00000000000001066 ) ) ;
#28886 = CARTESIAN_POINT ( 'NONE',  ( 15.48695972777691310, -26.74878859331900927, 16.30093088680190405 ) ) ;
#28887 = ADVANCED_FACE ( 'NONE', ( #23155 ), #10568, .T. ) ;
#28888 = ORIENTED_EDGE ( 'NONE', *, *, #33705, .F. ) ;
#28889 = CARTESIAN_POINT ( 'NONE',  ( -1.412590157703688977E-13, 38.50629078351121137, 16.30093088680190405 ) ) ;
#28890 = ADVANCED_FACE ( 'NONE', ( #25997 ), #13202, .T. ) ;
#28891 = FACE_OUTER_BOUND ( 'NONE', #13134, .T. ) ;
#28892 = AXIS2_PLACEMENT_3D ( 'NONE', #18294, #11793, #37171 ) ;
#28893 = CARTESIAN_POINT ( 'NONE',  ( 4.002244506128361579, 26.73020382270167516, 20.99999999999999645 ) ) ;
#28894 = DIRECTION ( 'NONE',  ( 0.000000000000000000, 0.000000000000000000, -1.000000000000000000 ) ) ;
#28895 = DIRECTION ( 'NONE',  ( 0.000000000000000000, 0.000000000000000000, 1.000000000000000000 ) ) ;
#28896 = CONICAL_SURFACE ( 'NONE', #2286, 1.000000000000004441, 0.7853981633974583820 ) ;
#28897 = VECTOR ( 'NONE', #35045, 1000.000000000000114 ) ;
#28898 = AXIS2_PLACEMENT_3D ( 'NONE', #40057, #36426, #24428 ) ;
#28899 = FACE_BOUND ( 'NONE', #6373, .T. ) ;
#28900 = CARTESIAN_POINT ( 'NONE',  ( 15.26743640727520557, 21.18345451738099428, 17.92354375534863209 ) ) ;
#28901 = CARTESIAN_POINT ( 'NONE',  ( -22.67492542834196101, 9.789819215906979011, -8.893573617071718118 ) ) ;
#28902 = CARTESIAN_POINT ( 'NONE',  ( 15.95756409205271709, -19.85041831507555798, -19.00748645968882045 ) ) ;
#28903 = PLANE ( 'NONE',  #12469 ) ;
#28904 = ADVANCED_FACE ( 'NONE', ( #1027 ), #16876, .F. ) ;
#28905 = CARTESIAN_POINT ( 'NONE',  ( 15.31294454353861667, 26.87829293536686137, -6.413898871446972905 ) ) ;
#28906 = ORIENTED_EDGE ( 'NONE', *, *, #34748, .F. ) ;
#28907 = CARTESIAN_POINT ( 'NONE',  ( -15.68734635201983174, 24.91775635742894579, -7.836637281011617162 ) ) ;
#28908 = CARTESIAN_POINT ( 'NONE',  ( -30.12142568021468136, -17.39061322484690919, 19.27171037444157164 ) ) ;
#28909 = DIRECTION ( 'NONE',  ( -1.000000000000000000, 0.000000000000000000, 0.000000000000000000 ) ) ;
#28910 = CARTESIAN_POINT ( 'NONE',  ( 13.79954197581136732, 23.33194756670403436, -14.47988002075514835 ) ) ;
#28911 = ORIENTED_EDGE ( 'NONE', *, *, #21883, .T. ) ;
#28912 = CARTESIAN_POINT ( 'NONE',  ( 33.35910093694781864, -18.39580519663982727, -7.117606809128307788 ) ) ;
#28913 = DIRECTION ( 'NONE',  ( -0.000000000000000000, -0.000000000000000000, -1.000000000000000000 ) ) ;
#28914 = ORIENTED_EDGE ( 'NONE', *, *, #14335, .F. ) ;
#28916 = FACE_OUTER_BOUND ( 'NONE', #16149, .T. ) ;
#28915 = CARTESIAN_POINT ( 'NONE',  ( -12.45621400986809668, 21.34344825005930346, -18.40940681241713150 ) ) ;
#28917 = CARTESIAN_POINT ( 'NONE',  ( -15.68502289456722210, -26.14630305052633119, -9.204429133117855599 ) ) ;
#28918 = CARTESIAN_POINT ( 'NONE',  ( 8.293999462566144842, 11.53598992149257008, 6.000000000000000000 ) ) ;
#28919 = ORIENTED_EDGE ( 'NONE', *, *, #26517, .F. ) ;
#28920 = CARTESIAN_POINT ( 'NONE',  ( -35.14568626021495845, -14.53237387118475432, -5.000000000000003553 ) ) ;
#28921 = CARTESIAN_POINT ( 'NONE',  ( -13.87797780512911139, -25.88099118681344990, -8.779743625905863880 ) ) ;
#28922 = CARTESIAN_POINT ( 'NONE',  ( -4.984135866956331817, 36.15314577889358105, 10.50000000000000533 ) ) ;
#28923 = CARTESIAN_POINT ( 'NONE',  ( 16.86035064919571980, 22.16869397439054978, -5.950760093676068507 ) ) ;
#28924 = ORIENTED_EDGE ( 'NONE', *, *, #186, .F. ) ;
#28925 = CARTESIAN_POINT ( 'NONE',  ( 21.11582681380412296, 4.515134061867360771, -23.11302823821948849 ) ) ;
#28926 = PLANE ( 'NONE',  #4425 ) ;
#28927 = DIRECTION ( 'NONE',  ( 0.9135454576426048634, 0.4067366430757912710, -6.938893903907218911E-15 ) ) ;
#28928 = ORIENTED_EDGE ( 'NONE', *, *, #23415, .F. ) ;
#28929 = CARTESIAN_POINT ( 'NONE',  ( -26.68538983161234768, 0.004158945161739156619, -15.41724847776275098 ) ) ;
#28930 = CARTESIAN_POINT ( 'NONE',  ( 31.42341880231480644, -0.5937245782808074912, -5.470706975624656465 ) ) ;
#28931 = AXIS2_PLACEMENT_3D ( 'NONE', #37248, #25252, #31347 ) ;
#28932 = AXIS2_PLACEMENT_3D ( 'NONE', #9880, #9090, #22261 ) ;
#28933 = CARTESIAN_POINT ( 'NONE',  ( 29.41993030479209281, -12.15499915640502948, 20.25080042701565475 ) ) ;
#28934 = ORIENTED_EDGE ( 'NONE', *, *, #28099, .F. ) ;
#28935 = EDGE_CURVE ( 'NONE', #15766, #11791, #19503, .T. ) ;
#28936 = CARTESIAN_POINT ( 'NONE',  ( -20.90924525106831666, -8.502318254486386451, -30.00000000000000711 ) ) ;
#28937 = CARTESIAN_POINT ( 'NONE',  ( -13.94482798346716557, 26.50521816028930289, 11.00000000000000000 ) ) ;
#28938 = CARTESIAN_POINT ( 'NONE',  ( 13.63396663385386454, 16.24580510161703728, 7.000000000000000000 ) ) ;
#28939 = DIRECTION ( 'NONE',  ( 0.000000000000000000, 0.000000000000000000, 1.000000000000000000 ) ) ;
#28940 = PLANE ( 'NONE',  #660 ) ;
#28941 = CARTESIAN_POINT ( 'NONE',  ( -14.42035624161473883, 26.65972665747678860, 10.49999999999999822 ) ) ;
#28942 = B_SPLINE_CURVE_WITH_KNOTS ( 'NONE', 3,
 ( #467, #37241, #3508, #21994, #9411, #3112, #3308, #18755 ),
 .UNSPECIFIED., .F., .F.,
 ( 4, 2, 2, 4 ),
 ( 0.000000000000000000, 0.0004488403289517302135, 0.0006732604934275947511, 0.0008976806579034594512 ),
 .UNSPECIFIED. ) ;
#28943 = CARTESIAN_POINT ( 'NONE',  ( -14.57486473880221745, 26.18419839932921533, 10.50000000000000533 ) ) ;
#28944 = ORIENTED_EDGE ( 'NONE', *, *, #39336, .F. ) ;
#28945 = CARTESIAN_POINT ( 'NONE',  ( -6.392125613574828336, 35.62765252371742264, 10.99387789255782799 ) ) ;
#28946 = CARTESIAN_POINT ( 'NONE',  ( -6.994507294956786581, 44.66003774390582493, 9.500000000000000000 ) ) ;
#28947 = CARTESIAN_POINT ( 'NONE',  ( 26.61403125366520683, -23.18509203170473043, -10.21710804142331419 ) ) ;
#28948 = DIRECTION ( 'NONE',  ( 0.000000000000000000, 0.000000000000000000, 1.000000000000000000 ) ) ;
#28949 = PLANE ( 'NONE',  #1515 ) ;
#28950 = EDGE_CURVE ( 'NONE', #31599, #7885, #32102, .T. ) ;
#28951 = CARTESIAN_POINT ( 'NONE',  ( 10.47400997058416650, 17.78520939947398105, -28.04374864806230150 ) ) ;
#28952 = DIRECTION ( 'NONE',  ( -0.9135454576426005335, 0.4067366430758009299, 0.000000000000000000 ) ) ;
#28953 = ORIENTED_EDGE ( 'NONE', *, *, #37807, .T. ) ;
#28955 = VECTOR ( 'NONE', #9641, 1000.000000000000000 ) ;
#28954 = CARTESIAN_POINT ( 'NONE',  ( -14.05926931476738595, 15.33240373186624694, -26.47723576656629163 ) ) ;
#28956 = CARTESIAN_POINT ( 'NONE',  ( -23.31304291943800067, -15.59395685184293967, 21.00000000000000000 ) ) ;
#28957 = EDGE_CURVE ( 'NONE', #39268, #16887, #1426, .T. ) ;
#28958 = AXIS2_PLACEMENT_3D ( 'NONE', #4374, #16780, #23470 ) ;
#28959 = EDGE_CURVE ( 'NONE', #8671, #5684, #7171, .T. ) ;
#28960 = CARTESIAN_POINT ( 'NONE',  ( 13.00677425146152366, -23.09145112541884259, -15.45087358678626366 ) ) ;
#28961 = CARTESIAN_POINT ( 'NONE',  ( 2.525645716490518389, 8.212903943950921715, 9.000000000000001776 ) ) ;
#28962 = CARTESIAN_POINT ( 'NONE',  ( 10.99973294177321215, 17.29901363094238675, -30.00000000000001421 ) ) ;
#28963 = ORIENTED_EDGE ( 'NONE', *, *, #23233, .T. ) ;
#28964 = CARTESIAN_POINT ( 'NONE',  ( 15.36806905513557808, 26.68643454456307396, -6.416988418440872977 ) ) ;
#28965 = VERTEX_POINT ( 'NONE', #11377 ) ;
#28967 = DIRECTION ( 'NONE',  ( 0.000000000000000000, 0.000000000000000000, 1.000000000000000000 ) ) ;
#28966 = CARTESIAN_POINT ( 'NONE',  ( -13.45748191022267193, 22.88503781989287944, -15.44276203698733774 ) ) ;
#28968 = CARTESIAN_POINT ( 'NONE',  ( -15.20090094983863160, -26.38220823943847293, -7.828045879455097555 ) ) ;
#28969 = CARTESIAN_POINT ( 'NONE',  ( -31.25372621196067513, -24.60616950719562723, 12.73282698324853079 ) ) ;
#28970 = EDGE_CURVE ( 'NONE', #37730, #9704, #24156, .T. ) ;
#28971 = CARTESIAN_POINT ( 'NONE',  ( -31.41171746008181032, -20.30212926178818833, -8.407145291683050914 ) ) ;
#28972 = CARTESIAN_POINT ( 'NONE',  ( -1.907480624423063320, -21.18899373848512724, -23.32666558514067390 ) ) ;
#28973 = CARTESIAN_POINT ( 'NONE',  ( 15.62450264098779051, 25.80212576317565265, -6.418156584292412425 ) ) ;
#28974 = EDGE_LOOP ( 'NONE', ( #14636, #12450, #11148, #4189 ) ) ;
#28975 = CARTESIAN_POINT ( 'NONE',  ( 23.08677377554354493, 8.111467817205479491, -11.84555345141176907 ) ) ;
#28976 = LINE ( 'NONE', #38321, #27743 ) ;
#28977 = CARTESIAN_POINT ( 'NONE',  ( -8.858816326124456353, -25.39986765292802318, -4.999999999999999112 ) ) ;
#28978 = CARTESIAN_POINT ( 'NONE',  ( -13.83280510892178938, 26.34487040058245455, 17.92354375535250810 ) ) ;
#28979 = ORIENTED_EDGE ( 'NONE', *, *, #3169, .T. ) ;
#28980 = CARTESIAN_POINT ( 'NONE',  ( -32.87372159360177193, -3.395346227908654591, -8.163538743417984023 ) ) ;
#28981 = DIRECTION ( 'NONE',  ( 0.3090169943749560000, 0.9510565162951507556, 0.000000000000000000 ) ) ;
#28982 = ORIENTED_EDGE ( 'NONE', *, *, #12986, .T. ) ;
#28983 = LINE ( 'NONE', #9899, #38090 ) ;
#28984 = FACE_OUTER_BOUND ( 'NONE', #9260, .T. ) ;
#28985 = EDGE_CURVE ( 'NONE', #31336, #22260, #8521, .T. ) ;
#28986 = ADVANCED_FACE ( 'NONE', ( #15014 ), #15626, .T. ) ;
#28987 = CARTESIAN_POINT ( 'NONE',  ( 19.85478904061002581, -8.024875900502717485, -25.62134553024078087 ) ) ;
#28988 = EDGE_CURVE ( 'NONE', #30940, #3918, #27943, .T. ) ;
#28989 = CARTESIAN_POINT ( 'NONE',  ( 32.84658669524299768, -23.46788009898371996, 11.55979286843938958 ) ) ;
#28990 = AXIS2_PLACEMENT_3D ( 'NONE', #16844, #32070, #10740 ) ;
#28991 = ORIENTED_EDGE ( 'NONE', *, *, #16962, .F. ) ;
#28992 = ORIENTED_EDGE ( 'NONE', *, *, #8046, .F. ) ;
#28993 = DIRECTION ( 'NONE',  ( 0.000000000000000000, 0.000000000000000000, 1.000000000000000000 ) ) ;
#28994 = CARTESIAN_POINT ( 'NONE',  ( 9.917734535019443243, 14.47043272369397116, 13.00000000000000178 ) ) ;
#28995 = CYLINDRICAL_SURFACE ( 'NONE', #14264, 1.000000000000000000 ) ;
#28996 = EDGE_LOOP ( 'NONE', ( #17057, #972, #3343, #34610 ) ) ;
#28997 = CARTESIAN_POINT ( 'NONE',  ( -1.032345509077061241, 20.89205812428711795, -26.96911111641401604 ) ) ;
#28998 = DIRECTION ( 'NONE',  ( 1.000000000000000000, 0.000000000000000000, 0.000000000000000000 ) ) ;
#28999 = FACE_OUTER_BOUND ( 'NONE', #25966, .T. ) ;
#29000 = DIRECTION ( 'NONE',  ( 0.000000000000000000, 0.000000000000000000, 1.000000000000000000 ) ) ;
#29001 = CARTESIAN_POINT ( 'NONE',  ( 15.26584437371809955, 27.13525491562438319, 6.000000000000000000 ) ) ;
#29002 = EDGE_CURVE ( 'NONE', #1935, #7593, #16290, .T. ) ;
#29003 = CARTESIAN_POINT ( 'NONE',  ( 9.221287281574507944, 10.65863771052197784, 10.49999999999999822 ) ) ;
#29004 = CARTESIAN_POINT ( 'NONE',  ( 13.83290884757558104, 28.83794920898534642, -9.108879102860099053 ) ) ;
#29005 = EDGE_CURVE ( 'NONE', #36981, #10090, #18076, .T. ) ;
#29006 = DIRECTION ( 'NONE',  ( -2.168404344971006896E-16, 1.000000000000000000, 0.000000000000000000 ) ) ;
#29007 = ORIENTED_EDGE ( 'NONE', *, *, #36853, .T. ) ;
#29009 = CARTESIAN_POINT ( 'NONE',  ( 4.984135866956515670, 36.15314577889351000, 11.00000000000000000 ) ) ;
#29008 = CARTESIAN_POINT ( 'NONE',  ( -19.65695430485491357, 15.61437265943404995, -6.449524717961147680 ) ) ;
#29010 = DIRECTION ( 'NONE',  ( -0.7431448254773953543, -0.6691306063588570163, -0.000000000000000000 ) ) ;
#29011 = EDGE_CURVE ( 'NONE', #14195, #10996, #20728, .T. ) ;
#29012 = CARTESIAN_POINT ( 'NONE',  ( 9.569772169525011307, -18.12929409070867948, -30.00000000000000000 ) ) ;
#29013 = FACE_OUTER_BOUND ( 'NONE', #15289, .T. ) ;
#29014 = CARTESIAN_POINT ( 'NONE',  ( 12.10580092867515845, 19.95408366012758350, -20.53583464531860159 ) ) ;
#29015 = CARTESIAN_POINT ( 'NONE',  ( -23.06249103411543544, 13.31513540672989926, -13.39439507595155554 ) ) ;
#29016 = CARTESIAN_POINT ( 'NONE',  ( 19.48557158514988075, -11.24999999999998224, 6.000000000000000000 ) ) ;
#29017 = CIRCLE ( 'NONE', #28374, 0.5000000000000011102 ) ;
#29018 = CIRCLE ( 'NONE', #29658, 1.000000000000007772 ) ;
#29019 = ADVANCED_FACE ( 'NONE', ( #33522 ), #8520, .T. ) ;
#29020 = CARTESIAN_POINT ( 'NONE',  ( -15.37464264532748004, -13.57371270378507866, -30.00000000000001421 ) ) ;
#29021 = CARTESIAN_POINT ( 'NONE',  ( 6.428110747044506468, -21.25176611192976495, -20.99117257299570838 ) ) ;
#29022 = CARTESIAN_POINT ( 'NONE',  ( 14.83059429241407123, 25.12647099005219786, -10.65921042686171560 ) ) ;
#29023 = CARTESIAN_POINT ( 'NONE',  ( 18.24293951000086977, 12.18618061105114592, -20.11237983827145115 ) ) ;
#29024 = DIRECTION ( 'NONE',  ( 0.8386705679454296014, 0.5446390350150185355, -9.740544695154170490E-16 ) ) ;
#29025 = CARTESIAN_POINT ( 'NONE',  ( -24.28032989564857047, -12.76774640304084585, 21.00000000000000000 ) ) ;
#29026 = VERTEX_POINT ( 'NONE', #23759 ) ;
#29027 = CARTESIAN_POINT ( 'NONE',  ( -9.370244153187160308, 35.41390855819400940, -5.875078464094462660 ) ) ;
#29028 = ORIENTED_EDGE ( 'NONE', *, *, #7146, .F. ) ;
#29029 = VECTOR ( 'NONE', #32206, 999.9999999999998863 ) ;
#29030 = CARTESIAN_POINT ( 'NONE',  ( 14.70981814587860903, 21.45668995266196433, 10.94387467463493557 ) ) ;
#29031 = ORIENTED_EDGE ( 'NONE', *, *, #39241, .F. ) ;
#29032 = CARTESIAN_POINT ( 'NONE',  ( 30.76077710142195798, -0.06682749899988031650, -6.886782333292955194 ) ) ;
#29033 = CARTESIAN_POINT ( 'NONE',  ( 8.412270287199559604, 10.07085245822950981, 11.00000000000000000 ) ) ;
#29034 = CARTESIAN_POINT ( 'NONE',  ( -31.51573171626090186, 0.5582143012903737489, 15.13084544680213739 ) ) ;
#29035 = ORIENTED_EDGE ( 'NONE', *, *, #33018, .T. ) ;
#29036 = CARTESIAN_POINT ( 'NONE',  ( -30.24738832504583641, 0.1073154935118994652, -8.298770971096649518 ) ) ;
#29037 = ORIENTED_EDGE ( 'NONE', *, *, #12511, .T. ) ;
#29038 = CARTESIAN_POINT ( 'NONE',  ( 21.21202041312366049, -5.034384574639595655, -24.45694360859277694 ) ) ;
#29039 = ADVANCED_FACE ( 'NONE', ( #17482 ), #8924, .F. ) ;
#29040 = VERTEX_POINT ( 'NONE', #26605 ) ;
#29041 = CARTESIAN_POINT ( 'NONE',  ( 12.44178368932912093, 35.65276919561900826, 10.99999999999994316 ) ) ;
#29042 = CARTESIAN_POINT ( 'NONE',  ( -6.151085731882353969, 35.08626808545859888, 7.000000000000000000 ) ) ;
#29043 = CARTESIAN_POINT ( 'NONE',  ( -4.059628295990764357, 8.059656032623825794, 7.338691926023208190 ) ) ;
#29044 = CARTESIAN_POINT ( 'NONE',  ( 1.329271672591037179, 34.78122644969443655, 19.27171037444156454 ) ) ;
#29045 = CIRCLE ( 'NONE', #27103, 1.000000000000000888 ) ;
#29046 = FACE_OUTER_BOUND ( 'NONE', #31078, .T. ) ;
#29047 = VERTEX_POINT ( 'NONE', #33321 ) ;
#29048 = FILL_AREA_STYLE ('',( #32306 ) ) ;
#29049 = CARTESIAN_POINT ( 'NONE',  ( 12.80736835487433289, 15.68301270189216545, 11.00000000000000000 ) ) ;
#29050 = DIRECTION ( 'NONE',  ( 0.000000000000000000, 0.000000000000000000, 1.000000000000000000 ) ) ;
#29051 = CIRCLE ( 'NONE', #11551, 15.00000000000000000 ) ;
#29052 = CARTESIAN_POINT ( 'NONE',  ( -18.69515074622357176, 22.45407711376243753, 11.00000000002426148 ) ) ;
#29053 = CARTESIAN_POINT ( 'NONE',  ( 13.86124000734726103, 15.40656454556149590, -27.04395577147614915 ) ) ;
#29054 = AXIS2_PLACEMENT_3D ( 'NONE', #20146, #31379, #23390 ) ;
#29055 = CARTESIAN_POINT ( 'NONE',  ( 11.44944937545603203, 32.55932223515596036, -8.531584680290370315 ) ) ;
#29056 = ORIENTED_EDGE ( 'NONE', *, *, #27545, .T. ) ;
#29057 = CARTESIAN_POINT ( 'NONE',  ( 6.143904198944456496, -13.77689918168226058, 20.99999999999998934 ) ) ;
#29058 = CARTESIAN_POINT ( 'NONE',  ( -1.000000000000000222, 37.13089969389957901, 10.49999999999999645 ) ) ;
#29059 = EDGE_CURVE ( 'NONE', #25190, #14259, #16546, .T. ) ;
#29060 = CARTESIAN_POINT ( 'NONE',  ( 15.31709984922062517, -25.22568667072951598, -11.53260946786015317 ) ) ;
#29061 = PLANE ( 'NONE',  #35303 ) ;
#29062 = CARTESIAN_POINT ( 'NONE',  ( -14.36830325120616081, 20.48707633493503977, 11.00000000000000000 ) ) ;
#29063 = VERTEX_POINT ( 'NONE', #2037 ) ;
#29064 = CARTESIAN_POINT ( 'NONE',  ( -11.00242421671864790, 17.29730523913238827, -29.34874318703804263 ) ) ;
#29065 = CARTESIAN_POINT ( 'NONE',  ( -22.45592429723070893, -27.55223906713353088, 15.72805884748896688 ) ) ;
#29066 = CARTESIAN_POINT ( 'NONE',  ( 14.30475062438041256, -25.71389175379151837, -9.717608377535148279 ) ) ;
#29067 = DIRECTION ( 'NONE',  ( -2.168404344971006896E-16, 1.000000000000000000, 0.000000000000000000 ) ) ;
#29068 = VERTEX_POINT ( 'NONE', #14820 ) ;
#29069 = VERTEX_POINT ( 'NONE', #26807 ) ;
#29070 = CARTESIAN_POINT ( 'NONE',  ( -12.74940050238178735, 29.92346444574509334, -9.954757084635510012 ) ) ;
#29071 = FACE_OUTER_BOUND ( 'NONE', #16953, .T. ) ;
#29072 = FACE_BOUND ( 'NONE', #16698, .T. ) ;
#29073 = AXIS2_PLACEMENT_3D ( 'NONE', #34090, #34290, #14999 ) ;
#29074 = AXIS2_PLACEMENT_3D ( 'NONE', #29933, #1916, #33404 ) ;
#29075 = CARTESIAN_POINT ( 'NONE',  ( -20.45380339070934284, -5.041909576501859114, -26.41892961284724350 ) ) ;
#29076 = CARTESIAN_POINT ( 'NONE',  ( -13.36146265112639675, 15.68301270189280672, 7.445905703748357141 ) ) ;
#29077 = ORIENTED_EDGE ( 'NONE', *, *, #27736, .F. ) ;
#29078 = CARTESIAN_POINT ( 'NONE',  ( 30.75747790117273794, 0.1077116562829361079, -5.474152632779671457 ) ) ;
#29079 = FACE_OUTER_BOUND ( 'NONE', #21253, .T. ) ;
#29080 = CARTESIAN_POINT ( 'NONE',  ( 13.53057405073934838, 22.08338764125490528, 9.500000000000000000 ) ) ;
#29081 = VECTOR ( 'NONE', #8007, 1000.000000000000000 ) ;
#29082 = ORIENTED_EDGE ( 'NONE', *, *, #5365, .T. ) ;
#29083 = CARTESIAN_POINT ( 'NONE',  ( -20.96976484853918876, 0.8063829224527387929, -26.22476293720499285 ) ) ;
#29084 = CARTESIAN_POINT ( 'NONE',  ( -5.002948306803596701, 36.19539921059739385, 10.49999999999999822 ) ) ;
#29085 = ORIENTED_EDGE ( 'NONE', *, *, #16640, .F. ) ;
#29086 = CARTESIAN_POINT ( 'NONE',  ( 20.45006009983584860, -1.583034825077791696, -30.00000000000000000 ) ) ;
#29087 = VECTOR ( 'NONE', #38174, 999.9999999999998863 ) ;
#29088 = CARTESIAN_POINT ( 'NONE',  ( 20.47044054185530726, -1.308743071981321560, -29.99999999999996803 ) ) ;
#29089 = CARTESIAN_POINT ( 'NONE',  ( 34.90004137879596868, -9.293601764822927436, 16.87380292611441845 ) ) ;
#29090 = EDGE_CURVE ( 'NONE', #23552, #28064, #27011, .T. ) ;
#29091 = VERTEX_POINT ( 'NONE', #14622 ) ;
#29092 = CARTESIAN_POINT ( 'NONE',  ( 8.548670570950529068, 36.69528512485702976, 15.72805884748941807 ) ) ;
#29093 = ADVANCED_FACE ( 'NONE', ( #15218 ), #31229, .T. ) ;
#29094 = CARTESIAN_POINT ( 'NONE',  ( -5.178899460637612862, -25.25135431486990711, 15.72805884748939853 ) ) ;
#29095 = CARTESIAN_POINT ( 'NONE',  ( -0.9999999999999997780, 36.00000000000000711, 9.500000000000000000 ) ) ;
#29096 = CARTESIAN_POINT ( 'NONE',  ( -4.817371740575544514, 23.83900317890010001, 20.99999999999999645 ) ) ;
#29097 = DIRECTION ( 'NONE',  ( 1.000000000000000000, 0.000000000000000000, 0.000000000000000000 ) ) ;
#29098 = CARTESIAN_POINT ( 'NONE',  ( 2.806807826039672715, 9.295007390093600108, 7.000000000000000000 ) ) ;
#29099 = EDGE_CURVE ( 'NONE', #20131, #33341, #18471, .T. ) ;
#29100 = AXIS2_PLACEMENT_3D ( 'NONE', #33802, #23300, #13744 ) ;
#29101 = CIRCLE ( 'NONE', #5096, 1.000000000000000888 ) ;
#29102 = CARTESIAN_POINT ( 'NONE',  ( 25.71436706254310067, 9.015208126564360214, -5.000000000000000888 ) ) ;
#29103 = CARTESIAN_POINT ( 'NONE',  ( 13.22866120778439125, 26.17694675931205595, 18.42518152272108978 ) ) ;
#29104 = CARTESIAN_POINT ( 'NONE',  ( -19.24333380943624050, 7.104126583969421205, -30.00000000000000000 ) ) ;
#29105 = CARTESIAN_POINT ( 'NONE',  ( 14.07081834845426016, -16.54739306722566283, -24.54471350758723602 ) ) ;
#29106 = CIRCLE ( 'NONE', #8989, 0.5000000000000004441 ) ;
#29107 = DIRECTION ( 'NONE',  ( -0.2079116908177663647, -0.9781476007338042455, -3.469446951953611033E-15 ) ) ;
#29108 = EDGE_LOOP ( 'NONE', ( #11665, #30533, #10436 ) ) ;
#29109 = CARTESIAN_POINT ( 'NONE',  ( 15.11738838694767217, 26.47243151418015827, -8.290468601944230187 ) ) ;
#29110 = EDGE_LOOP ( 'NONE', ( #32072, #3942, #35942, #36073 ) ) ;
#29111 = CARTESIAN_POINT ( 'NONE',  ( -15.56517687278530282, 24.67863418428501632, -8.782714596946386010 ) ) ;
#29112 = CARTESIAN_POINT ( 'NONE',  ( -27.96047413129358006, -4.559793092419412552, 19.99202127657104455 ) ) ;
#29113 = EDGE_CURVE ( 'NONE', #13649, #11592, #6266, .T. ) ;
#29114 = CARTESIAN_POINT ( 'NONE',  ( 10.58109189495872116, 32.70007430011108340, 10.96580508970282963 ) ) ;
#29115 = CARTESIAN_POINT ( 'NONE',  ( 11.17396215358744271, 17.57883549974418713, -26.83496991786927666 ) ) ;
#29116 = ORIENTED_EDGE ( 'NONE', *, *, #23922, .T. ) ;
#29117 = CARTESIAN_POINT ( 'NONE',  ( 25.46527745054863345, -14.04222176945395439, -16.62674829446373792 ) ) ;
#29118 = CARTESIAN_POINT ( 'NONE',  ( 3.229431105722923245, 20.49260818092372460, 12.00000000000000000 ) ) ;
#29119 = ORIENTED_EDGE ( 'NONE', *, *, #12986, .F. ) ;
#29121 = CARTESIAN_POINT ( 'NONE',  ( 8.249810963174727618, 9.972158775796183150, 7.485699520496982728 ) ) ;
#29120 = CARTESIAN_POINT ( 'NONE',  ( -10.86820090079098122, 17.78895852278078848, -26.80626250025666835 ) ) ;
#29122 = CARTESIAN_POINT ( 'NONE',  ( -16.05336419634168266, -26.67939413728697318, -7.338295715723472057 ) ) ;
#29123 = CARTESIAN_POINT ( 'NONE',  ( -9.356056665764020508, 26.06569820189716324, 10.50000000000000533 ) ) ;
#29124 = EDGE_LOOP ( 'NONE', ( #33069, #37909, #36393, #26593, #20438, #38124, #5404 ) ) ;
#29125 = CARTESIAN_POINT ( 'NONE',  ( -20.30067844349249029, -8.412790941247147103, -24.26813493527708232 ) ) ;
#29126 = CARTESIAN_POINT ( 'NONE',  ( -14.83609535436326254, -26.57805634534657102, -5.474075349637312016 ) ) ;
#29127 = PLANE ( 'NONE',  #6647 ) ;
#29128 = CARTESIAN_POINT ( 'NONE',  ( 15.75967858163252977, 18.63110151714538887, -15.73365853743660736 ) ) ;
#29129 = ORIENTED_EDGE ( 'NONE', *, *, #39045, .T. ) ;
#29130 = CARTESIAN_POINT ( 'NONE',  ( 23.44710309751157951, 3.753209576940052639, -17.73587880687377805 ) ) ;
#29131 = CARTESIAN_POINT ( 'NONE',  ( -1.000003370709253492, 22.50000000000031264, 12.00000000000000000 ) ) ;
#29132 = CARTESIAN_POINT ( 'NONE',  ( -18.23649648353780961, -16.09146789626144169, 23.00000000000000000 ) ) ;
#29133 = EDGE_LOOP ( 'NONE', ( #5261, #1788, #25875 ) ) ;
#29134 = CARTESIAN_POINT ( 'NONE',  ( -23.41064877084379248, 0.2929791562720443499, -20.50634540125940219 ) ) ;
#29136 = CARTESIAN_POINT ( 'NONE',  ( 20.53937652207208231, 0.5506371726960779256, -28.69615207527581191 ) ) ;
#29135 = AXIS2_PLACEMENT_3D ( 'NONE', #27459, #29911, #33775 ) ;
#29137 = AXIS2_PLACEMENT_3D ( 'NONE', #15373, #15769, #27960 ) ;
#29138 = CARTESIAN_POINT ( 'NONE',  ( 22.33353841799053541, -20.81031336111236740, 20.25080042701592475 ) ) ;
#29139 = ADVANCED_FACE ( 'NONE', ( #21901 ), #33819, .T. ) ;
#29140 = VERTEX_POINT ( 'NONE', #37151 ) ;
#29141 = AXIS2_PLACEMENT_3D ( 'NONE', #13247, #19961, #28690 ) ;
#29142 =( BOUNDED_SURFACE ( )  B_SPLINE_SURFACE ( 2, 3, ( 
 ( #9114, #18856, #37143, #373, #27798, #30854 ),
 ( #31445, #9317, #12752, #18661, #31053, #22291 ),
 ( #6059, #9718, #3218, #22098, #6844, #6646 ) ),
 .UNSPECIFIED., .F., .F., .F. ) 
 B_SPLINE_SURFACE_WITH_KNOTS ( ( 3, 3 ),
 ( 4, 2, 4 ),
 ( 0.000000000000000000, 1.000000000000000000 ),
 ( 3.412702215524944904, 3.665191429188091377, 3.917680642851237405 ),
 .UNSPECIFIED. ) 
 GEOMETRIC_REPRESENTATION_ITEM ( )  RATIONAL_B_SPLINE_SURFACE ( (
 ( 1.000000000000000000, 1.000000000000000000, 1.000000000000000000, 1.000000000000000000, 1.000000000000000000, 1.000000000000000000),
 ( 0.7071067811865474617, 0.7071067811865474617, 0.7071067811865474617, 0.7071067811865474617, 0.7071067811865474617, 0.7071067811865474617),
 ( 1.000000000000000000, 1.000000000000000000, 1.000000000000000000, 1.000000000000000000, 1.000000000000000000, 1.000000000000000000) ) ) 
 REPRESENTATION_ITEM ( '' )  SURFACE ( )  );
#29143 = PRODUCT_RELATED_PRODUCT_CATEGORY ( 'part', '', ( #3190 ) ) ;
#29144 = CARTESIAN_POINT ( 'NONE',  ( -22.52744239175981278, -0.1803094636421871677, -20.90349153980994501 ) ) ;
#29145 = CYLINDRICAL_SURFACE ( 'NONE', #38774, 1.000000000000000888 ) ;
#29146 = PLANE ( 'NONE',  #19356 ) ;
#29147 = EDGE_CURVE ( 'NONE', #39240, #4057, #65, .T. ) ;
#29148 = EDGE_CURVE ( 'NONE', #18344, #11394, #577, .T. ) ;
#29149 = DIRECTION ( 'NONE',  ( 0.000000000000000000, 0.000000000000000000, 1.000000000000000000 ) ) ;
#29150 = CARTESIAN_POINT ( 'NONE',  ( -11.48173768534023331, 32.16538668264431777, 10.49999999999999822 ) ) ;
#29151 = LINE ( 'NONE', #19198, #3457 ) ;
#29152 = DIRECTION ( 'NONE',  ( 0.000000000000000000, 0.000000000000000000, -1.000000000000000000 ) ) ;
#29153 = ORIENTED_EDGE ( 'NONE', *, *, #39173, .T. ) ;
#29154 = DIRECTION ( 'NONE',  ( 0.000000000000000000, 0.000000000000000000, 1.000000000000000000 ) ) ;
#29155 = PLANE ( 'NONE',  #22023 ) ;
#29156 = CARTESIAN_POINT ( 'NONE',  ( 23.14904545314587025, -21.42671327224799427, -13.89312732397599426 ) ) ;
#29157 = DIRECTION ( 'NONE',  ( -1.000000000000000000, 0.000000000000000000, 0.000000000000000000 ) ) ;
#29158 = CARTESIAN_POINT ( 'NONE',  ( -7.096882951594429834, 29.56287847632736288, 10.49999999999999645 ) ) ;
#29159 = CARTESIAN_POINT ( 'NONE',  ( 12.05224603734456679, 20.93102218528974134, -19.42687687656769668 ) ) ;
#29160 = CARTESIAN_POINT ( 'NONE',  ( 0.4999999999999995559, 37.00000000000000711, 11.00000000000000000 ) ) ;
#29161 = AXIS2_PLACEMENT_3D ( 'NONE', #32819, #22847, #32618 ) ;
#29162 = ORIENTED_EDGE ( 'NONE', *, *, #30308, .T. ) ;
#29163 = CARTESIAN_POINT ( 'NONE',  ( -15.03102915852888444, 16.97105545825134953, -19.88194163820099192 ) ) ;
#29164 = CARTESIAN_POINT ( 'NONE',  ( -23.98526753813956347, -9.069922861307588846, 20.99999999999999645 ) ) ;
#29165 = EDGE_CURVE ( 'NONE', #11380, #25337, #13700, .T. ) ;
#29166 = CARTESIAN_POINT ( 'NONE',  ( 11.82685544034319314, -21.49105343387592626, -18.46001624164255261 ) ) ;
#29167 = EDGE_CURVE ( 'NONE', #11008, #5904, #21706, .T. ) ;
#29168 = DIRECTION ( 'NONE',  ( 1.000000000000000000, 0.000000000000000000, 0.000000000000000000 ) ) ;
#29169 = CARTESIAN_POINT ( 'NONE',  ( 15.29903755497086415, 26.49996819934222358, -7.357928002827080149 ) ) ;
#29170 = ORIENTED_EDGE ( 'NONE', *, *, #23510, .T. ) ;
#29171 = CARTESIAN_POINT ( 'NONE',  ( 11.47567478000847885, 18.44475041446002450, -23.85263498135895688 ) ) ;
#29172 = AXIS2_PLACEMENT_3D ( 'NONE', #26802, #20315, #5465 ) ;
#29173 = B_SPLINE_SURFACE_WITH_KNOTS ( 'NONE', 1, 3, ( 
 ( #31964, #690, #16331, #13067, #38060, #9644, #22411, #22022, #4130, #31368 ),
 ( #37267, #9441, #28314, #34813, #6966, #21820, #19371, #34225, #7582, #5145 ) ),
 .UNSPECIFIED., .F., .F., .F.,
 ( 2, 2 ),
 ( 4, 2, 2, 2, 4 ),
 ( 0.000000000000000000, 1.000000000000000000 ),
 ( 1.958393013450087983, 2.351092095148810568, 2.743791176847532931, 3.136490258546255738, 3.529189340244978101 ),
 .UNSPECIFIED. ) ;
#29174 = EDGE_LOOP ( 'NONE', ( #1422, #36681 ) ) ;
#29176 = CARTESIAN_POINT ( 'NONE',  ( -13.94482798346716201, 26.50521816028930999, 7.499999999999993783 ) ) ;
#29175 = CARTESIAN_POINT ( 'NONE',  ( -15.14009367329834888, 26.39762901518510319, -8.293352721384346538 ) ) ;
#29177 = CARTESIAN_POINT ( 'NONE',  ( -11.53523938750379685, -20.97785456172497831, -19.49820750867069918 ) ) ;
#29178 = CARTESIAN_POINT ( 'NONE',  ( -37.45384686740443669, -12.88771083438535214, 12.14047268033070992 ) ) ;
#29179 = CARTESIAN_POINT ( 'NONE',  ( -32.30830845181216660, -19.51484095444094535, -7.971085280149651453 ) ) ;
#29180 = CARTESIAN_POINT ( 'NONE',  ( -1.806066488169840056, -20.67681132108909381, -26.61857900440850599 ) ) ;
#29181 = CARTESIAN_POINT ( 'NONE',  ( 15.61778544462205431, 24.86146771946813061, -8.309072973913199434 ) ) ;
#29182 = EDGE_LOOP ( 'NONE', ( #6223, #5267, #28992, #17203 ) ) ;
#29183 = CARTESIAN_POINT ( 'NONE',  ( 23.00570941814261161, 9.122255987794249066, -9.381850414016666306 ) ) ;
#29184 = DIRECTION ( 'NONE',  ( -0.000000000000000000, -0.000000000000000000, 1.000000000000000000 ) ) ;
#29185 = CARTESIAN_POINT ( 'NONE',  ( -12.23327497914565853, 13.81973598992469121, 7.000000000000000000 ) ) ;
#29186 = CARTESIAN_POINT ( 'NONE',  ( 11.91494638969559361, 32.61409561180352057, 16.87380292611443977 ) ) ;
#29187 = ORIENTED_EDGE ( 'NONE', *, *, #23154, .T. ) ;
#29188 = CARTESIAN_POINT ( 'NONE',  ( -32.32461280127759551, -2.467648900451871796, -8.192925622072531056 ) ) ;
#29189 = CARTESIAN_POINT ( 'NONE',  ( -22.54917513128955164, -0.2132175735129904770, 20.25080042701864969 ) ) ;
#29190 = EDGE_LOOP ( 'NONE', ( #8712, #16657, #23245, #7977, #3133 ) ) ;
#29191 = CARTESIAN_POINT ( 'NONE',  ( 8.137585970692075676, 29.15429895402930072, 10.50000000000000000 ) ) ;
#29192 = DIRECTION ( 'NONE',  ( 1.000000000000000000, 0.000000000000000000, 0.000000000000000000 ) ) ;
#29193 = EDGE_CURVE ( 'NONE', #3260, #34846, #37351, .T. ) ;
#29194 = CARTESIAN_POINT ( 'NONE',  ( 18.76590878806661067, -8.252041909800054142, -29.21828954202150541 ) ) ;
#29195 = CARTESIAN_POINT ( 'NONE',  ( 34.90171719354076885, -20.15051581687074034, 12.73282698324853257 ) ) ;
#29196 = VECTOR ( 'NONE', #7111, 1000.000000000000000 ) ;
#29197 = ORIENTED_EDGE ( 'NONE', *, *, #17845, .T. ) ;
#29198 = CIRCLE ( 'NONE', #12317, 0.5000000000000004441 ) ;
#29199 = FACE_OUTER_BOUND ( 'NONE', #32461, .T. ) ;
#29200 = CARTESIAN_POINT ( 'NONE',  ( -17.09304275257433048, 21.59026560281640883, -4.999999999999997335 ) ) ;
#29201 = DIRECTION ( 'NONE',  ( 0.000000000000000000, 0.000000000000000000, 1.000000000000000000 ) ) ;
#29202 = VERTEX_POINT ( 'NONE', #16014 ) ;
#29203 = CARTESIAN_POINT ( 'NONE',  ( -1.015836423920226883, 20.57100803839839998, -28.44595161374707004 ) ) ;
#29204 = DIRECTION ( 'NONE',  ( 1.000000000000000000, 0.000000000000000000, 0.000000000000000000 ) ) ;
#29205 = CARTESIAN_POINT ( 'NONE',  ( -13.63581098909220479, 27.45627467658446008, 7.000000000000000000 ) ) ;
#29206 = DIRECTION ( 'NONE',  ( -0.000000000000000000, -0.000000000000000000, -1.000000000000000000 ) ) ;
#29207 = CARTESIAN_POINT ( 'NONE',  ( -14.50767453556301589, 21.81310552875940090, 10.66666666666666252 ) ) ;
#29208 = LINE ( 'NONE', #38347, #39162 ) ;
#29209 = CARTESIAN_POINT ( 'NONE',  ( 12.17552494184827339, 25.04416116006207460, -15.21251802476954396 ) ) ;
#29210 = DIRECTION ( 'NONE',  ( -1.000000000000000000, 0.000000000000000000, 0.000000000000000000 ) ) ;
#29211 = VERTEX_POINT ( 'NONE', #18865 ) ;
#29212 = AXIS2_PLACEMENT_3D ( 'NONE', #1623, #7710, #4054 ) ;
#29214 = DIRECTION ( 'NONE',  ( 0.000000000000000000, 0.000000000000000000, 1.000000000000000000 ) ) ;
#29213 = CARTESIAN_POINT ( 'NONE',  ( -19.90936391447298703, 14.41308808657887042, -9.387851554354570638 ) ) ;
#29215 = CARTESIAN_POINT ( 'NONE',  ( -14.08493436138092036, 27.60220370627969899, 10.68306085400105765 ) ) ;
#29216 = CARTESIAN_POINT ( 'NONE',  ( 15.39191398672864430, -26.52213166449434922, -7.356080702479480316 ) ) ;
#29217 = CARTESIAN_POINT ( 'NONE',  ( -75.15099915297791711, 43.38844959084113384, 3.000000000000000000 ) ) ;
#29218 = CARTESIAN_POINT ( 'NONE',  ( 13.74447603680569330, 23.45254812458578897, -14.47033917909823053 ) ) ;
#29219 = CARTESIAN_POINT ( 'NONE',  ( -6.023418944065157987, 39.81932404830322270, -4.999999999999988454 ) ) ;
#29220 = CARTESIAN_POINT ( 'NONE',  ( -8.505700342264141511, 22.10876900990917804, 7.000000000000000000 ) ) ;
#29221 = EDGE_CURVE ( 'NONE', #7567, #4300, #9919, .T. ) ;
#29222 = CARTESIAN_POINT ( 'NONE',  ( -20.65774335103317227, -19.41944233773801898, -16.75787539182721275 ) ) ;
#29223 = CARTESIAN_POINT ( 'NONE',  ( 5.978239409463006027, -20.40449185056595027, -24.25458186627032120 ) ) ;
#29224 = CARTESIAN_POINT ( 'NONE',  ( 15.23844353641876381, 26.06950005415061966, -8.299311558484985696 ) ) ;
#29225 = CARTESIAN_POINT ( 'NONE',  ( 21.09554553119179587, 13.00325820389446640, -4.999999999999996447 ) ) ;
#29226 = CARTESIAN_POINT ( 'NONE',  ( -8.744117900323425729, 12.16605582823075338, 10.00000000000000000 ) ) ;
#29227 = CARTESIAN_POINT ( 'NONE',  ( -24.37759566069507855, -10.08322588119030172, 20.99999999999999645 ) ) ;
#29228 = ORIENTED_EDGE ( 'NONE', *, *, #27501, .T. ) ;
#29229 = CARTESIAN_POINT ( 'NONE',  ( -8.892437800321363994, 33.34416954038874792, -10.26036216454556538 ) ) ;
#29230 = EDGE_LOOP ( 'NONE', ( #3213, #13096, #5727, #29680 ) ) ;
#29231 = CARTESIAN_POINT ( 'NONE',  ( -9.590349012255924066, -18.48796701930649178, -26.83885042670429755 ) ) ;
#29232 = CARTESIAN_POINT ( 'NONE',  ( 14.75621568350166335, 21.89813303538585032, 10.49999999999999822 ) ) ;
#29233 = ORIENTED_EDGE ( 'NONE', *, *, #30488, .F. ) ;
#29234 = CARTESIAN_POINT ( 'NONE',  ( 20.48156205581511458, 0.8692611811187744841, -30.00000000000000000 ) ) ;
#29235 = DIRECTION ( 'NONE',  ( 1.000000000000000000, 0.000000000000000000, 0.000000000000000000 ) ) ;
#29236 = CARTESIAN_POINT ( 'NONE',  ( -28.78471548568729688, -2.122417091760708807, 18.87996532025785257 ) ) ;
#29237 = ORIENTED_EDGE ( 'NONE', *, *, #33173, .F. ) ;
#29238 = CARTESIAN_POINT ( 'NONE',  ( -27.66913085872133493, 0.2817421747210221428, -13.51868300798002309 ) ) ;
#29239 = EDGE_CURVE ( 'NONE', #25837, #31884, #24098, .T. ) ;
#29240 = ORIENTED_EDGE ( 'NONE', *, *, #25395, .T. ) ;
#29241 = B_SPLINE_CURVE_WITH_KNOTS ( 'NONE', 3,
 ( #21104, #20906, #11760, #23353, #23750, #11366, #35750, #1823 ),
 .UNSPECIFIED., .F., .F.,
 ( 4, 2, 2, 4 ),
 ( 8.673617379884035472E-19, 0.0004726692273637059846, 0.0007090038410455666747, 0.0009453384547274274732 ),
 .UNSPECIFIED. ) ;
#29242 = CARTESIAN_POINT ( 'NONE',  ( 35.39442739984237818, -9.583334781271833691, -5.874798423248003942 ) ) ;
#29243 = ADVANCED_FACE ( 'NONE', ( #22298 ), #21508, .F. ) ;
#29244 = CIRCLE ( 'NONE', #4599, 0.5000000000000004441 ) ;
#29245 = EDGE_LOOP ( 'NONE', ( #22981, #18436 ) ) ;
#29246 = CARTESIAN_POINT ( 'NONE',  ( -1.947644445291446980, 40.50000000000003553, 11.55979286843934695 ) ) ;
#29247 = CARTESIAN_POINT ( 'NONE',  ( -10.14717575287011542, 32.53695909538323860, 13.00000000000000178 ) ) ;
#29248 = DIRECTION ( 'NONE',  ( 1.000000000000000000, 0.000000000000000000, 0.000000000000000000 ) ) ;
#29249 = CARTESIAN_POINT ( 'NONE',  ( -11.57512167954172355, 28.64755075779800464, 18.87996532025787388 ) ) ;
#29250 = ADVANCED_FACE ( 'NONE', ( #3024 ), #27808, .F. ) ;
#29251 = DIRECTION ( 'NONE',  ( 0.000000000000000000, 0.000000000000000000, 1.000000000000000000 ) ) ;
#29252 = VERTEX_POINT ( 'NONE', #6066 ) ;
#29253 = CARTESIAN_POINT ( 'NONE',  ( -12.11431921870781281, -16.53859995802357474, -30.00000000000001066 ) ) ;
#29254 = DIRECTION ( 'NONE',  ( 1.000000000000000000, 0.000000000000000000, 0.000000000000000000 ) ) ;
#29255 = AXIS2_PLACEMENT_3D ( 'NONE', #28649, #15664, #18912 ) ;
#29256 = DIRECTION ( 'NONE',  ( 0.000000000000000000, 0.000000000000000000, 1.000000000000000000 ) ) ;
#29257 = CARTESIAN_POINT ( 'NONE',  ( 14.94108027486234391, 14.43501233363183722, -26.53384665043704871 ) ) ;
#29258 = CARTESIAN_POINT ( 'NONE',  ( 7.125101744601430198, 22.13210201189419379, -22.13446490823594814 ) ) ;
#29259 = EDGE_LOOP ( 'NONE', ( #17905, #12232 ) ) ;
#29260 = DIRECTION ( 'NONE',  ( 0.000000000000000000, 0.000000000000000000, 1.000000000000000000 ) ) ;
#29261 = CARTESIAN_POINT ( 'NONE',  ( -12.41268156625113406, 18.79179606750104981, 12.00000000000000000 ) ) ;
#29262 = CARTESIAN_POINT ( 'NONE',  ( 14.74936230926602754, -24.71673612477145099, -12.49531891550463136 ) ) ;
#29263 = DIRECTION ( 'NONE',  ( 0.8090169943749510040, 0.5877852522924683631, 0.000000000000000000 ) ) ;
#29264 = EDGE_CURVE ( 'NONE', #39078, #36470, #3226, .T. ) ;
#29265 = CYLINDRICAL_SURFACE ( 'NONE', #38648, 0.5000000000000004441 ) ;
#29266 = EDGE_CURVE ( 'NONE', #12503, #15556, #28003, .T. ) ;
#29267 = ORIENTED_EDGE ( 'NONE', *, *, #31190, .F. ) ;
#29268 = CARTESIAN_POINT ( 'NONE',  ( -11.90002364435815885, 19.37375396377245096, -21.61855169659785503 ) ) ;
#29269 = CONICAL_SURFACE ( 'NONE', #24082, 0.9999999999999983347, 0.7853981633974498333 ) ;
#29270 = CARTESIAN_POINT ( 'NONE',  ( -35.98781724630784140, -12.75392035872630991, 15.72805884748931859 ) ) ;
#29271 = CARTESIAN_POINT ( 'NONE',  ( 9.550906370826885095, -18.66785797286095772, -26.24677233048349123 ) ) ;
#29272 = CIRCLE ( 'NONE', #7213, 1.000000000000000888 ) ;
#29273 = FACE_OUTER_BOUND ( 'NONE', #10979, .T. ) ;
#29274 = ORIENTED_EDGE ( 'NONE', *, *, #15871, .T. ) ;
#29275 = ORIENTED_EDGE ( 'NONE', *, *, #13596, .T. ) ;
#29276 = CARTESIAN_POINT ( 'NONE',  ( -13.31194575400795266, 31.44560903785412265, -4.999999999999996447 ) ) ;
#29277 = CYLINDRICAL_SURFACE ( 'NONE', #5512, 6.000000000000003553 ) ;
#29278 = DIRECTION ( 'NONE',  ( 1.000000000000000000, 0.000000000000000000, -0.000000000000000000 ) ) ;
#29279 = CARTESIAN_POINT ( 'NONE',  ( -34.85992093908750178, -7.630325756601307852, -6.756134094771754306 ) ) ;
#29280 = DIRECTION ( 'NONE',  ( 1.000000000000000000, 0.000000000000000000, 0.000000000000000000 ) ) ;
#29281 = VERTEX_POINT ( 'NONE', #15814 ) ;
#29282 = CARTESIAN_POINT ( 'NONE',  ( 29.41927195708630549, 0.2493808729530674062, -10.18512608144294873 ) ) ;
#29283 = CARTESIAN_POINT ( 'NONE',  ( 13.37378135583786332, 20.59160479820249634, 9.500000000000000000 ) ) ;
#29284 = CYLINDRICAL_SURFACE ( 'NONE', #7022, 1.000000000000000000 ) ;
#29285 = CARTESIAN_POINT ( 'NONE',  ( -3.211402178667006169, 32.38366924255629442, 12.00000000000000000 ) ) ;
#29286 = ORIENTED_EDGE ( 'NONE', *, *, #10914, .T. ) ;
#29287 = CARTESIAN_POINT ( 'NONE',  ( -30.49613795931812277, -0.02358107124917707340, -7.827247679823234883 ) ) ;
#29288 = CARTESIAN_POINT ( 'NONE',  ( -5.027400250555931649, 36.23526740290156312, 10.49999999999999822 ) ) ;
#29289 = EDGE_CURVE ( 'NONE', #10554, #29357, #34505, .T. ) ;
#29290 = EDGE_LOOP ( 'NONE', ( #8096, #18190 ) ) ;
#29291 = CARTESIAN_POINT ( 'NONE',  ( 21.47982430794170128, -1.719347241053234221, -24.74632320230637106 ) ) ;
#29292 = CARTESIAN_POINT ( 'NONE',  ( 19.38974044528932339, 6.790579630597447292, -30.00000000000001066 ) ) ;
#29293 = CARTESIAN_POINT ( 'NONE',  ( 30.62963707967951166, -23.89786472172307086, 15.13084544680214094 ) ) ;
#29294 = EDGE_CURVE ( 'NONE', #708, #19619, #9724, .T. ) ;
#29295 = ORIENTED_EDGE ( 'NONE', *, *, #23538, .T. ) ;
#29296 = CARTESIAN_POINT ( 'NONE',  ( 1.732136883776949521, 38.50629078351121137, 16.30093088680190760 ) ) ;
#29297 = CARTESIAN_POINT ( 'NONE',  ( 15.89892447185634339, -25.15199583021764695, 17.92354375535250810 ) ) ;
#29298 = CARTESIAN_POINT ( 'NONE',  ( 13.94482798346721353, 26.50521816028912525, 11.00000000000000000 ) ) ;
#29299 = CARTESIAN_POINT ( 'NONE',  ( 6.290729337820269329, 29.14951258272645163, 20.50957957746029692 ) ) ;
#29300 = AXIS2_PLACEMENT_3D ( 'NONE', #10769, #19708, #29652 ) ;
#29301 = FACE_OUTER_BOUND ( 'NONE', #10669, .T. ) ;
#29302 = AXIS2_PLACEMENT_3D ( 'NONE', #31296, #16051, #3461 ) ;
#29303 = FACE_OUTER_BOUND ( 'NONE', #34371, .T. ) ;
#29304 = CARTESIAN_POINT ( 'NONE',  ( 5.194952508988293971, 31.55601946072578912, -13.85024353354532423 ) ) ;
#29305 = DIRECTION ( 'NONE',  ( 1.000000000000000000, 0.000000000000000000, 0.000000000000000000 ) ) ;
#29306 = CARTESIAN_POINT ( 'NONE',  ( 18.88552629894499546, 10.90356369248356572, 18.87996532025784902 ) ) ;
#29307 = CARTESIAN_POINT ( 'NONE',  ( -21.08026172065598303, 11.39671773059110471, -11.88141413567837645 ) ) ;
#29308 = VECTOR ( 'NONE', #4496, 1000.000000000000227 ) ;
#29309 = CARTESIAN_POINT ( 'NONE',  ( 20.01903129369064516, -26.18370256011770536, -9.488982841011081248 ) ) ;
#29310 = DIRECTION ( 'NONE',  ( 0.1045284632676570929, 0.9945218953682729568, 0.000000000000000000 ) ) ;
#29311 = CARTESIAN_POINT ( 'NONE',  ( -13.28731253931435319, 15.83618351362805043, 10.49999999999999822 ) ) ;
#29312 = ORIENTED_EDGE ( 'NONE', *, *, #7321, .T. ) ;
#29313 = CARTESIAN_POINT ( 'NONE',  ( 10.91553583107620007, 17.35227997941746025, -29.99999999999999289 ) ) ;
#29314 = ORIENTED_EDGE ( 'NONE', *, *, #11618, .F. ) ;
#29315 = CARTESIAN_POINT ( 'NONE',  ( -15.68533655378858249, 25.84264350341399208, -5.000000000000000000 ) ) ;
#29316 = CARTESIAN_POINT ( 'NONE',  ( -26.58217467610690932, -19.30423083005489104, 19.99202127657103389 ) ) ;
#29317 = CARTESIAN_POINT ( 'NONE',  ( 4.475131784526629630, 8.183115020678576101, 7.000000000000000000 ) ) ;
#29318 = CARTESIAN_POINT ( 'NONE',  ( 11.05794297925115721, 17.31467482071210995, -28.70911162413052509 ) ) ;
#29319 = VERTEX_POINT ( 'NONE', #4419 ) ;
#29320 = CARTESIAN_POINT ( 'NONE',  ( 32.95544229134011260, -19.49942389514326280, -6.696085395276597296 ) ) ;
#29321 = EDGE_CURVE ( 'NONE', #24512, #17938, #22697, .T. ) ;
#29322 = ORIENTED_EDGE ( 'NONE', *, *, #32788, .F. ) ;
#29324 = PLANE ( 'NONE',  #14054 ) ;
#29323 = CARTESIAN_POINT ( 'NONE',  ( -11.73230135076743430, 19.55154583864819529, -21.58659322360452038 ) ) ;
#29325 = CARTESIAN_POINT ( 'NONE',  ( -16.19425115350092170, -26.23270428128562060, -9.181978510543402194 ) ) ;
#29326 = DIRECTION ( 'NONE',  ( 0.000000000000000000, 0.000000000000000000, -1.000000000000000000 ) ) ;
#29327 = ORIENTED_EDGE ( 'NONE', *, *, #35101, .T. ) ;
#29328 = CARTESIAN_POINT ( 'NONE',  ( -21.86307784644980856, -9.053974127840067609, -21.89187085695087731 ) ) ;
#29329 = CARTESIAN_POINT ( 'NONE',  ( -9.042611116926241976, -18.44506910216152207, -28.72510403185944838 ) ) ;
#29330 = CARTESIAN_POINT ( 'NONE',  ( 24.28032989564874811, -12.76774640304083874, 23.00000000000000000 ) ) ;
#29331 = CARTESIAN_POINT ( 'NONE',  ( 13.62489508051746689, 16.45350914129836184, -24.13972925105511180 ) ) ;
#29332 = ORIENTED_EDGE ( 'NONE', *, *, #14261, .F. ) ;
#29333 = CARTESIAN_POINT ( 'NONE',  ( 20.49112534608896752, 3.798362884196711420, -26.44148346684262307 ) ) ;
#29334 = CARTESIAN_POINT ( 'NONE',  ( 11.54666566735224364, 32.07468077621332725, 7.499999999999997335 ) ) ;
#29335 = DIRECTION ( 'NONE',  ( -0.000000000000000000, -0.000000000000000000, 1.000000000000000000 ) ) ;
#29336 = EDGE_LOOP ( 'NONE', ( #11637, #14239, #3478, #15072 ) ) ;
#29337 = CARTESIAN_POINT ( 'NONE',  ( -20.48845606910846939, 0.6931994281368786259, -29.34533676971968319 ) ) ;
#29338 = CARTESIAN_POINT ( 'NONE',  ( 31.31041380544943209, -0.5838616379220428199, -6.405593367610136646 ) ) ;
#29339 = CARTESIAN_POINT ( 'NONE',  ( 30.06493440560372221, -18.98646248983848395, 18.87996532025784546 ) ) ;
#29340 = ORIENTED_EDGE ( 'NONE', *, *, #29393, .T. ) ;
#29341 = AXIS2_PLACEMENT_3D ( 'NONE', #7695, #1403, #38372 ) ;
#29342 = CARTESIAN_POINT ( 'NONE',  ( -20.39124144463984223, 2.214395427629727742, -30.00000000000000000 ) ) ;
#29343 = CARTESIAN_POINT ( 'NONE',  ( 3.091399026088761826, 22.35909668862748489, -19.80438750953543803 ) ) ;
#29344 = LINE ( 'NONE', #38078, #491 ) ;
#29345 = DIRECTION ( 'NONE',  ( -0.5877852522924791323, -0.8090169943749430104, 6.938893903907231533E-15 ) ) ;
#29346 = CYLINDRICAL_SURFACE ( 'NONE', #21423, 1.000000000000000888 ) ;
#29347 = DIRECTION ( 'NONE',  ( 1.000000000000000000, 0.000000000000000000, 0.000000000000000000 ) ) ;
#29348 = CARTESIAN_POINT ( 'NONE',  ( 40.48557158514985588, -11.25000000000009415, 0.000000000000000000 ) ) ;
#29349 = ORIENTED_EDGE ( 'NONE', *, *, #4912, .T. ) ;
#29350 = LINE ( 'NONE', #13097, #7839 ) ;
#29351 = CARTESIAN_POINT ( 'NONE',  ( -6.654030453887870067, 35.94335816374513115, 7.000000000000000000 ) ) ;
#29352 = CARTESIAN_POINT ( 'NONE',  ( 19.36144844918272057, -17.87459393394177098, -18.75074344801209136 ) ) ;
#29353 = FACE_OUTER_BOUND ( 'NONE', #9822, .T. ) ;
#29354 = DIRECTION ( 'NONE',  ( 1.000000000000000000, 0.000000000000000000, 0.000000000000000000 ) ) ;
#29355 = CARTESIAN_POINT ( 'NONE',  ( 14.99494866545234295, 27.15817369698893557, -7.803426522503517759 ) ) ;
#29356 = DIRECTION ( 'NONE',  ( 1.000000000000000000, 0.000000000000000000, -0.000000000000000000 ) ) ;
#29357 = VERTEX_POINT ( 'NONE', #977 ) ;
#29358 = CARTESIAN_POINT ( 'NONE',  ( -17.79487051664777653, 19.67746942737967686, -6.435833144689066643 ) ) ;
#29359 = CARTESIAN_POINT ( 'NONE',  ( -23.54493052986481771, -14.21898406159468742, 20.99999999999999645 ) ) ;
#29360 = EDGE_CURVE ( 'NONE', #24105, #36787, #3816, .T. ) ;
#29361 = AXIS2_PLACEMENT_3D ( 'NONE', #28432, #19487, #3453 ) ;
#29362 = CARTESIAN_POINT ( 'NONE',  ( 15.31485424103991910, -26.62395559521617727, -6.417108935247511248 ) ) ;
#29363 = FACE_OUTER_BOUND ( 'NONE', #19407, .T. ) ;
#29364 = CARTESIAN_POINT ( 'NONE',  ( 15.18411200369405911, 26.24943595222697112, -8.297974487407337563 ) ) ;
#29365 = ORIENTED_EDGE ( 'NONE', *, *, #11344, .F. ) ;
#29366 = CARTESIAN_POINT ( 'NONE',  ( 10.98205083975412322, 17.31024513893945382, -29.34830281054965795 ) ) ;
#29367 = EDGE_LOOP ( 'NONE', ( #32586, #1287, #37239, #25183 ) ) ;
#29369 = CARTESIAN_POINT ( 'NONE',  ( 14.42035624161478857, 26.65972665747657899, 10.59344459855564580 ) ) ;
#29368 = CARTESIAN_POINT ( 'NONE',  ( -15.07734993948445634, 26.21826188937749080, -8.764079339540616687 ) ) ;
#29370 = CARTESIAN_POINT ( 'NONE',  ( -9.514518717948533322, -18.20889895306638095, -28.70720734546157971 ) ) ;
#29371 = CARTESIAN_POINT ( 'NONE',  ( -34.10020663062403656, -21.93670956716201914, 11.55979286843944820 ) ) ;
#29372 = VECTOR ( 'NONE', #38877, 1000.000000000000000 ) ;
#29373 = CARTESIAN_POINT ( 'NONE',  ( -31.78402004932586422, -20.53790200070664795, -7.546523510580437133 ) ) ;
#29374 = CARTESIAN_POINT ( 'NONE',  ( -9.284007248013184110, -25.41560839480977663, -5.953717583739019936 ) ) ;
#29375 = CARTESIAN_POINT ( 'NONE',  ( 12.77005203192321936, 19.16553846908422187, -20.64983810823187582 ) ) ;
#29376 = EDGE_CURVE ( 'NONE', #35634, #5931, #27976, .T. ) ;
#29377 = VERTEX_POINT ( 'NONE', #7254 ) ;
#29378 = CARTESIAN_POINT ( 'NONE',  ( 22.82816708945120610, 8.056500230395544193, -12.84677774467560951 ) ) ;
#29379 = DIRECTION ( 'NONE',  ( 0.000000000000000000, 0.000000000000000000, 1.000000000000000000 ) ) ;
#29380 = DIRECTION ( 'NONE',  ( 0.000000000000000000, 0.000000000000000000, 1.000000000000000000 ) ) ;
#29381 = ADVANCED_FACE ( 'NONE', ( #13357 ), #20070, .F. ) ;
#29382 = CARTESIAN_POINT ( 'NONE',  ( -1.247473515615844075, 16.63111439559750693, 6.000000000000000000 ) ) ;
#29383 = ORIENTED_EDGE ( 'NONE', *, *, #24147, .F. ) ;
#29384 = CARTESIAN_POINT ( 'NONE',  ( -25.92394411639992313, -1.058492705183743610, -17.26204767525081962 ) ) ;
#29385 = CARTESIAN_POINT ( 'NONE',  ( -11.85876577173794466, 19.91979463210470769, 19.99202127657087402 ) ) ;
#29386 = ORIENTED_EDGE ( 'NONE', *, *, #12593, .T. ) ;
#29387 = CARTESIAN_POINT ( 'NONE',  ( 24.81299795227012339, -13.60183200321584707, 20.99999999999999645 ) ) ;
#29388 = CARTESIAN_POINT ( 'NONE',  ( 8.505700342264139735, 22.10876900990906435, 9.000000000000001776 ) ) ;
#29389 = CARTESIAN_POINT ( 'NONE',  ( 5.706335727061685681, 24.35410196624994583, 12.00000000000000000 ) ) ;
#29390 = CARTESIAN_POINT ( 'NONE',  ( 20.60527582150886872, -9.801935859646480509, -23.00172017847723538 ) ) ;
#29391 = CIRCLE ( 'NONE', #33923, 1.000000000000000000 ) ;
#29392 = CARTESIAN_POINT ( 'NONE',  ( 32.69891748962707112, -23.33280782877936943, 12.73282698324868356 ) ) ;
#29393 = EDGE_CURVE ( 'NONE', #36335, #30133, #1377, .T. ) ;
#29394 = ORIENTED_EDGE ( 'NONE', *, *, #16052, .T. ) ;
#29395 = ADVANCED_FACE ( 'NONE', ( #771 ), #19452, .T. ) ;
#29396 = DIRECTION ( 'NONE',  ( 0.000000000000000000, 0.000000000000000000, 1.000000000000000000 ) ) ;
#29397 = CARTESIAN_POINT ( 'NONE',  ( -0.5000000000000007772, 32.75000000000000000, 10.75000000000000000 ) ) ;
#29398 = AXIS2_PLACEMENT_3D ( 'NONE', #25196, #812, #28440 ) ;
#29399 = DIRECTION ( 'NONE',  ( 0.000000000000000000, 0.000000000000000000, 1.000000000000000000 ) ) ;
#29400 = ORIENTED_EDGE ( 'NONE', *, *, #30624, .T. ) ;
#29401 = CARTESIAN_POINT ( 'NONE',  ( -1.281162814042743125, 25.70428639643705893, -19.63338862114114391 ) ) ;
#29402 = CARTESIAN_POINT ( 'NONE',  ( -14.99771756515323418, 22.21226231334756562, 7.102474990965861323 ) ) ;
#29403 = FACE_OUTER_BOUND ( 'NONE', #26543, .T. ) ;
#29404 = CARTESIAN_POINT ( 'NONE',  ( -1.605702774688126722, 27.44183462127829642, 13.00000000000000178 ) ) ;
#29405 = DIRECTION ( 'NONE',  ( 0.000000000000000000, 0.000000000000000000, -1.000000000000000000 ) ) ;
#29406 = CIRCLE ( 'NONE', #32671, 0.4999999999999989453 ) ;
#29407 = DIRECTION ( 'NONE',  ( 1.000000000000000000, -3.469446951953598806E-15, 0.000000000000000000 ) ) ;
#29408 = CARTESIAN_POINT ( 'NONE',  ( 13.02222589944813613, 25.99981456481483022, -13.33146986105651877 ) ) ;
#29409 = CARTESIAN_POINT ( 'NONE',  ( -12.42073081513906985, 14.75153745115810722, 10.99999999999999822 ) ) ;
#29410 = EDGE_LOOP ( 'NONE', ( #14780, #37860, #38866, #2683, #5059, #3499, #26824 ) ) ;
#29412 = DIRECTION ( 'NONE',  ( 1.000000000000000000, -1.387778780781449147E-14, 0.000000000000000000 ) ) ;
#29411 = CARTESIAN_POINT ( 'NONE',  ( -19.86079119093189860, 13.05667878886535505, -12.88684125302330585 ) ) ;
#29413 = AXIS2_PLACEMENT_3D ( 'NONE', #37692, #35245, #19395 ) ;
#29414 = CARTESIAN_POINT ( 'NONE',  ( -13.84312823610348708, 27.91543399189774632, 10.49999999999999822 ) ) ;
#29415 = CARTESIAN_POINT ( 'NONE',  ( 10.86932238750741675, -19.98308206961400302, -21.61300728401371885 ) ) ;
#29416 = CARTESIAN_POINT ( 'NONE',  ( -12.74038105676665289, 14.56698729810790027, 10.49999999999999822 ) ) ;
#29417 = CARTESIAN_POINT ( 'NONE',  ( 14.91649050592001657, 25.85859626688330337, -9.705674222665134465 ) ) ;
#29418 = CARTESIAN_POINT ( 'NONE',  ( -11.31392148919591811, 36.91540483778867099, -5.000000000000009770 ) ) ;
#29419 = EDGE_CURVE ( 'NONE', #4088, #24813, #35112, .T. ) ;
#29420 = DIRECTION ( 'NONE',  ( -0.000000000000000000, -0.000000000000000000, -1.000000000000000000 ) ) ;
#29421 = VECTOR ( 'NONE', #11317, 1000.000000000000000 ) ;
#29422 = CARTESIAN_POINT ( 'NONE',  ( -27.07092440652241550, -23.98996125867454765, -8.885765738235784639 ) ) ;
#29423 = CARTESIAN_POINT ( 'NONE',  ( 4.352148934427582105, -20.44045777049943879, -25.42944795558441129 ) ) ;
#29424 = CARTESIAN_POINT ( 'NONE',  ( 14.18108264993914247, 23.58463870654085426, -13.53032800031888705 ) ) ;
#29425 = CARTESIAN_POINT ( 'NONE',  ( 17.10314071577965933, 11.30215440122589499, -29.99999999999999645 ) ) ;
#29426 = DIRECTION ( 'NONE',  ( -0.000000000000000000, -0.000000000000000000, -1.000000000000000000 ) ) ;
#29427 = ORIENTED_EDGE ( 'NONE', *, *, #5515, .F. ) ;
#29428 = CARTESIAN_POINT ( 'NONE',  ( -5.618023183903376960, 32.38114438848539578, -12.93671402627438027 ) ) ;
#29429 = ORIENTED_EDGE ( 'NONE', *, *, #11364, .T. ) ;
#29430 = DIRECTION ( 'NONE',  ( 0.9945218953682731788, -0.1045284632676559550, 0.000000000000000000 ) ) ;
#29431 = EDGE_LOOP ( 'NONE', ( #1491, #22470, #9402, #11456 ) ) ;
#29432 = LINE ( 'NONE', #16857, #14156 ) ;
#29433 = CARTESIAN_POINT ( 'NONE',  ( -9.902837789212762587, 25.19189593419573114, 10.74999999999999822 ) ) ;
#29434 = EDGE_LOOP ( 'NONE', ( #31765, #18543, #40069, #24631 ) ) ;
#29435 = CARTESIAN_POINT ( 'NONE',  ( -22.71722914426532114, 0.6555868368756240239, -21.62299990059295496 ) ) ;
#29436 = ORIENTED_EDGE ( 'NONE', *, *, #20581, .F. ) ;
#29437 = CARTESIAN_POINT ( 'NONE',  ( 21.79622464777374446, -5.878312547718441472, -23.18940552536372479 ) ) ;
#29438 = VECTOR ( 'NONE', #521, 1000.000000000000000 ) ;
#29439 = ORIENTED_EDGE ( 'NONE', *, *, #22556, .T. ) ;
#29440 = PRODUCT_CONTEXT ( 'NONE', #24134, 'mechanical' ) ;
#29441 = CARTESIAN_POINT ( 'NONE',  ( -3.607749162633401507, 7.931741834401821123, 10.49999999999999822 ) ) ;
#29442 = VERTEX_POINT ( 'NONE', #16412 ) ;
#29443 = EDGE_CURVE ( 'NONE', #4065, #7337, #5271, .T. ) ;
#29444 = CARTESIAN_POINT ( 'NONE',  ( 11.30736835487432224, 14.81698729810772619, 7.000000000000000000 ) ) ;
#29445 = CARTESIAN_POINT ( 'NONE',  ( -3.713592597587352717, 7.966960743906856379, 7.499999999999997335 ) ) ;
#29446 = CARTESIAN_POINT ( 'NONE',  ( 11.00934640754938165, 31.84548813490947694, 17.92354375535252231 ) ) ;
#29447 = CARTESIAN_POINT ( 'NONE',  ( 13.63581098909226519, 27.45627467658428600, 7.000000000000000000 ) ) ;
#29448 = ORIENTED_EDGE ( 'NONE', *, *, #2442, .F. ) ;
#29449 = DIRECTION ( 'NONE',  ( 1.000000000000000000, 0.000000000000000000, 0.000000000000000000 ) ) ;
#29450 = DIRECTION ( 'NONE',  ( 0.000000000000000000, 0.000000000000000000, 1.000000000000000000 ) ) ;
#29451 = LINE ( 'NONE', #16670, #23401 ) ;
#29452 = CARTESIAN_POINT ( 'NONE',  ( 15.30396852670833496, 13.69301631135325792, -28.83852071831171671 ) ) ;
#29453 = CARTESIAN_POINT ( 'NONE',  ( 8.334627820638896623, 28.79881821608029213, -14.89598926884550956 ) ) ;
#29454 = AXIS2_PLACEMENT_3D ( 'NONE', #16404, #23305, #14159 ) ;
#29455 = EDGE_LOOP ( 'NONE', ( #38726, #23188, #22887, #7924, #36085 ) ) ;
#29456 = CARTESIAN_POINT ( 'NONE',  ( 18.23649648353767461, -16.09146789626181118, 20.99999999999999645 ) ) ;
#29457 = DIRECTION ( 'NONE',  ( 1.000000000000000000, 0.000000000000000000, -0.000000000000000000 ) ) ;
#29458 = CARTESIAN_POINT ( 'NONE',  ( 15.90316971415371050, -26.71736174511572059, -6.876908740700370615 ) ) ;
#29459 = LINE ( 'NONE', #23767, #8747 ) ;
#29460 = CARTESIAN_POINT ( 'NONE',  ( 8.137585970692077453, 29.15429895402930072, 10.50000000000000000 ) ) ;
#29461 = EDGE_CURVE ( 'NONE', #24176, #36229, #4877, .T. ) ;
#29462 = VERTEX_POINT ( 'NONE', #32049 ) ;
#29463 = CARTESIAN_POINT ( 'NONE',  ( -15.01743222564557811, 25.97117291061142552, -9.238173852736359493 ) ) ;
#29464 = AXIS2_PLACEMENT_3D ( 'NONE', #7562, #10821, #19963 ) ;
#29465 = CARTESIAN_POINT ( 'NONE',  ( -23.94800771174391585, -26.22823558801417221, 16.87380292611477728 ) ) ;
#29466 = CARTESIAN_POINT ( 'NONE',  ( 9.977387133527567897, -19.25012270239910350, -23.88382223299232265 ) ) ;
#29467 = ADVANCED_FACE ( 'NONE', ( #19868 ), #38142, .T. ) ;
#29468 = EDGE_CURVE ( 'NONE', #32234, #29912, #31650, .T. ) ;
#29469 = CARTESIAN_POINT ( 'NONE',  ( -13.05736835487441994, 16.11602540378456183, 11.00000000000000000 ) ) ;
#29470 = EDGE_LOOP ( 'NONE', ( #34346, #19235, #6951, #8605 ) ) ;
#29471 = ORIENTED_EDGE ( 'NONE', *, *, #29289, .F. ) ;
#29472 = CARTESIAN_POINT ( 'NONE',  ( -10.02345167188216202, 25.24780830218480432, -16.99244641157628166 ) ) ;
#29473 = FACE_OUTER_BOUND ( 'NONE', #22268, .T. ) ;
#29474 = FACE_BOUND ( 'NONE', #37620, .T. ) ;
#29475 = AXIS2_PLACEMENT_3D ( 'NONE', #20778, #8572, #35610 ) ;
#29476 = EDGE_CURVE ( 'NONE', #39512, #2291, #32467, .T. ) ;
#29477 = CARTESIAN_POINT ( 'NONE',  ( -30.78709934541342008, -6.653293242902037719, -13.05879633663284345 ) ) ;
#29478 = CARTESIAN_POINT ( 'NONE',  ( 8.368303251206119953, 20.48707633493483371, 7.000000000000000000 ) ) ;
#29479 = ORIENTED_EDGE ( 'NONE', *, *, #33257, .T. ) ;
#29480 = CARTESIAN_POINT ( 'NONE',  ( 23.29810041234063078, 0.6049309071670201376, -20.54846396778402351 ) ) ;
#29481 = DIRECTION ( 'NONE',  ( 0.000000000000000000, 0.000000000000000000, 1.000000000000000000 ) ) ;
#29482 = CARTESIAN_POINT ( 'NONE',  ( -8.410254037844433483, 17.06698729810786475, 10.50000000000000000 ) ) ;
#29483 = DIRECTION ( 'NONE',  ( -0.8090169943749426773, 0.5877852522924796874, 0.000000000000000000 ) ) ;
#29484 = UNCERTAINTY_MEASURE_WITH_UNIT (LENGTH_MEASURE( 1.000000000000000082E-05 ), #33951, 'distance_accuracy_value', 'NONE');
#29485 = ORIENTED_EDGE ( 'NONE', *, *, #27694, .F. ) ;
#29486 = CARTESIAN_POINT ( 'NONE',  ( -25.86828471411721964, 0.3106744887170168612, -16.44263060901230133 ) ) ;
#29487 = DIRECTION ( 'NONE',  ( -0.9135454576426031981, 0.4067366430757951568, 0.000000000000000000 ) ) ;
#29488 = EDGE_LOOP ( 'NONE', ( #35082, #27512, #26054, #37057 ) ) ;
#29489 = CARTESIAN_POINT ( 'NONE',  ( 20.53469380938287614, -0.9365662817021573883, -28.64349147984585287 ) ) ;
#29490 = AXIS2_PLACEMENT_3D ( 'NONE', #29049, #17072, #14212 ) ;
#29491 = CARTESIAN_POINT ( 'NONE',  ( 34.34163329534274567, -19.82715122747730163, 14.53008259254011136 ) ) ;
#29492 = ORIENTED_EDGE ( 'NONE', *, *, #7887, .F. ) ;
#29493 = CARTESIAN_POINT ( 'NONE',  ( -15.39524332971155474, 28.62968336403564962, 15.72805884748878746 ) ) ;
#29494 = EDGE_CURVE ( 'NONE', #2390, #32551, #35758, .T. ) ;
#29495 = CARTESIAN_POINT ( 'NONE',  ( -15.74227866052810221, -25.75916161678033234, 17.42190598798392998 ) ) ;
#29496 = ADVANCED_FACE ( 'NONE', ( #1176 ), #25946, .F. ) ;
#29497 = DIRECTION ( 'NONE',  ( 0.000000000000000000, 0.000000000000000000, 1.000000000000000000 ) ) ;
#29498 = EDGE_CURVE ( 'NONE', #28465, #13835, #7459, .T. ) ;
#29499 = CARTESIAN_POINT ( 'NONE',  ( 1.790359260782300899, 30.61752677313665671, 20.69868183039780973 ) ) ;
#29500 = CARTESIAN_POINT ( 'NONE',  ( 14.52509594610762278, 21.97885917798724620, 9.500000000000000000 ) ) ;
#29501 = EDGE_LOOP ( 'NONE', ( #26630, #26495, #15038, #8538 ) ) ;
#29502 = DIRECTION ( 'NONE',  ( 1.000000000000000000, 0.000000000000000000, 0.000000000000000000 ) ) ;
#29503 = AXIS2_PLACEMENT_3D ( 'NONE', #13816, #5083, #38603 ) ;
#29504 = CARTESIAN_POINT ( 'NONE',  ( 4.977190560089425730, 37.49800343037592398, -6.706298034499838856 ) ) ;
#29505 = DIRECTION ( 'NONE',  ( -0.9135454576425986462, 0.4067366430758054263, 0.000000000000000000 ) ) ;
#29506 = CARTESIAN_POINT ( 'NONE',  ( 21.61978140912328072, 6.167694920802003544, 18.87996532025766783 ) ) ;
#29507 = CARTESIAN_POINT ( 'NONE',  ( 21.86335951176813097, -26.92177804972322974, -6.781317475430051367 ) ) ;
#29508 = CARTESIAN_POINT ( 'NONE',  ( -2.853172919594720192, 21.57294901687549427, 13.00000000000000178 ) ) ;
#29509 = CONICAL_SURFACE ( 'NONE', #39883, 0.5000000000000039968, 0.7853981633974480570 ) ;
#29510 = CARTESIAN_POINT ( 'NONE',  ( -13.24038105676665111, 15.43301270189234486, 10.49999999999999822 ) ) ;
#29511 = DIRECTION ( 'NONE',  ( 0.8660254037844431485, 0.4999999999999921174, -0.000000000000000000 ) ) ;
#29512 = ORIENTED_EDGE ( 'NONE', *, *, #10548, .T. ) ;
#29513 = EDGE_CURVE ( 'NONE', #23354, #20669, #30580, .T. ) ;
#29514 = CARTESIAN_POINT ( 'NONE',  ( 11.11465799936758536, 17.80655977757938757, -26.21732550182372989 ) ) ;
#29515 = ORIENTED_EDGE ( 'NONE', *, *, #31009, .T. ) ;
#29516 = CARTESIAN_POINT ( 'NONE',  ( -15.52230086708900991, 25.98154550537155316, -6.889299160236542541 ) ) ;
#29517 = CARTESIAN_POINT ( 'NONE',  ( -29.65272772477494101, -7.615234770328493497, 19.99202127657132522 ) ) ;
#29518 = EDGE_CURVE ( 'NONE', #32217, #18134, #13759, .T. ) ;
#29519 = CARTESIAN_POINT ( 'NONE',  ( -8.541476348891238857, 27.59512447410525127, 6.000000000000000000 ) ) ;
#29520 = CARTESIAN_POINT ( 'NONE',  ( 15.32298969794395305, 26.41742287619900864, -7.358219379429043805 ) ) ;
#29521 = ORIENTED_EDGE ( 'NONE', *, *, #17182, .T. ) ;
#29522 = CARTESIAN_POINT ( 'NONE',  ( 26.02550586683312162, -15.40048236337812604, -15.67641675238316168 ) ) ;
#29523 = ORIENTED_EDGE ( 'NONE', *, *, #30760, .T. ) ;
#29525 = CARTESIAN_POINT ( 'NONE',  ( 4.940908595777814938, 35.94977745735560859, 9.500000000000000000 ) ) ;
#29524 = CARTESIAN_POINT ( 'NONE',  ( -15.03361511047567944, 26.73982999355708401, -8.280263540186123095 ) ) ;
#29526 = CARTESIAN_POINT ( 'NONE',  ( -12.43912898525198507, -20.85335003963435696, -19.38474122678572087 ) ) ;
#29527 = LINE ( 'NONE', #1702, #32213 ) ;
#29528 = ORIENTED_EDGE ( 'NONE', *, *, #12015, .T. ) ;
#29529 = CARTESIAN_POINT ( 'NONE',  ( -18.93673219582609946, -7.851978407254149417, -29.22088221090666593 ) ) ;
#29530 = CARTESIAN_POINT ( 'NONE',  ( -11.20571940622763663, -21.02004376229801252, -19.53273776196371259 ) ) ;
#29531 = CARTESIAN_POINT ( 'NONE',  ( -2.140527761532693418, 7.619874298175171035, 10.50000000000000355 ) ) ;
#29532 = CARTESIAN_POINT ( 'NONE',  ( 16.31817167508792110, 21.23338471077256173, -10.75037980594654385 ) ) ;
#29533 = ORIENTED_EDGE ( 'NONE', *, *, #5690, .F. ) ;
#29534 = CARTESIAN_POINT ( 'NONE',  ( 20.38527744339932468, 3.800983730763423996, -27.02006532963664043 ) ) ;
#29535 = DIRECTION ( 'NONE',  ( 0.000000000000000000, 0.000000000000000000, 1.000000000000000000 ) ) ;
#29536 = CARTESIAN_POINT ( 'NONE',  ( -24.22138565352702955, -9.557272464391553868, 23.00000000000000000 ) ) ;
#29537 = ORIENTED_EDGE ( 'NONE', *, *, #2415, .T. ) ;
#29538 = CARTESIAN_POINT ( 'NONE',  ( -31.09037572277983230, -0.2342870890902537251, -5.472932512709705932 ) ) ;
#29539 = VECTOR ( 'NONE', #35111, 1000.000000000000000 ) ;
#29540 = CARTESIAN_POINT ( 'NONE',  ( 20.72199863514437013, 0.3644282351036394196, -27.41698609587929525 ) ) ;
#29541 = CARTESIAN_POINT ( 'NONE',  ( 26.60725962520467647, -21.34341596033631561, 19.27171037444124480 ) ) ;
#29542 = ORIENTED_EDGE ( 'NONE', *, *, #40176, .T. ) ;
#29543 = CARTESIAN_POINT ( 'NONE',  ( -21.57036019902172441, 1.425437567633411673, -23.93286968654156155 ) ) ;
#29544 = AXIS2_PLACEMENT_3D ( 'NONE', #15127, #27516, #31164 ) ;
#29545 = CARTESIAN_POINT ( 'NONE',  ( 9.163310636333564574, 20.63632441393291117, -29.99999999999999645 ) ) ;
#29546 = CARTESIAN_POINT ( 'NONE',  ( 7.824485034907088021, 10.87986945260446170, 10.00000000000000000 ) ) ;
#29547 = VECTOR ( 'NONE', #39092, 1000.000000000000000 ) ;
#29548 = AXIS2_PLACEMENT_3D ( 'NONE', #33345, #36180, #11794 ) ;
#29549 = CARTESIAN_POINT ( 'NONE',  ( -5.440836655099179353, 34.39106106163288246, 12.00000000000000000 ) ) ;
#29550 = CARTESIAN_POINT ( 'NONE',  ( 19.48557158514982746, -11.25000000000009415, -5.000000000000000000 ) ) ;
#29551 = CARTESIAN_POINT ( 'NONE',  ( 13.63581098909226874, 27.45627467658428955, 7.000000000000000000 ) ) ;
#29552 = CARTESIAN_POINT ( 'NONE',  ( 8.007761790012084546, 9.776959832083274904, 10.49999999999999822 ) ) ;
#29553 = ORIENTED_EDGE ( 'NONE', *, *, #20464, .T. ) ;
#29554 = CARTESIAN_POINT ( 'NONE',  ( -21.61425450235728718, 5.849382257123279416, -19.97008806117738899 ) ) ;
#29555 = DIRECTION ( 'NONE',  ( 0.8660254037844363761, -0.5000000000000039968, -0.000000000000000000 ) ) ;
#29556 = CARTESIAN_POINT ( 'NONE',  ( -17.00000000000000000, 22.50000000000000355, 6.000000000000000000 ) ) ;
#29557 = CARTESIAN_POINT ( 'NONE',  ( 22.37649770465107224, -19.47939514452113841, -15.75872631881709118 ) ) ;
#29558 = CARTESIAN_POINT ( 'NONE',  ( 1.587660364795204782, 9.681887955242936883, 6.000000000000000000 ) ) ;
#29559 = CARTESIAN_POINT ( 'NONE',  ( -14.86556419889030067, 20.43481210330121556, 10.49999999999999822 ) ) ;
#29560 = CARTESIAN_POINT ( 'NONE',  ( 15.26389162175653880, 27.29890105065966921, -5.471704770948925933 ) ) ;
#29561 = DIRECTION ( 'NONE',  ( 1.000000000000000000, 0.000000000000000000, 0.000000000000000000 ) ) ;
#29562 = ORIENTED_EDGE ( 'NONE', *, *, #24791, .T. ) ;
#29563 = CARTESIAN_POINT ( 'NONE',  ( -13.91731628353523220, 15.09031314651060640, -28.80639967540201241 ) ) ;
#29564 = CARTESIAN_POINT ( 'NONE',  ( -23.78345815580402345, -15.17947280105380514, 21.00000000000000000 ) ) ;
#29565 = CARTESIAN_POINT ( 'NONE',  ( 15.31712116136816348, -26.67315282756072747, -5.946102590047462222 ) ) ;
#29566 = DIRECTION ( 'NONE',  ( 0.000000000000000000, 0.000000000000000000, 1.000000000000000000 ) ) ;
#29567 = CARTESIAN_POINT ( 'NONE',  ( 11.90204051271606112, 19.37169779250840307, -21.61878633652037607 ) ) ;
#29568 = ORIENTED_EDGE ( 'NONE', *, *, #23072, .F. ) ;
#29569 = DIRECTION ( 'NONE',  ( 0.000000000000000000, 0.000000000000000000, 1.000000000000000000 ) ) ;
#29570 = EDGE_LOOP ( 'NONE', ( #35688, #18635, #33504, #31680 ) ) ;
#29572 = LINE ( 'NONE', #33242, #25704 ) ;
#29571 = CARTESIAN_POINT ( 'NONE',  ( -15.14941780581691511, 26.36647399290094285, -8.294559382431438976 ) ) ;
#29573 = CARTESIAN_POINT ( 'NONE',  ( -14.57486702249206623, -25.45132688092154893, -10.65428866108198847 ) ) ;
#29574 = CARTESIAN_POINT ( 'NONE',  ( -36.68766582957241695, -16.69324967293977124, 12.14047268033123750 ) ) ;
#29575 = CIRCLE ( 'NONE', #12057, 1.000000000000000888 ) ;
#29576 = AXIS2_PLACEMENT_3D ( 'NONE', #39208, #32928, #21327 ) ;
#29577 = CARTESIAN_POINT ( 'NONE',  ( -23.44121009936221611, -15.14254397387390405, -17.60241826803686394 ) ) ;
#29578 = CARTESIAN_POINT ( 'NONE',  ( -8.902953248278356213, -24.69963661859840087, -10.29415431459782226 ) ) ;
#29579 = CARTESIAN_POINT ( 'NONE',  ( 15.71024529842017436, 24.58213290089141978, -8.311554404203290503 ) ) ;
#29580 = ORIENTED_EDGE ( 'NONE', *, *, #15807, .T. ) ;
#29581 = CARTESIAN_POINT ( 'NONE',  ( 21.76977311220710121, 8.780111591737426835, -14.89262190181197809 ) ) ;
#29582 = CARTESIAN_POINT ( 'NONE',  ( -10.37659643210535698, 39.73422260934387396, 11.00000000000000355 ) ) ;
#29583 = DIRECTION ( 'NONE',  ( 0.000000000000000000, 0.000000000000000000, 1.000000000000000000 ) ) ;
#29584 = DIRECTION ( 'NONE',  ( -0.5877852522924796874, -0.8090169943749426773, 0.000000000000000000 ) ) ;
#29585 = VERTEX_POINT ( 'NONE', #4824 ) ;
#29586 = CARTESIAN_POINT ( 'NONE',  ( -32.95954470968036532, -2.553576478305152886, -5.461075913141677951 ) ) ;
#29587 = CARTESIAN_POINT ( 'NONE',  ( -21.91791918718876175, -0.7365302467875901593, 20.50957957746284066 ) ) ;
#29588 = CARTESIAN_POINT ( 'NONE',  ( 23.74914942275264096, -8.582573258223899160, 20.99999999999999645 ) ) ;
#29589 = DIRECTION ( 'NONE',  ( -1.000000000000000000, 0.000000000000000000, 0.000000000000000000 ) ) ;
#29590 = PLANE ( 'NONE',  #5412 ) ;
#29591 = CARTESIAN_POINT ( 'NONE',  ( 34.19331540110757572, -17.52795661523900961, -5.856166949180161119 ) ) ;
#29592 = DIRECTION ( 'NONE',  ( 0.6691306063588560171, -0.7431448254773962425, 0.000000000000000000 ) ) ;
#29593 = EDGE_CURVE ( 'NONE', #31884, #26227, #26416, .T. ) ;
#29594 = ORIENTED_EDGE ( 'NONE', *, *, #33758, .T. ) ;
#29595 = CARTESIAN_POINT ( 'NONE',  ( 1.605696033269625955, 17.55816537872232530, 13.00000000000000178 ) ) ;
#29596 = CIRCLE ( 'NONE', #34788, 1.000000000000000000 ) ;
#29597 = VECTOR ( 'NONE', #4590, 1000.000000000000000 ) ;
#29598 = CARTESIAN_POINT ( 'NONE',  ( 6.373266493267778721, 35.58529424598359725, 11.00000000000000000 ) ) ;
#29599 = VERTEX_POINT ( 'NONE', #30421 ) ;
#29600 = ADVANCED_FACE ( 'NONE', ( #14370 ), #24312, .F. ) ;
#29601 = CARTESIAN_POINT ( 'NONE',  ( 0.3612209001919436946, 33.46140997383869120, -12.88978858418767715 ) ) ;
#29602 = DIRECTION ( 'NONE',  ( -0.000000000000000000, -0.000000000000000000, -1.000000000000000000 ) ) ;
#29603 = AXIS2_PLACEMENT_3D ( 'NONE', #34862, #13111, #25706 ) ;
#29604 = DIRECTION ( 'NONE',  ( -0.000000000000000000, -0.000000000000000000, -1.000000000000000000 ) ) ;
#29605 = EDGE_CURVE ( 'NONE', #35208, #32427, #5651, .T. ) ;
#29606 = DIRECTION ( 'NONE',  ( 0.000000000000000000, 0.000000000000000000, 1.000000000000000000 ) ) ;
#29607 = CARTESIAN_POINT ( 'NONE',  ( 12.69371393710733642, 14.59393057220526835, 10.76099332938164288 ) ) ;
#29608 = DIRECTION ( 'NONE',  ( 1.000000000000000000, 0.000000000000000000, 0.000000000000000000 ) ) ;
#29609 = CARTESIAN_POINT ( 'NONE',  ( 13.99338577196167321, 26.32572741696355934, -11.50149747935983413 ) ) ;
#29610 = CARTESIAN_POINT ( 'NONE',  ( -9.165211421344535481, 24.66068167190384841, 13.00000000000000178 ) ) ;
#29611 = VERTEX_POINT ( 'NONE', #20678 ) ;
#29613 = DIRECTION ( 'NONE',  ( 1.000000000000000000, 0.000000000000000000, 0.000000000000000000 ) ) ;
#29612 = CARTESIAN_POINT ( 'NONE',  ( -17.97661971344022902, 11.67401855304127523, -22.24591093701263134 ) ) ;
#29614 = CARTESIAN_POINT ( 'NONE',  ( -14.48927117870122316, -30.61587158504648087, 11.00000000000000000 ) ) ;
#29615 = CARTESIAN_POINT ( 'NONE',  ( 15.35992194021738300, -26.51421217328086755, -7.356954887253082553 ) ) ;
#29616 = CARTESIAN_POINT ( 'NONE',  ( -13.76030399595643239, 27.49672490655791535, 11.00000000000000000 ) ) ;
#29617 = CARTESIAN_POINT ( 'NONE',  ( 12.36626470332232763, 20.52366543882663663, -19.49109148384244605 ) ) ;
#29618 = CARTESIAN_POINT ( 'NONE',  ( 16.84920187454417828, 29.09530251867925443, -13.79123840944734880 ) ) ;
#29619 =( BOUNDED_SURFACE ( )  B_SPLINE_SURFACE ( 2, 3, ( 
 ( #24569, #36964, #18675, #9128, #3030, #6073, #21714, #21515, #9332, #18478, #20923, #182, #15422, #27815, #32058, #3231, #12372, #37158 ),
 ( #34116, #15622, #12571, #24963, #5475, #37357, #3425, #25756, #22502, #15821, #6860, #16225, #37955, #22111, #10127, #38152, #35108, #4228 ),
 ( #21908, #9927, #34511, #37559, #28208, #9730, #6660, #28810, #16630, #25162, #31857, #387, #12964, #6466, #13567, #3625, #31660, #31459 ) ),
 .UNSPECIFIED., .F., .F., .F. ) 
 B_SPLINE_SURFACE_WITH_KNOTS ( ( 3, 3 ),
 ( 4, 2, 2, 2, 2, 2, 2, 2, 4 ),
 ( 0.000000000000000000, 1.000000000000000000 ),
 ( 0.2711095619351563957, 0.5960312531500917554, 0.9209529443650270597, 1.245874635579962364, 1.570796326794897668, 1.895718018009833195, 2.220639709224768499, 2.545561400439703803, 2.870483091654639107 ),
 .UNSPECIFIED. ) 
 GEOMETRIC_REPRESENTATION_ITEM ( )  RATIONAL_B_SPLINE_SURFACE ( (
 ( 1.000000000000000000, 1.000000000000000000, 1.000000000000000000, 1.000000000000000000, 1.000000000000000000, 1.000000000000000000, 1.000000000000000000, 1.000000000000000000, 1.000000000000000000, 1.000000000000000000, 1.000000000000000000, 1.000000000000000000, 1.000000000000000000, 1.000000000000000000, 1.000000000000000000, 1.000000000000000000, 1.000000000000000000, 1.000000000000000000),
 ( 0.7071067811865474617, 0.7071067811865474617, 0.7071067811865474617, 0.7071067811865474617, 0.7071067811865473507, 0.7071067811865473507, 0.7071067811865474617, 0.7071067811865474617, 0.7071067811865474617, 0.7071067811865474617, 0.7071067811865475727, 0.7071067811865475727, 0.7071067811865474617, 0.7071067811865474617, 0.7071067811865474617, 0.7071067811865474617, 0.7071067811865474617, 0.7071067811865474617),
 ( 1.000000000000000000, 1.000000000000000000, 1.000000000000000000, 1.000000000000000000, 1.000000000000000000, 1.000000000000000000, 1.000000000000000000, 1.000000000000000000, 1.000000000000000000, 1.000000000000000000, 1.000000000000000000, 1.000000000000000000, 1.000000000000000000, 1.000000000000000000, 1.000000000000000000, 1.000000000000000000, 1.000000000000000000, 1.000000000000000000) ) ) 
 REPRESENTATION_ITEM ( '' )  SURFACE ( )  );
#29620 = FACE_OUTER_BOUND ( 'NONE', #25444, .T. ) ;
#29621 = CARTESIAN_POINT ( 'NONE',  ( -24.25258108503407328, -22.82957551827030684, -12.05318650362971766 ) ) ;
#29622 = CARTESIAN_POINT ( 'NONE',  ( 2.847707569172010622, -20.70244955242776896, -25.48826837884827512 ) ) ;
#29623 = CARTESIAN_POINT ( 'NONE',  ( 13.37878228885757181, 21.93571083929289500, -16.47005970201684377 ) ) ;
#29624 = CARTESIAN_POINT ( 'NONE',  ( 16.68830378044837914, 11.92867436094057787, -29.42711812811024430 ) ) ;
#29625 = DIRECTION ( 'NONE',  ( 0.000000000000000000, 0.000000000000000000, 1.000000000000000000 ) ) ;
#29626 = EDGE_CURVE ( 'NONE', #7910, #27538, #17834, .T. ) ;
#29627 = ORIENTED_EDGE ( 'NONE', *, *, #38183, .T. ) ;
#29628 = CARTESIAN_POINT ( 'NONE',  ( -7.439527340440343472, 36.65827423083189274, -5.866875955026374712 ) ) ;
#29629 = ORIENTED_EDGE ( 'NONE', *, *, #35571, .T. ) ;
#29630 = AXIS2_PLACEMENT_3D ( 'NONE', #30190, #5204, #24091 ) ;
#29631 = CONICAL_SURFACE ( 'NONE', #34815, 1.000000000000004441, 0.7853981633974482790 ) ;
#29632 = DIRECTION ( 'NONE',  ( -0.9781476007338067991, -0.2079116908177533474, 0.000000000000000000 ) ) ;
#29633 = VERTEX_POINT ( 'NONE', #30010 ) ;
#29634 = PLANE ( 'NONE',  #2506 ) ;
#29635 = CARTESIAN_POINT ( 'NONE',  ( 9.381390373406876648, 11.27850996657544513, 10.49999999999999822 ) ) ;
#29636 = VERTEX_POINT ( 'NONE', #33075 ) ;
#29637 = CARTESIAN_POINT ( 'NONE',  ( -29.98443152904168940, 0.2276001790674742065, -8.770443406083204607 ) ) ;
#29638 = ORIENTED_EDGE ( 'NONE', *, *, #25872, .F. ) ;
#29639 = CARTESIAN_POINT ( 'NONE',  ( 19.80298806677364709, -5.334938486795024026, -29.24553249901355656 ) ) ;
#29640 = ORIENTED_EDGE ( 'NONE', *, *, #36427, .T. ) ;
#29641 = PRODUCT_CONTEXT ( 'NONE', #3361, 'mechanical' ) ;
#29642 = CARTESIAN_POINT ( 'NONE',  ( -10.14060191828654212, 25.26915018278947755, 10.00000000000000000 ) ) ;
#29643 = ORIENTED_EDGE ( 'NONE', *, *, #3911, .T. ) ;
#29644 = DIRECTION ( 'NONE',  ( -0.9135454576426005335, 0.4067366430758010409, 0.000000000000000000 ) ) ;
#29645 = CARTESIAN_POINT ( 'NONE',  ( -7.935776944912362296, 22.65328985282726393, 6.000000000000000000 ) ) ;
#29646 = EDGE_CURVE ( 'NONE', #21311, #38258, #35907, .T. ) ;
#29647 = CARTESIAN_POINT ( 'NONE',  ( 1.485997264023448450, 36.23016441347868977, 18.42518152272108622 ) ) ;
#29648 = DIRECTION ( 'NONE',  ( 1.000000000000000000, 0.000000000000000000, 0.000000000000000000 ) ) ;
#29649 = ORIENTED_EDGE ( 'NONE', *, *, #19664, .T. ) ;
#29650 = SHAPE_REPRESENTATION_RELATIONSHIP ( 'NONE' , 'NONE' ,  #28068, #36190 ) ;
#29651 = CARTESIAN_POINT ( 'NONE',  ( 9.941034666242806850, 32.57396620494213124, 7.499999999999997335 ) ) ;
#29652 = DIRECTION ( 'NONE',  ( -0.9510565162951503115, 0.3090169943749572767, 0.000000000000000000 ) ) ;
#29653 = EDGE_CURVE ( 'NONE', #34264, #23249, #10207, .T. ) ;
#29654 = DIRECTION ( 'NONE',  ( -1.000000000000000000, 0.000000000000000000, 0.000000000000000000 ) ) ;
#29655 = CARTESIAN_POINT ( 'NONE',  ( 19.01290250727002018, 16.88526884184630461, -6.928959836932907734 ) ) ;
#29656 = VECTOR ( 'NONE', #25180, 1000.000000000000227 ) ;
#29657 = CARTESIAN_POINT ( 'NONE',  ( 5.802993469575763896, 20.02905561438103987, -27.10461695544125504 ) ) ;
#29658 = AXIS2_PLACEMENT_3D ( 'NONE', #15990, #18643, #37127 ) ;
#29659 = VERTEX_POINT ( 'NONE', #5024 ) ;
#29660 = CARTESIAN_POINT ( 'NONE',  ( -12.28720923544494070, -14.55658080566520418, 20.99999999999999289 ) ) ;
#29661 = CYLINDRICAL_SURFACE ( 'NONE', #14927, 1.000000000000000000 ) ;
#29662 = CARTESIAN_POINT ( 'NONE',  ( 9.870890762638957483, -18.12032902427516490, -28.06054875518065828 ) ) ;
#29663 = CARTESIAN_POINT ( 'NONE',  ( 26.31271763591405133, -28.25584584496056806, -4.999999999999992895 ) ) ;
#29664 = AXIS2_PLACEMENT_3D ( 'NONE', #36302, #20463, #8464 ) ;
#29665 = CARTESIAN_POINT ( 'NONE',  ( -14.81197284684445670, 20.44044478137485399, 10.76099332938164288 ) ) ;
#29666 = CIRCLE ( 'NONE', #16037, 6.000000000000014211 ) ;
#29667 = CARTESIAN_POINT ( 'NONE',  ( -14.92970566726980053, 25.81632110502188127, -9.708005003289713386 ) ) ;
#29668 = CARTESIAN_POINT ( 'NONE',  ( -32.43957513060942688, -23.09559191376246901, 13.92931973827798231 ) ) ;
#29669 = CARTESIAN_POINT ( 'NONE',  ( 10.40875948710034393, -20.60785335237228821, -20.62936224035580679 ) ) ;
#29670 = EDGE_CURVE ( 'NONE', #37999, #34064, #29666, .T. ) ;
#29671 = DIRECTION ( 'NONE',  ( -0.5877852522924791323, -0.8090169943749430104, 0.000000000000000000 ) ) ;
#29672 = ADVANCED_FACE ( 'NONE', ( #32669 ), #29808, .F. ) ;
#29673 = EDGE_LOOP ( 'NONE', ( #6152, #35985, #28588, #33451 ) ) ;
#29674 = ORIENTED_EDGE ( 'NONE', *, *, #22044, .T. ) ;
#29675 = CARTESIAN_POINT ( 'NONE',  ( -10.97358061145035890, 27.71178282933573556, -14.08931735373363736 ) ) ;
#29676 = DIRECTION ( 'NONE',  ( 1.000000000000000000, 0.000000000000000000, 0.000000000000000000 ) ) ;
#29677 = DIRECTION ( 'NONE',  ( -0.000000000000000000, -0.000000000000000000, -1.000000000000000000 ) ) ;
#29678 = CARTESIAN_POINT ( 'NONE',  ( -27.80923940722906096, -4.326673682006865640, -16.00039589016309804 ) ) ;
#29679 = DIRECTION ( 'NONE',  ( -0.1045284632676436176, 0.9945218953682742891, 0.000000000000000000 ) ) ;
#29680 = ORIENTED_EDGE ( 'NONE', *, *, #27748, .F. ) ;
#29681 = CARTESIAN_POINT ( 'NONE',  ( 27.10756907707635222, 0.2822830175333150837, -14.47971340185655720 ) ) ;
#29682 = DIRECTION ( 'NONE',  ( 0.000000000000000000, 0.000000000000000000, 1.000000000000000000 ) ) ;
#29683 = DIRECTION ( 'NONE',  ( -0.000000000000000000, -0.000000000000000000, -1.000000000000000000 ) ) ;
#29684 = CARTESIAN_POINT ( 'NONE',  ( -17.67639428338700114, -29.21024101586626998, 10.99999999999985434 ) ) ;
#29685 = ORIENTED_EDGE ( 'NONE', *, *, #32764, .T. ) ;
#29686 = CARTESIAN_POINT ( 'NONE',  ( -22.73079022145749661, 0.6103013872901770220, -21.61737968283550515 ) ) ;
#29687 = CARTESIAN_POINT ( 'NONE',  ( 11.94134295108989896, 16.18301270189217433, 9.500000000000000000 ) ) ;
#29688 = EDGE_LOOP ( 'NONE', ( #36543, #39082, #25806 ) ) ;
#29689 = CARTESIAN_POINT ( 'NONE',  ( 31.04069800111786037, -4.622072988384480219, -12.21417130457122369 ) ) ;
#29690 = CIRCLE ( 'NONE', #30960, 0.5000000000000000000 ) ;
#29691 = CARTESIAN_POINT ( 'NONE',  ( 36.01097648505593440, -14.57711145883802395, 15.13084544680213384 ) ) ;
#29692 = ORIENTED_EDGE ( 'NONE', *, *, #19694, .T. ) ;
#29693 = CARTESIAN_POINT ( 'NONE',  ( -10.55929393611012124, 36.39458846701819539, 13.92931973827808712 ) ) ;
#29694 = CONICAL_SURFACE ( 'NONE', #18678, 0.9999999999999974465, 0.7853981633974554954 ) ;
#29695 = CARTESIAN_POINT ( 'NONE',  ( -10.81727955708315925, -23.19337658762207965, 18.42518152272366549 ) ) ;
#29696 = DIRECTION ( 'NONE',  ( -0.000000000000000000, -0.000000000000000000, -1.000000000000000000 ) ) ;
#29697 = EDGE_CURVE ( 'NONE', #10198, #15741, #37469, .T. ) ;
#29698 = CARTESIAN_POINT ( 'NONE',  ( -0.8051564177164421965, 29.93655406406123376, 20.82122704794079837 ) ) ;
#29699 = AXIS2_PLACEMENT_3D ( 'NONE', #37278, #9452, #21832 ) ;
#29700 = DIRECTION ( 'NONE',  ( 0.000000000000000000, 0.000000000000000000, 1.000000000000000000 ) ) ;
#29701 = ORIENTED_EDGE ( 'NONE', *, *, #14619, .F. ) ;
#29702 = CARTESIAN_POINT ( 'NONE',  ( -13.00577423375715114, 27.77729443754455829, 10.50000000000000000 ) ) ;
#29703 = EDGE_CURVE ( 'NONE', #22904, #21130, #8067, .T. ) ;
#29704 = CARTESIAN_POINT ( 'NONE',  ( 6.020667366826272904, 36.76097728554005073, -7.565657333014108588 ) ) ;
#29705 = LINE ( 'NONE', #8376, #11302 ) ;
#29706 = CARTESIAN_POINT ( 'NONE',  ( 5.578133564215900009, 24.05045924978373861, 20.99999999999999645 ) ) ;
#29707 = CARTESIAN_POINT ( 'NONE',  ( 14.98275746386106633, -20.98974146216496806, -18.11133193274115172 ) ) ;
#29708 = CARTESIAN_POINT ( 'NONE',  ( -9.340438144419710653, 38.00965938231844632, 10.99999999999994138 ) ) ;
#29709 = AXIS2_PLACEMENT_3D ( 'NONE', #19117, #18920, #31308 ) ;
#29710 = DIRECTION ( 'NONE',  ( 0.000000000000000000, 0.000000000000000000, 1.000000000000000000 ) ) ;
#29711 = CARTESIAN_POINT ( 'NONE',  ( 2.231660708550581962, 7.803782283739836956, 10.49999999999999822 ) ) ;
#29712 = ORIENTED_EDGE ( 'NONE', *, *, #36181, .F. ) ;
#29713 = CARTESIAN_POINT ( 'NONE',  ( 14.49168446761245121, 25.08686542864395719, -11.59031123052781176 ) ) ;
#29714 = CIRCLE ( 'NONE', #21281, 18.00000000000000000 ) ;
#29715 = ORIENTED_EDGE ( 'NONE', *, *, #32753, .F. ) ;
#29717 = CIRCLE ( 'NONE', #12202, 1.000000000000000000 ) ;
#29716 = CARTESIAN_POINT ( 'NONE',  ( -12.17635432242331639, 19.07997197433500958, -21.66576389041598816 ) ) ;
#29718 = CARTESIAN_POINT ( 'NONE',  ( -28.25018339770791087, -2.647087534802860187, 19.27171037444157164 ) ) ;
#29719 = CARTESIAN_POINT ( 'NONE',  ( 4.058514655873871391, 8.059341904692812975, 7.339470489435487188 ) ) ;
#29720 = CARTESIAN_POINT ( 'NONE',  ( 13.25152841075581023, 22.16086677354865841, -16.45058133833084568 ) ) ;
#29721 = VERTEX_POINT ( 'NONE', #36112 ) ;
#29722 = CARTESIAN_POINT ( 'NONE',  ( 20.46135049998398969, -12.10462214192124897, -21.83542778586768307 ) ) ;
#29723 = ORIENTED_EDGE ( 'NONE', *, *, #1407, .F. ) ;
#29724 = VECTOR ( 'NONE', #3015, 1000.000000000000000 ) ;
#29726 = LINE ( 'NONE', #5340, #1743 ) ;
#29725 = CARTESIAN_POINT ( 'NONE',  ( -11.10899655815487286, 18.75408899665464091, -23.79491269033197298 ) ) ;
#29727 = CARTESIAN_POINT ( 'NONE',  ( -16.30272796611154362, -25.72258041950212970, -10.55552886378998068 ) ) ;
#29728 = DIRECTION ( 'NONE',  ( 0.4539904997395342034, -0.8910065241883743381, -1.196099074440426220E-16 ) ) ;
#29729 = EDGE_CURVE ( 'NONE', #27275, #17659, #14741, .T. ) ;
#29730 = ORIENTED_EDGE ( 'NONE', *, *, #38781, .F. ) ;
#29731 = CARTESIAN_POINT ( 'NONE',  ( -19.39494709936099781, -7.365632527046459543, -27.74002402222404484 ) ) ;
#29732 = CARTESIAN_POINT ( 'NONE',  ( -13.16152623113992348, -24.05409641368920504, -13.53816783273080127 ) ) ;
#29733 = LINE ( 'NONE', #23836, #7960 ) ;
#29734 = CARTESIAN_POINT ( 'NONE',  ( 14.38663302965268542, 17.85124432971809583, -19.80540727126786393 ) ) ;
#29735 = ORIENTED_EDGE ( 'NONE', *, *, #70, .T. ) ;
#29736 = CARTESIAN_POINT ( 'NONE',  ( 23.72444218837145158, 2.197028041356958727, -18.63410458577873285 ) ) ;
#29737 = CARTESIAN_POINT ( 'NONE',  ( -8.229154955995012344, 10.32288908946084760, 10.96580508970281187 ) ) ;
#29738 = CARTESIAN_POINT ( 'NONE',  ( -35.72300736400992349, -23.12593624637962719, 22.99999999999905498 ) ) ;
#29739 = EDGE_LOOP ( 'NONE', ( #6047, #1534, #6775, #39727 ) ) ;
#29740 = CARTESIAN_POINT ( 'NONE',  ( -30.90771625177988113, -0.2200328037497713274, -6.882354936934209633 ) ) ;
#29741 = CARTESIAN_POINT ( 'NONE',  ( 25.48014744351514693, -0.1196400326508215983, -17.37346584602176591 ) ) ;
#29742 = CARTESIAN_POINT ( 'NONE',  ( 21.70013981686734894, -23.40282575515950825, 19.27171037444156809 ) ) ;
#29743 = EDGE_LOOP ( 'NONE', ( #8757, #929, #22249, #11897 ) ) ;
#29744 = CARTESIAN_POINT ( 'NONE',  ( -29.21107446086027082, 1.733986180571661873, -5.474071973575725281 ) ) ;
#29745 = CARTESIAN_POINT ( 'NONE',  ( -18.07620401364299667, 24.68088026512193522, -5.000000000000000000 ) ) ;
#29746 = EDGE_CURVE ( 'NONE', #32987, #16453, #8913, .T. ) ;
#29747 = DIRECTION ( 'NONE',  ( 0.4999999999999920619, -0.8660254037844432595, 0.000000000000000000 ) ) ;
#29748 = VECTOR ( 'NONE', #1814, 999.9999999999998863 ) ;
#29749 = AXIS2_PLACEMENT_3D ( 'NONE', #11006, #39225, #35786 ) ;
#29750 = DIRECTION ( 'NONE',  ( 1.000000000000000000, 0.000000000000000000, 0.000000000000000000 ) ) ;
#29751 = ADVANCED_FACE ( 'NONE', ( #7864 ), #24111, .T. ) ;
#29752 = CIRCLE ( 'NONE', #16765, 18.00000000000002842 ) ;
#29753 = VECTOR ( 'NONE', #9306, 1000.000000000000227 ) ;
#29754 = ADVANCED_FACE ( 'NONE', ( #5619 ), #36313, .F. ) ;
#29755 = DIRECTION ( 'NONE',  ( 0.000000000000000000, 0.000000000000000000, 1.000000000000000000 ) ) ;
#29756 = CARTESIAN_POINT ( 'NONE',  ( 0.000000000000000000, 22.50000000000000355, 7.000000000000000000 ) ) ;
#29757 = DIRECTION ( 'NONE',  ( -0.000000000000000000, -0.000000000000000000, -1.000000000000000000 ) ) ;
#29758 = VERTEX_POINT ( 'NONE', #20875 ) ;
#29759 = CARTESIAN_POINT ( 'NONE',  ( -23.53550312530761346, 5.153870508594805777, -15.77917154867632732 ) ) ;
#29760 = CARTESIAN_POINT ( 'NONE',  ( 12.05833259093393117, 18.99598562053712314, -30.00000000000000000 ) ) ;
#29761 = DIRECTION ( 'NONE',  ( -1.000000000000000000, 0.000000000000000000, 0.000000000000000000 ) ) ;
#29762 = CARTESIAN_POINT ( 'NONE',  ( 23.61345955422964948, -23.17554374091795566, -12.06964299242005545 ) ) ;
#29763 = CARTESIAN_POINT ( 'NONE',  ( -8.927394655428429360, 11.06314620770957013, 7.000000000000000000 ) ) ;
#29764 = CARTESIAN_POINT ( 'NONE',  ( -14.50704651774856835, 20.00412295564782283, 10.49999999999999822 ) ) ;
#29765 = CARTESIAN_POINT ( 'NONE',  ( 14.61867237244439721, 25.74613599029391153, -10.63056160451222532 ) ) ;
#29766 = ORIENTED_EDGE ( 'NONE', *, *, #18466, .F. ) ;
#29767 = CARTESIAN_POINT ( 'NONE',  ( -16.59571780117528306, 22.97185772529794434, -4.999999999999999112 ) ) ;
#29768 = CARTESIAN_POINT ( 'NONE',  ( -23.05386822411328041, -7.747535282638268406, 20.99999999999999645 ) ) ;
#29769 = CARTESIAN_POINT ( 'NONE',  ( 9.534133013345522656, -18.29165158992863738, -28.07943093716786720 ) ) ;
#29770 = CARTESIAN_POINT ( 'NONE',  ( -7.824485034907249670, 10.87986945260456295, 7.499999999999999112 ) ) ;
#29771 = CARTESIAN_POINT ( 'NONE',  ( 15.37593855497895134, 26.65856383457258261, -6.417017949581364178 ) ) ;
#29772 = ORIENTED_EDGE ( 'NONE', *, *, #17772, .F. ) ;
#29773 = FACE_OUTER_BOUND ( 'NONE', #13198, .T. ) ;
#29774 = ORIENTED_EDGE ( 'NONE', *, *, #11997, .T. ) ;
#29776 = DIRECTION ( 'NONE',  ( 1.000000000000000000, 0.000000000000000000, 0.000000000000000000 ) ) ;
#29775 = CARTESIAN_POINT ( 'NONE',  ( -13.97834737394524396, 24.06032382748300691, -13.50144991984861775 ) ) ;
#29777 = EDGE_CURVE ( 'NONE', #39013, #7898, #17369, .T. ) ;
#29778 = CARTESIAN_POINT ( 'NONE',  ( -9.487969581998370927, -18.17220041443854583, -30.00000000000000000 ) ) ;
#29779 = CARTESIAN_POINT ( 'NONE',  ( -22.73078996736959922, -29.06185046644121428, 10.99999999999970868 ) ) ;
#29780 = ADVANCED_FACE ( 'NONE', ( #12908 ), #22518, .T. ) ;
#29781 = AXIS2_PLACEMENT_3D ( 'NONE', #34266, #31018, #34462 ) ;
#29782 = CARTESIAN_POINT ( 'NONE',  ( -18.00895331265001076, -11.61959776305488923, -25.58275405777271416 ) ) ;
#29783 = CARTESIAN_POINT ( 'NONE',  ( -6.481551405175245861, -23.88552407126505628, -12.80164040886976196 ) ) ;
#29784 = CARTESIAN_POINT ( 'NONE',  ( 11.55093992908412126, 16.93669310835906572, -30.00000000000000000 ) ) ;
#29785 = ORIENTED_EDGE ( 'NONE', *, *, #33279, .T. ) ;
#29786 = CARTESIAN_POINT ( 'NONE',  ( 25.30102210956597020, 6.478166462252010760, -5.958356417954576933 ) ) ;
#29787 = DIRECTION ( 'NONE',  ( 0.000000000000000000, 0.000000000000000000, -1.000000000000000000 ) ) ;
#29788 = CARTESIAN_POINT ( 'NONE',  ( -13.01838097023000707, 23.73363068877903359, 6.000000000000000000 ) ) ;
#29789 = CARTESIAN_POINT ( 'NONE',  ( 2.036571916123615100, 8.108948098542045457, 10.49999999999999467 ) ) ;
#29790 = VECTOR ( 'NONE', #27251, 1000.000000000000000 ) ;
#29791 = ORIENTED_EDGE ( 'NONE', *, *, #27152, .T. ) ;
#29792 = CARTESIAN_POINT ( 'NONE',  ( -20.48034806427134313, -1.125288817275917008, -30.00000000000000000 ) ) ;
#29793 = CARTESIAN_POINT ( 'NONE',  ( -10.32110568927837413, 19.34973993761487066, 20.50957957746001981 ) ) ;
#29794 = CARTESIAN_POINT ( 'NONE',  ( 24.85114452701355958, -15.17411596029600851, 20.94377226548378346 ) ) ;
#29795 = LINE ( 'NONE', #1564, #21339 ) ;
#29796 = EDGE_CURVE ( 'NONE', #18134, #11440, #15403, .T. ) ;
#29797 = DIRECTION ( 'NONE',  ( -0.000000000000000000, -0.000000000000000000, -1.000000000000000000 ) ) ;
#29798 = EDGE_CURVE ( 'NONE', #2507, #26077, #36170, .T. ) ;
#29799 = VERTEX_POINT ( 'NONE', #9075 ) ;
#29800 = DIRECTION ( 'NONE',  ( 1.000000000000000000, 0.000000000000000000, 0.000000000000000000 ) ) ;
#29801 = CIRCLE ( 'NONE', #28516, 1.000000000000000888 ) ;
#29802 = DIRECTION ( 'NONE',  ( -0.9135454576426006446, 0.4067366430758009299, 0.000000000000000000 ) ) ;
#29803 = CARTESIAN_POINT ( 'NONE',  ( -9.997483185316569987, 21.95197631500770896, 10.49999999999999467 ) ) ;
#29804 = CARTESIAN_POINT ( 'NONE',  ( 1.384233241701591899, 33.43667168175883830, -12.89082250209952640 ) ) ;
#29805 = DIRECTION ( 'NONE',  ( 0.000000000000000000, 0.000000000000000000, 1.000000000000000000 ) ) ;
#29806 = CARTESIAN_POINT ( 'NONE',  ( 12.41267482483262796, 26.20820393249957192, 13.00000000000000178 ) ) ;
#29807 = VECTOR ( 'NONE', #18313, 999.9999999999998863 ) ;
#29808 = PLANE ( 'NONE',  #20610 ) ;
#29809 = FACE_OUTER_BOUND ( 'NONE', #39873, .T. ) ;
#29810 = CYLINDRICAL_SURFACE ( 'NONE', #30093, 1.000000000000000888 ) ;
#29811 = CARTESIAN_POINT ( 'NONE',  ( 11.40974394891913057, 20.73802190120719047, -20.40291310562222193 ) ) ;
#29812 = PLANE ( 'NONE',  #26997 ) ;
#29813 = ORIENTED_EDGE ( 'NONE', *, *, #20537, .T. ) ;
#29815 = LINE ( 'NONE', #39358, #5763 ) ;
#29814 = CARTESIAN_POINT ( 'NONE',  ( -18.71293717657318112, 16.10063966046890727, -10.85465713401838705 ) ) ;
#29816 = CARTESIAN_POINT ( 'NONE',  ( -0.4999999999999998890, 37.39061994947694245, 10.82238861112329076 ) ) ;
#29817 = CARTESIAN_POINT ( 'NONE',  ( 10.00012431106257083, -18.80013087926857196, -25.01062988768326179 ) ) ;
#29818 = CARTESIAN_POINT ( 'NONE',  ( 5.490944681523308724, 34.83286367817510154, 7.000000000000000000 ) ) ;
#29819 = CARTESIAN_POINT ( 'NONE',  ( 10.97849594700618425, 17.36583575188205941, -28.70580706648543412 ) ) ;
#29820 = DIRECTION ( 'NONE',  ( 0.000000000000000000, 0.000000000000000000, -1.000000000000000000 ) ) ;
#29821 = CARTESIAN_POINT ( 'NONE',  ( -8.593266739736659332, 16.38397459621564067, 10.49999999999999822 ) ) ;
#29822 = CARTESIAN_POINT ( 'NONE',  ( -26.85786336487645798, -23.80939247740336029, -9.326638227506361289 ) ) ;
#29823 = CARTESIAN_POINT ( 'NONE',  ( 1.811844033679846255, -24.72003103208043839, -6.454257893813014846 ) ) ;
#29824 = CARTESIAN_POINT ( 'NONE',  ( 12.05618289028952894, 19.20794177042097317, -21.64528753798118998 ) ) ;
#29825 = CARTESIAN_POINT ( 'NONE',  ( 17.23802802930360301, 12.42931764800617422, -23.31302680604725808 ) ) ;
#29826 = LINE ( 'NONE', #2011, #13440 ) ;
#29827 = EDGE_CURVE ( 'NONE', #5736, #24952, #2977, .T. ) ;
#29828 = VERTEX_POINT ( 'NONE', #2775 ) ;
#29829 = CARTESIAN_POINT ( 'NONE',  ( -6.749652402378329086, 32.93967545494245286, -12.03137183237044994 ) ) ;
#29830 = VERTEX_POINT ( 'NONE', #27557 ) ;
#29831 = CIRCLE ( 'NONE', #35665, 1.000000000000000000 ) ;
#29832 = CARTESIAN_POINT ( 'NONE',  ( 14.61656768153249786, 21.96308928146552120, 10.49999999999999822 ) ) ;
#29833 = VERTEX_POINT ( 'NONE', #34058 ) ;
#29834 = CARTESIAN_POINT ( 'NONE',  ( 8.917734535019441466, 14.47043272369397116, 12.00000000000000000 ) ) ;
#29835 = CARTESIAN_POINT ( 'NONE',  ( 9.417813166173738537, 10.93662330136606009, 10.49999999999999822 ) ) ;
#29836 = CIRCLE ( 'NONE', #2584, 1.000000000000000888 ) ;
#29837 = ORIENTED_EDGE ( 'NONE', *, *, #18379, .F. ) ;
#29838 = CARTESIAN_POINT ( 'NONE',  ( -30.27639200216978921, 0.2080803662807323429, -7.829370471578710244 ) ) ;
#29839 = ORIENTED_EDGE ( 'NONE', *, *, #23558, .F. ) ;
#29840 = CARTESIAN_POINT ( 'NONE',  ( 34.53444588180299490, -11.54643433007243658, -8.446032751583265608 ) ) ;
#29841 = ORIENTED_EDGE ( 'NONE', *, *, #24797, .F. ) ;
#29842 = SHAPE_DEFINITION_REPRESENTATION ( #22001, #8618 ) ;
#29843 = CARTESIAN_POINT ( 'NONE',  ( -0.4999999999999998890, 37.13089969389958611, 11.00000000000000178 ) ) ;
#29844 = ORIENTED_EDGE ( 'NONE', *, *, #18199, .T. ) ;
#29845 = LINE ( 'NONE', #10762, #32694 ) ;
#29846 = DIRECTION ( 'NONE',  ( 1.000000000000000000, 0.000000000000000000, 0.000000000000000000 ) ) ;
#29847 = B_SPLINE_CURVE_WITH_KNOTS ( 'NONE', 3,
 ( #6202, #4504, #854, #10601, #34240, #6930, #37085, #34043, #1260, #3895, #37283, #4299, #13234, #32137, #9255, #22579, #21837, #28882 ),
 .UNSPECIFIED., .F., .F.,
 ( 4, 2, 2, 2, 2, 2, 2, 2, 4 ),
 ( 0.000000000000000000, 0.08767908505624519289, 0.1753581701124903858, 0.2630372551687354954, 0.3507163402249806605, 0.4383954252812256591, 0.5260745103374705467, 0.6137535953937155453, 0.7014326804499604329 ),
 .UNSPECIFIED. ) ;
#29848 = DIRECTION ( 'NONE',  ( 0.000000000000000000, 0.000000000000000000, 1.000000000000000000 ) ) ;
#29849 = ORIENTED_EDGE ( 'NONE', *, *, #32363, .F. ) ;
#29850 = CARTESIAN_POINT ( 'NONE',  ( -15.51137734265978452, -13.41919184397205989, -30.00000000000002842 ) ) ;
#29851 = DIRECTION ( 'NONE',  ( 0.000000000000000000, 0.000000000000000000, -1.000000000000000000 ) ) ;
#29852 = ADVANCED_FACE ( 'NONE', ( #28152 ), #15167, .F. ) ;
#29853 = CARTESIAN_POINT ( 'NONE',  ( -4.817371740575545402, 23.83900317890010001, 23.00000000000000000 ) ) ;
#29854 = CARTESIAN_POINT ( 'NONE',  ( 15.03591831393239353, 14.57499296974832781, -25.40006105580101092 ) ) ;
#29855 = CARTESIAN_POINT ( 'NONE',  ( 11.29805954857153516, 32.07545058919369296, -9.425914070865543337 ) ) ;
#29856 = ORIENTED_EDGE ( 'NONE', *, *, #8762, .F. ) ;
#29857 = DIRECTION ( 'NONE',  ( -1.000000000000000000, 0.000000000000000000, 0.000000000000000000 ) ) ;
#29858 = DIRECTION ( 'NONE',  ( -0.000000000000000000, -0.000000000000000000, -1.000000000000000000 ) ) ;
#29859 = CARTESIAN_POINT ( 'NONE',  ( 15.74830575105852226, -26.80738400109229147, -5.000000000000000888 ) ) ;
#29860 = CARTESIAN_POINT ( 'NONE',  ( 17.21213525677114120, -20.06193531423683041, 20.50957957746029336 ) ) ;
#29861 = CIRCLE ( 'NONE', #27291, 0.5000000000000000000 ) ;
#29862 = LINE ( 'NONE', #14424, #5588 ) ;
#29863 = CARTESIAN_POINT ( 'NONE',  ( -11.47017161796830820, 18.44952784731361461, -23.85172870555624769 ) ) ;
#29864 = CARTESIAN_POINT ( 'NONE',  ( -36.30242391553720438, -14.63578948164528981, 14.53008259254010959 ) ) ;
#29865 = CARTESIAN_POINT ( 'NONE',  ( 12.69460418788277778, -24.00195335915195471, -13.55933954820171117 ) ) ;
#29866 = EDGE_CURVE ( 'NONE', #2121, #1690, #1777, .T. ) ;
#29867 = CARTESIAN_POINT ( 'NONE',  ( 5.082600654608392610, 21.41965916404854298, 13.00000000000000178 ) ) ;
#29868 = VERTEX_POINT ( 'NONE', #15964 ) ;
#29869 = EDGE_LOOP ( 'NONE', ( #8597, #19713, #29594, #20182 ) ) ;
#29870 = CARTESIAN_POINT ( 'NONE',  ( -11.48376733107994063, 31.82382468019164534, -9.435985624090092116 ) ) ;
#29871 = DIRECTION ( 'NONE',  ( 0.000000000000000000, 0.000000000000000000, 1.000000000000000000 ) ) ;
#29872 = DIRECTION ( 'NONE',  ( 1.000000000000000000, 0.000000000000000000, 0.000000000000000000 ) ) ;
#29873 = AXIS2_PLACEMENT_3D ( 'NONE', #19446, #25939, #32457 ) ;
#29874 = CARTESIAN_POINT ( 'NONE',  ( -33.14594191503550036, -6.195422458497144014, -9.876726191397294130 ) ) ;
#29875 = DIRECTION ( 'NONE',  ( 0.000000000000000000, 0.000000000000000000, 1.000000000000000000 ) ) ;
#29876 = EDGE_LOOP ( 'NONE', ( #30632, #14838, #19691, #1370, #4080, #39176, #31825, #1497 ) ) ;
#29877 = CARTESIAN_POINT ( 'NONE',  ( 28.83991352859764845, 0.1616784926268942935, -11.60121644625366777 ) ) ;
#29878 = ADVANCED_FACE ( 'NONE', ( #15566 ), #6410, .T. ) ;
#29879 = AXIS2_PLACEMENT_3D ( 'NONE', #15563, #27950, #124 ) ;
#29880 = CARTESIAN_POINT ( 'NONE',  ( 11.44169217588633636, 32.12932954397578555, 10.76099332938163755 ) ) ;
#29881 = PLANE ( 'NONE',  #29749 ) ;
#29882 = CARTESIAN_POINT ( 'NONE',  ( -25.76746751309237737, -28.17378816281799558, 10.99999999999996625 ) ) ;
#29883 = ADVANCED_FACE ( 'NONE', ( #28345 ), #22055, .F. ) ;
#29884 = EDGE_LOOP ( 'NONE', ( #27662, #33515, #26537, #11232 ) ) ;
#29885 = CARTESIAN_POINT ( 'NONE',  ( -30.89051437471967887, -0.02824647624105855806, -5.474200716472483741 ) ) ;
#29886 = FACE_OUTER_BOUND ( 'NONE', #30299, .T. ) ;
#29887 = ORIENTED_EDGE ( 'NONE', *, *, #20812, .T. ) ;
#29888 = CARTESIAN_POINT ( 'NONE',  ( 25.96735800389505400, -3.809743913480001964, -17.99300411472922079 ) ) ;
#29889 = CARTESIAN_POINT ( 'NONE',  ( 35.82891851945763761, -9.175709056023070076, 15.72805884748939853 ) ) ;
#29890 = VERTEX_POINT ( 'NONE', #40142 ) ;
#29891 = CARTESIAN_POINT ( 'NONE',  ( -16.24129362380272212, 27.01431713449522221, 15.13084544680213561 ) ) ;
#29892 = AXIS2_PLACEMENT_3D ( 'NONE', #16966, #27854, #9374 ) ;
#29893 = CARTESIAN_POINT ( 'NONE',  ( 16.23042486174298560, -23.86708630543422416, 18.87996532025784546 ) ) ;
#29894 = CARTESIAN_POINT ( 'NONE',  ( -3.000488737322915878, 30.46850471150003159, 9.000000000000001776 ) ) ;
#29895 = CARTESIAN_POINT ( 'NONE',  ( 8.504221777570171170, 25.88639746736838987, 20.50957957746123128 ) ) ;
#29896 = CARTESIAN_POINT ( 'NONE',  ( 13.81877807188817364, 20.04207961888452871, 10.50000000000000000 ) ) ;
#29897 = ORIENTED_EDGE ( 'NONE', *, *, #18510, .T. ) ;
#29898 = EDGE_CURVE ( 'NONE', #28064, #3290, #33865, .T. ) ;
#29899 = CARTESIAN_POINT ( 'NONE',  ( -39.48557158514991272, -11.24999999999982414, 23.00000000000000000 ) ) ;
#29900 = EDGE_CURVE ( 'NONE', #42, #15406, #37105, .T. ) ;
#29901 = DIRECTION ( 'NONE',  ( 0.000000000000000000, 0.000000000000000000, 1.000000000000000000 ) ) ;
#29902 = EDGE_CURVE ( 'NONE', #13055, #29941, #21854, .T. ) ;
#29903 = CARTESIAN_POINT ( 'NONE',  ( 6.972704631243735740, 35.83133064181360794, -8.442364626267595540 ) ) ;
#29904 = VECTOR ( 'NONE', #820, 1000.000000000000000 ) ;
#29905 = LINE ( 'NONE', #26856, #39840 ) ;
#29906 = CARTESIAN_POINT ( 'NONE',  ( 19.05502067200783500, 4.384649331628448721, 20.25080042701557304 ) ) ;
#29907 = VECTOR ( 'NONE', #36397, 1000.000000000000000 ) ;
#29908 = CARTESIAN_POINT ( 'NONE',  ( 18.97005494646916901, -26.22064284678461021, -9.527288771957310942 ) ) ;
#29909 = CYLINDRICAL_SURFACE ( 'NONE', #1583, 0.5000000000000004441 ) ;
#29910 = DIRECTION ( 'NONE',  ( 1.000000000000000000, 0.000000000000000000, 0.000000000000000000 ) ) ;
#29911 = DIRECTION ( 'NONE',  ( -0.2113248654051873565, 0.7886751345948044278, 0.5773502691896372774 ) ) ;
#29912 = VERTEX_POINT ( 'NONE', #21655 ) ;
#29913 = CARTESIAN_POINT ( 'NONE',  ( 11.41474510619553584, 18.49724849801811288, -23.84291374344302028 ) ) ;
#29914 = EDGE_LOOP ( 'NONE', ( #18269, #6191, #6763, #14287 ) ) ;
#29915 = CARTESIAN_POINT ( 'NONE',  ( -11.74180227034369395, 17.69492043334604503, -25.07106241003591407 ) ) ;
#29916 = CARTESIAN_POINT ( 'NONE',  ( -24.52800942765094305, -23.26501842005211884, 18.87996532025785257 ) ) ;
#29917 = CARTESIAN_POINT ( 'NONE',  ( 4.360713706315008764, 8.147350538441772372, 7.102637441331451029 ) ) ;
#29918 = CARTESIAN_POINT ( 'NONE',  ( 13.27975059410090886, 22.11080264522603755, -16.45492753240296580 ) ) ;
#29919 = ORIENTED_EDGE ( 'NONE', *, *, #25561, .T. ) ;
#29920 = CARTESIAN_POINT ( 'NONE',  ( 24.57022902387958041, -15.56970263708699420, -16.62770197561091479 ) ) ;
#29921 = ORIENTED_EDGE ( 'NONE', *, *, #5509, .T. ) ;
#29923 = FACE_OUTER_BOUND ( 'NONE', #5353, .T. ) ;
#29922 = CARTESIAN_POINT ( 'NONE',  ( -14.87717852953102415, 26.83350838914018155, -8.737445087221045625 ) ) ;
#29924 = CARTESIAN_POINT ( 'NONE',  ( -17.98522147080449329, -26.74354288057798357, -8.201969047480554664 ) ) ;
#29925 = EDGE_CURVE ( 'NONE', #32427, #15193, #18224, .T. ) ;
#29926 = CARTESIAN_POINT ( 'NONE',  ( 17.34253826607186255, 27.32041144404028543, -5.000000000000000000 ) ) ;
#29927 = EDGE_LOOP ( 'NONE', ( #3607, #29286, #18108 ) ) ;
#29928 = CARTESIAN_POINT ( 'NONE',  ( -35.44912448985124342, -12.22065591061644518, -5.865871141610608852 ) ) ;
#29929 = CARTESIAN_POINT ( 'NONE',  ( -10.76246318078418440, -20.54449477115332812, -20.58967632249421342 ) ) ;
#29930 = CARTESIAN_POINT ( 'NONE',  ( 22.38472516250426381, -15.35952186208530357, 23.00000000000000000 ) ) ;
#29931 = EDGE_LOOP ( 'NONE', ( #19659, #36736, #16607, #32098 ) ) ;
#29932 = CARTESIAN_POINT ( 'NONE',  ( 29.62645323178156076, 1.115095990645281532, -6.891287580428307358 ) ) ;
#29933 = CARTESIAN_POINT ( 'NONE',  ( 8.917734535019441466, 14.47043272369397116, 6.000000000000000000 ) ) ;
#29934 = CARTESIAN_POINT ( 'NONE',  ( -0.7344975573282397363, 36.24516302788250499, 6.000000000000000000 ) ) ;
#29935 = EDGE_LOOP ( 'NONE', ( #2732, #25507, #8961, #7285, #11986 ) ) ;
#29936 = CARTESIAN_POINT ( 'NONE',  ( -20.53086226280845139, 0.7723353936895273053, -28.70396588008199856 ) ) ;
#29937 = CARTESIAN_POINT ( 'NONE',  ( 31.77445454197319563, -1.004264897904582954, -5.000000000000000000 ) ) ;
#29938 = VECTOR ( 'NONE', #5867, 1000.000000000000114 ) ;
#29939 = CARTESIAN_POINT ( 'NONE',  ( 30.92601969764218950, -9.797982979853070873, 19.66345542862528006 ) ) ;
#29940 = AXIS2_PLACEMENT_3D ( 'NONE', #30255, #2031, #23753 ) ;
#29941 = VERTEX_POINT ( 'NONE', #31010 ) ;
#29942 = CARTESIAN_POINT ( 'NONE',  ( -28.10180234942462718, 1.777709783175517977, -10.22205278907307502 ) ) ;
#29943 = CARTESIAN_POINT ( 'NONE',  ( -11.31392148919591811, 36.91540483778867099, -14.26382729546508088 ) ) ;
#29944 = DIRECTION ( 'NONE',  ( -0.000000000000000000, -0.000000000000000000, 1.000000000000000000 ) ) ;
#29945 = DIRECTION ( 'NONE',  ( 1.000000000000000000, 0.000000000000000000, 0.000000000000000000 ) ) ;
#29946 = VECTOR ( 'NONE', #28028, 1000.000000000000000 ) ;
#29947 = EDGE_CURVE ( 'NONE', #8857, #10191, #34259, .T. ) ;
#29948 = EDGE_CURVE ( 'NONE', #22045, #12690, #126, .T. ) ;
#29949 = CARTESIAN_POINT ( 'NONE',  ( -4.458872323573595864, 26.51478363815348160, 13.00000000000000178 ) ) ;
#29950 = CARTESIAN_POINT ( 'NONE',  ( 6.354454053420413473, 35.54304081427980577, 11.00000000000000000 ) ) ;
#29951 = CARTESIAN_POINT ( 'NONE',  ( 14.91782843052409646, 20.93207305098514581, 7.000000000000000000 ) ) ;
#29952 = ORIENTED_EDGE ( 'NONE', *, *, #10345, .F. ) ;
#29953 = CARTESIAN_POINT ( 'NONE',  ( -20.02047420364571906, 5.006101022618450358, -27.65113345958681634 ) ) ;
#29954 = CARTESIAN_POINT ( 'NONE',  ( -13.46929972531958697, 26.35070966310183138, 7.499999999999993783 ) ) ;
#29955 = CARTESIAN_POINT ( 'NONE',  ( 14.48927117870123027, -30.61587158504688233, 23.00000000000000000 ) ) ;
#29956 = CARTESIAN_POINT ( 'NONE',  ( 16.65204975395604237, -15.35049418271700006, -23.13297094094993511 ) ) ;
#29957 = DIRECTION ( 'NONE',  ( -0.9510565162951543083, -0.3090169943749450088, 0.000000000000000000 ) ) ;
#29958 = DIRECTION ( 'NONE',  ( -0.000000000000000000, -0.000000000000000000, -1.000000000000000000 ) ) ;
#29959 = CARTESIAN_POINT ( 'NONE',  ( 10.75708226969095627, 17.60808951942069456, -28.06054662593295390 ) ) ;
#29960 = CARTESIAN_POINT ( 'NONE',  ( -10.24066009500599250, -26.58087177409006330, 14.53008259255018153 ) ) ;
#29961 = ORIENTED_EDGE ( 'NONE', *, *, #15471, .F. ) ;
#29962 = AXIS2_PLACEMENT_3D ( 'NONE', #34697, #6459, #19250 ) ;
#29963 = CARTESIAN_POINT ( 'NONE',  ( -14.32137131676681463, 17.27576680070661297, -20.87916438781902073 ) ) ;
#29964 = CARTESIAN_POINT ( 'NONE',  ( -25.52323811238533224, -15.66556294379314451, 20.82122704794065271 ) ) ;
#29965 = DIRECTION ( 'NONE',  ( 0.000000000000000000, 0.000000000000000000, 1.000000000000000000 ) ) ;
#29966 = CARTESIAN_POINT ( 'NONE',  ( 15.42861054628522233, 26.73803055450190058, -5.474192869590372545 ) ) ;
#29967 = EDGE_LOOP ( 'NONE', ( #16251, #15123, #32658, #4534, #34525, #16450 ) ) ;
#29968 = CARTESIAN_POINT ( 'NONE',  ( -14.75621568350166513, 21.89813303538607059, 10.49999999999999822 ) ) ;
#29969 = ORIENTED_EDGE ( 'NONE', *, *, #7509, .T. ) ;
#29971 = CARTESIAN_POINT ( 'NONE',  ( -12.30736835487442882, 14.81698729810789672, 9.500000000000000000 ) ) ;
#29970 = CARTESIAN_POINT ( 'NONE',  ( -14.87240269245140567, 25.99712635132547689, -9.698082481812916100 ) ) ;
#29972 = CARTESIAN_POINT ( 'NONE',  ( -10.84979689475692766, -19.98760476204195058, -21.61563630248454615 ) ) ;
#29973 = ADVANCED_FACE ( 'NONE', ( #37299 ), #31202, .T. ) ;
#29974 = CARTESIAN_POINT ( 'NONE',  ( -31.38526299860026825, -24.75545609243354406, 11.55979286843934872 ) ) ;
#29975 = CARTESIAN_POINT ( 'NONE',  ( -27.33604612326909233, -15.39033642126372037, -14.72902412931908067 ) ) ;
#29976 = CARTESIAN_POINT ( 'NONE',  ( -9.295420884976664411, -25.43675055676933638, -5.476495350188955946 ) ) ;
#29977 = CARTESIAN_POINT ( 'NONE',  ( -9.788946493797832105, 21.72623886970244911, 12.00000000000000000 ) ) ;
#29978 = CARTESIAN_POINT ( 'NONE',  ( 11.99148969583736246, 17.49118954514694124, -25.10245485184838898 ) ) ;
#29980 = EDGE_CURVE ( 'NONE', #22931, #36670, #21264, .T. ) ;
#29979 = ORIENTED_EDGE ( 'NONE', *, *, #22458, .F. ) ;
#29981 = CARTESIAN_POINT ( 'NONE',  ( 22.20949710084497397, 6.145177408896746130, -17.88822456531065441 ) ) ;
#29982 = DIRECTION ( 'NONE',  ( 0.000000000000000000, 0.000000000000000000, 1.000000000000000000 ) ) ;
#29983 = AXIS2_PLACEMENT_3D ( 'NONE', #26838, #8359, #17515 ) ;
#29984 = EDGE_CURVE ( 'NONE', #35419, #37631, #16774, .T. ) ;
#29985 = CARTESIAN_POINT ( 'NONE',  ( 8.842822184360947801, 12.23747979796203289, 22.99999999999999289 ) ) ;
#29986 = CARTESIAN_POINT ( 'NONE',  ( 12.39463915635820612, 18.33192650902018883, 12.00000000000000000 ) ) ;
#29987 = ORIENTED_EDGE ( 'NONE', *, *, #32271, .F. ) ;
#29988 = CARTESIAN_POINT ( 'NONE',  ( -28.54615080091948087, -0.9312913580789032864, -13.39927911465294841 ) ) ;
#29989 = CARTESIAN_POINT ( 'NONE',  ( 24.58697627075426695, 0.3755645577039563032, -18.44458219269206722 ) ) ;
#29990 = EDGE_CURVE ( 'NONE', #23748, #9924, #16164, .T. ) ;
#29991 = VECTOR ( 'NONE', #35028, 1000.000000000000000 ) ;
#29992 = DIRECTION ( 'NONE',  ( 0.000000000000000000, 0.000000000000000000, 1.000000000000000000 ) ) ;
#29993 = CARTESIAN_POINT ( 'NONE',  ( 20.02374874442605091, -18.66705478562347764, 20.82122704794080192 ) ) ;
#29994 = CARTESIAN_POINT ( 'NONE',  ( 1.981960960816328887, 14.62372257652092422, 13.00000000000000178 ) ) ;
#29995 = PRESENTATION_STYLE_ASSIGNMENT (( #5212 ) ) ;
#29996 = FACE_OUTER_BOUND ( 'NONE', #19176, .T. ) ;
#29997 = CIRCLE ( 'NONE', #19599, 0.5000000000000004441 ) ;
#29998 = EDGE_LOOP ( 'NONE', ( #25870, #8667, #20031, #36387 ) ) ;
#29999 = EDGE_CURVE ( 'NONE', #17070, #29633, #19403, .T. ) ;
#30000 = DIRECTION ( 'NONE',  ( 0.4999999999999920064, -0.8660254037844432595, 0.000000000000000000 ) ) ;
#30001 = ADVANCED_FACE ( 'NONE', ( #22244 ), #19607, .F. ) ;
#30002 = ADVANCED_FACE ( 'NONE', ( #29353 ), #1327, .F. ) ;
#30003 = DIRECTION ( 'NONE',  ( 0.000000000000000000, 0.000000000000000000, 1.000000000000000000 ) ) ;
#30004 = FACE_OUTER_BOUND ( 'NONE', #14598, .T. ) ;
#30005 = CARTESIAN_POINT ( 'NONE',  ( 0.4029506027351301145, 37.46258620939589434, -8.404766914894960195 ) ) ;
#30006 = DIRECTION ( 'NONE',  ( 1.000000000000000000, 0.000000000000000000, 0.000000000000000000 ) ) ;
#30007 = LINE ( 'NONE', #21067, #25345 ) ;
#30008 = AXIS2_PLACEMENT_3D ( 'NONE', #14853, #40019, #12001 ) ;
#30009 = CARTESIAN_POINT ( 'NONE',  ( 16.99999999999999645, 22.50000000000000711, 11.00000000000000178 ) ) ;
#30010 = CARTESIAN_POINT ( 'NONE',  ( 8.633502029282041690, 11.46765470489692795, 7.499999999999999112 ) ) ;
#30011 = CARTESIAN_POINT ( 'NONE',  ( 10.16520467992603294, 20.33931832809677331, 12.00000000000000000 ) ) ;
#30012 = CARTESIAN_POINT ( 'NONE',  ( 9.762440214476880485, -29.39637225273894572, 22.99999999999999645 ) ) ;
#30013 = CARTESIAN_POINT ( 'NONE',  ( 14.58186407764969061, 28.53296701108370925, -7.305968526827398613 ) ) ;
#30014 = DIRECTION ( 'NONE',  ( 1.000000000000000000, 0.000000000000000000, 0.000000000000000000 ) ) ;
#30015 = EDGE_LOOP ( 'NONE', ( #17030, #21890, #6122 ) ) ;
#30016 = CIRCLE ( 'NONE', #15744, 0.4999999999999997780 ) ;
#30018 = DIRECTION ( 'NONE',  ( 1.000000000000000000, 0.000000000000000000, 0.000000000000000000 ) ) ;
#30017 = CARTESIAN_POINT ( 'NONE',  ( -19.19098252355692580, 16.63498700241322936, -5.962789986923132446 ) ) ;
#30019 = CARTESIAN_POINT ( 'NONE',  ( -13.72527515842276280, 27.95206079998173365, 10.49999999999999822 ) ) ;
#30020 = CARTESIAN_POINT ( 'NONE',  ( 14.65398229857985157, -25.46724026263229135, -10.65132889757489032 ) ) ;
#30021 = B_SPLINE_CURVE_WITH_KNOTS ( 'NONE', 3,
 ( #37488, #34245, #34047, #9064 ),
 .UNSPECIFIED., .F., .F.,
 ( 4, 4 ),
 ( 0.000000000000000000, 1.000000000000000000 ),
 .UNSPECIFIED. ) ;
#30022 = CARTESIAN_POINT ( 'NONE',  ( -3.610593701936590350, 31.83882289796395426, 10.50000000000000533 ) ) ;
#30023 = CARTESIAN_POINT ( 'NONE',  ( 12.91822118044063394, 21.66998749496536902, -17.43529018280291254 ) ) ;
#30024 = CARTESIAN_POINT ( 'NONE',  ( 3.091399026088761826, 22.35909668862748489, -30.00000000000000711 ) ) ;
#30025 = CARTESIAN_POINT ( 'NONE',  ( 39.51968006260096189, -13.07391885151743338, 11.00000000000000000 ) ) ;
#30026 = ADVANCED_FACE ( 'NONE', ( #26099 ), #19926, .T. ) ;
#30027 = CARTESIAN_POINT ( 'NONE',  ( -26.78191558544384776, -21.01471732344365151, -12.00199842359465130 ) ) ;
#30028 = VECTOR ( 'NONE', #30521, 999.9999999999998863 ) ;
#30029 = CARTESIAN_POINT ( 'NONE',  ( 1.745246714805118726, -24.23261900456495965, -10.38794052831897829 ) ) ;
#30030 = CARTESIAN_POINT ( 'NONE',  ( 15.21143254768586495, 25.78252244675921290, -8.771152263473718236 ) ) ;
#30031 = EDGE_CURVE ( 'NONE', #3751, #24567, #9200, .T. ) ;
#30032 = CARTESIAN_POINT ( 'NONE',  ( 21.25194171196830339, 11.83548972908152841, -9.890527645891060260 ) ) ;
#30033 = DIRECTION ( 'NONE',  ( 0.7431448254773954654, 0.6691306063588570163, 0.000000000000000000 ) ) ;
#30034 = ORIENTED_EDGE ( 'NONE', *, *, #2619, .T. ) ;
#30035 = CARTESIAN_POINT ( 'NONE',  ( -7.357442437755574716, 36.13703667136246622, -7.577783863828958744 ) ) ;
#30036 = ORIENTED_EDGE ( 'NONE', *, *, #20302, .F. ) ;
#30037 = AXIS2_PLACEMENT_3D ( 'NONE', #1431, #39204, #13813 ) ;
#30038 = CARTESIAN_POINT ( 'NONE',  ( -27.91036560783436471, 4.231346453976238209, 15.13084544680909005 ) ) ;
#30039 = EDGE_LOOP ( 'NONE', ( #1647, #34665 ) ) ;
#30040 = CARTESIAN_POINT ( 'NONE',  ( -1.981967702234832984, 30.37627742347970283, 6.000000000000000000 ) ) ;
#30041 = CIRCLE ( 'NONE', #33953, 1.000000000000004441 ) ;
#30042 = CARTESIAN_POINT ( 'NONE',  ( -1.229437847141422901, 24.50739181907689712, 13.00000000000000178 ) ) ;
#30043 = ORIENTED_EDGE ( 'NONE', *, *, #33211, .F. ) ;
#30044 = CARTESIAN_POINT ( 'NONE',  ( -20.47417334391911936, 1.028570030172704763, -29.35142929161455072 ) ) ;
#30045 = ORIENTED_EDGE ( 'NONE', *, *, #29605, .F. ) ;
#30046 = CARTESIAN_POINT ( 'NONE',  ( 20.19203522719319466, -6.104531446830016250, -26.36559112601934984 ) ) ;
#30047 = ORIENTED_EDGE ( 'NONE', *, *, #29984, .T. ) ;
#30048 = DIRECTION ( 'NONE',  ( 0.5877852522924696954, -0.8090169943749500048, 0.000000000000000000 ) ) ;
#30049 = ORIENTED_EDGE ( 'NONE', *, *, #7887, .T. ) ;
#30050 = CARTESIAN_POINT ( 'NONE',  ( 14.97009266215792778, 21.42933399866928568, 10.49999999999999822 ) ) ;
#30051 = FACE_OUTER_BOUND ( 'NONE', #18591, .T. ) ;
#30052 = AXIS2_PLACEMENT_3D ( 'NONE', #24313, #27757, #39943 ) ;
#30053 = DIRECTION ( 'NONE',  ( 0.5877852522924690293, -0.8090169943749503378, 0.000000000000000000 ) ) ;
#30054 = ORIENTED_EDGE ( 'NONE', *, *, #9966, .F. ) ;
#30055 = AXIS2_PLACEMENT_3D ( 'NONE', #3363, #12701, #9069 ) ;
#30056 =( NAMED_UNIT ( * ) SI_UNIT ( $, .STERADIAN. ) SOLID_ANGLE_UNIT ( ) );
#30057 = DIRECTION ( 'NONE',  ( -0.000000000000000000, -0.000000000000000000, -1.000000000000000000 ) ) ;
#30058 = CARTESIAN_POINT ( 'NONE',  ( -14.47283171447380390, 21.48159823030330884, 11.00000000000000000 ) ) ;
#30059 = VECTOR ( 'NONE', #11859, 1000.000000000000227 ) ;
#30060 = DIRECTION ( 'NONE',  ( -0.8660254037844431485, -0.4999999999999921174, 0.000000000000000000 ) ) ;
#30061 = CARTESIAN_POINT ( 'NONE',  ( 18.97955609020411316, 16.84654830053328567, -7.414115074451304466 ) ) ;
#30062 = CARTESIAN_POINT ( 'NONE',  ( 11.98184379570800218, 31.25359194820647701, -9.457391703318352327 ) ) ;
#30063 = VERTEX_POINT ( 'NONE', #23056 ) ;
#30064 = CARTESIAN_POINT ( 'NONE',  ( -22.38085876145960640, 10.82216326969894737, -5.482735768144592292 ) ) ;
#30065 = CARTESIAN_POINT ( 'NONE',  ( 10.77256156952748256, 32.87247436945319379, 10.76099332938163933 ) ) ;
#30066 = DIRECTION ( 'NONE',  ( 0.000000000000000000, 0.000000000000000000, 1.000000000000000000 ) ) ;
#30067 =( GEOMETRIC_REPRESENTATION_CONTEXT ( 3 ) GLOBAL_UNCERTAINTY_ASSIGNED_CONTEXT ( ( #24034 ) ) GLOBAL_UNIT_ASSIGNED_CONTEXT ( ( #14816, #40032, #16665 ) ) REPRESENTATION_CONTEXT ( 'NONE', 'WORKASPACE' ) );
#30068 = B_SPLINE_CURVE_WITH_KNOTS ( 'NONE', 3,
 ( #14588, #2600, #12136, #39761, #15183, #5442, #30025, #21280, #8891, #17653, #33691, #8693, #14986, #8287, #5241, #2201, #24126, #24524 ),
 .UNSPECIFIED., .F., .F.,
 ( 4, 2, 2, 2, 2, 2, 2, 2, 4 ),
 ( 0.000000000000000000, 0.1250000000000000000, 0.2500000000000000000, 0.3750000000000000000, 0.5000000000000000000, 0.6250000000000000000, 0.7500000000000000000, 0.8750000000000000000, 1.000000000000000000 ),
 .UNSPECIFIED. ) ;
#30069 = CARTESIAN_POINT ( 'NONE',  ( 13.06227854178500181, -22.56613844598916430, -16.39924439641581699 ) ) ;
#30070 = DIRECTION ( 'NONE',  ( 1.000000000000000000, 0.000000000000000000, 0.000000000000000000 ) ) ;
#30071 = CARTESIAN_POINT ( 'NONE',  ( -9.080802685385670259, 10.85199816882132673, 10.94611345180490503 ) ) ;
#30072 = CARTESIAN_POINT ( 'NONE',  ( -14.84019340197460934, 25.60882683859346187, -10.18024224215897178 ) ) ;
#30073 = VECTOR ( 'NONE', #31099, 1000.000000000000000 ) ;
#30074 = CARTESIAN_POINT ( 'NONE',  ( 8.893966021365395491, -18.47319264949478779, -29.36029315992060873 ) ) ;
#30075 = CARTESIAN_POINT ( 'NONE',  ( 11.54426418658508879, 32.09594396785328740, 10.49999999999999822 ) ) ;
#30076 = ORIENTED_EDGE ( 'NONE', *, *, #3219, .F. ) ;
#30077 = ORIENTED_EDGE ( 'NONE', *, *, #10108, .T. ) ;
#30078 = CARTESIAN_POINT ( 'NONE',  ( -7.473191970175785848, 20.37911561391303650, -24.56105570974891705 ) ) ;
#30079 = FACE_OUTER_BOUND ( 'NONE', #9393, .T. ) ;
#30080 = DIRECTION ( 'NONE',  ( -0.9135454576426059736, -0.4067366430757888285, 0.000000000000000000 ) ) ;
#30081 = VECTOR ( 'NONE', #23657, 1000.000000000000000 ) ;
#30082 = LINE ( 'NONE', #5098, #11799 ) ;
#30083 = VERTEX_POINT ( 'NONE', #10065 ) ;
#30084 = CARTESIAN_POINT ( 'NONE',  ( 30.12592084412306548, 0.07472801878552456922, -8.768476169707916767 ) ) ;
#30085 = CARTESIAN_POINT ( 'NONE',  ( 4.835130509701799362, 15.55077355964573904, 6.000000000000000000 ) ) ;
#30086 = PLANE ( 'NONE',  #9013 ) ;
#30087 = CARTESIAN_POINT ( 'NONE',  ( -19.48557158514982390, 33.75000000000009948, 7.000000000000000000 ) ) ;
#30088 = ORIENTED_EDGE ( 'NONE', *, *, #16972, .T. ) ;
#30089 = CARTESIAN_POINT ( 'NONE',  ( -23.92885585469906573, 0.5139776474599682121, -19.49970526494919554 ) ) ;
#30090 = DIRECTION ( 'NONE',  ( 0.5906904945688790098, 0.000000000000000000, 0.8068982213550685012 ) ) ;
#30091 = ORIENTED_EDGE ( 'NONE', *, *, #26900, .F. ) ;
#30092 = CARTESIAN_POINT ( 'NONE',  ( 20.78038650074347160, -2.939622687103573551, -26.54821385022073343 ) ) ;
#30093 = AXIS2_PLACEMENT_3D ( 'NONE', #1582, #4220, #23715 ) ;
#30094 = CARTESIAN_POINT ( 'NONE',  ( 16.92376161250197697, -28.83147800495239466, 13.32518128616474939 ) ) ;
#30095 = EDGE_LOOP ( 'NONE', ( #24439, #5581, #23643, #1708 ) ) ;
#30096 = CARTESIAN_POINT ( 'NONE',  ( -12.06278152636159007, 35.25200209733603174, 13.92931973827870706 ) ) ;
#30097 = CARTESIAN_POINT ( 'NONE',  ( 12.01634099004108513, -16.14815750340189027, 20.94377226548372661 ) ) ;
#30098 = CARTESIAN_POINT ( 'NONE',  ( 14.98890121934609532, -28.67928442654220333, 11.00000000000000000 ) ) ;
#30099 = B_SPLINE_CURVE_WITH_KNOTS ( 'NONE', 3,
 ( #18795, #6194, #12687, #2953, #12295, #15545, #37868, #30790 ),
 .UNSPECIFIED., .F., .F.,
 ( 4, 2, 2, 4 ),
 ( 0.000000000000000000, 0.0002364868538934310324, 0.0004729737077868620648, 0.0009459474155737337790 ),
 .UNSPECIFIED. ) ;
#30100 = CARTESIAN_POINT ( 'NONE',  ( 6.949287954459814287, 25.26733242291902926, 20.82122704794137746 ) ) ;
#30101 = VECTOR ( 'NONE', #9909, 1000.000000000000000 ) ;
#30102 = CARTESIAN_POINT ( 'NONE',  ( 5.237540274239913529, 35.49300472853430222, 9.500000000000000000 ) ) ;
#30103 = VERTEX_POINT ( 'NONE', #31799 ) ;
#30104 = EDGE_CURVE ( 'NONE', #39958, #14016, #4574, .T. ) ;
#30105 = CARTESIAN_POINT ( 'NONE',  ( 11.87435565298210882, 15.06698729810772619, 7.499999999999997335 ) ) ;
#30106 = PLANE ( 'NONE',  #33169 ) ;
#30107 = CARTESIAN_POINT ( 'NONE',  ( 5.670256885233474264, 29.09287741234969715, -15.76086933226568476 ) ) ;
#30108 = PLANE ( 'NONE',  #26891 ) ;
#30109 = VECTOR ( 'NONE', #39746, 1000.000000000000000 ) ;
#30110 = EDGE_CURVE ( 'NONE', #16796, #5069, #32286, .T. ) ;
#30111 = CARTESIAN_POINT ( 'NONE',  ( 19.99288511728601136, -2.332377806213334015, 20.94377226548710524 ) ) ;
#30112 = EDGE_CURVE ( 'NONE', #39108, #29636, #724, .T. ) ;
#30113 = CARTESIAN_POINT ( 'NONE',  ( 16.95921849111858748, -23.60331070195671188, -14.18631301038341697 ) ) ;
#30114 = CARTESIAN_POINT ( 'NONE',  ( -1.947644445291298432, 40.50000000000004974, 11.00000000000000000 ) ) ;
#30115 = CARTESIAN_POINT ( 'NONE',  ( -14.44277748876678302, 26.55045409923029354, 7.000000000000000000 ) ) ;
#30116 = CARTESIAN_POINT ( 'NONE',  ( 2.623829155769261678, 7.750987179267949223, 10.68306085400107008 ) ) ;
#30117 = EDGE_LOOP ( 'NONE', ( #14864, #35615, #14067 ) ) ;
#30118 = CARTESIAN_POINT ( 'NONE',  ( 14.88782195473658909, 25.94899730737486720, -9.700714136109681363 ) ) ;
#30119 = AXIS2_PLACEMENT_3D ( 'NONE', #12817, #13014, #37800 ) ;
#30120 = EDGE_LOOP ( 'NONE', ( #10742, #2149, #18063, #15090, #16143 ) ) ;
#30121 = CARTESIAN_POINT ( 'NONE',  ( -15.04061483196161753, 25.01295785739290167, -10.19153934133739270 ) ) ;
#30122 = CARTESIAN_POINT ( 'NONE',  ( -32.11924139737082129, -16.82817082614032955, 18.42518152272146637 ) ) ;
#30123 = FACE_OUTER_BOUND ( 'NONE', #31433, .T. ) ;
#30124 = CARTESIAN_POINT ( 'NONE',  ( 12.98912340479801131, 21.55496206960689420, -17.44778214844380315 ) ) ;
#30125 = EDGE_LOOP ( 'NONE', ( #14202, #26175, #20107, #2740 ) ) ;
#30126 = CARTESIAN_POINT ( 'NONE',  ( 17.65215317207318080, -10.44170805849464401, -29.21171622812354585 ) ) ;
#30127 = ORIENTED_EDGE ( 'NONE', *, *, #34556, .F. ) ;
#30129 = CARTESIAN_POINT ( 'NONE',  ( -19.26948696230206082, 27.85601271560033965, 23.00000000000000355 ) ) ;
#30128 = CARTESIAN_POINT ( 'NONE',  ( -12.68926805779758027, 22.04200062495521095, -17.38483120121016157 ) ) ;
#30130 = CARTESIAN_POINT ( 'NONE',  ( -17.61165795415892532, -26.24323257045744029, -9.577737097562327051 ) ) ;
#30131 = CARTESIAN_POINT ( 'NONE',  ( -6.023418944065157987, 39.81932404830322270, -4.999999999999988454 ) ) ;
#30132 = CIRCLE ( 'NONE', #37256, 1.000000000000000000 ) ;
#30133 = VERTEX_POINT ( 'NONE', #22849 ) ;
#30134 = CARTESIAN_POINT ( 'NONE',  ( -24.86735191267609224, -9.411377462502228397, -18.68429284230914078 ) ) ;
#30135 = CARTESIAN_POINT ( 'NONE',  ( -15.13531929286638977, -26.65245416579944759, -5.474118494994447026 ) ) ;
#30136 = CARTESIAN_POINT ( 'NONE',  ( 24.22138565352641493, -9.557272464391596500, 23.00000000000000000 ) ) ;
#30137 = ORIENTED_EDGE ( 'NONE', *, *, #5658, .F. ) ;
#30138 = CARTESIAN_POINT ( 'NONE',  ( 28.62947963101195725, 2.007663261502573793, -7.844485846290086606 ) ) ;
#30139 = DIRECTION ( 'NONE',  ( -0.6847716512521441201, 0.4446959099295496043, 0.5773502691896332806 ) ) ;
#30140 = ADVANCED_FACE ( 'NONE', ( #31594 ), #34853, .T. ) ;
#30141 = CARTESIAN_POINT ( 'NONE',  ( -38.66460482714639824, -17.32098561216439947, 22.99999999999999289 ) ) ;
#30142 = ADVANCED_FACE ( 'NONE', ( #25304 ), #37698, .T. ) ;
#30143 = ORIENTED_EDGE ( 'NONE', *, *, #36804, .F. ) ;
#30144 = CARTESIAN_POINT ( 'NONE',  ( -22.75019642290121880, 0.5465434661334764854, -21.60863951403461414 ) ) ;
#30145 = ORIENTED_EDGE ( 'NONE', *, *, #36685, .F. ) ;
#30146 = CARTESIAN_POINT ( 'NONE',  ( 30.60780290727160136, -0.8964730165270395901, -9.647732689552546148 ) ) ;
#30147 = CARTESIAN_POINT ( 'NONE',  ( 31.26284659378134734, -14.97710070420450279, 19.27171037444157520 ) ) ;
#30148 = ORIENTED_EDGE ( 'NONE', *, *, #16239, .T. ) ;
#30149 = CARTESIAN_POINT ( 'NONE',  ( -27.66981915501925826, 3.518264008085504990, -5.000000000000000888 ) ) ;
#30150 = DIRECTION ( 'NONE',  ( -0.9945218953682744001, -0.1045284632676437842, 0.000000000000000000 ) ) ;
#30151 = AXIS2_PLACEMENT_3D ( 'NONE', #18281, #9130, #33533 ) ;
#30152 = LINE ( 'NONE', #20209, #519 ) ;
#30153 = DIRECTION ( 'NONE',  ( 0.000000000000000000, 0.000000000000000000, 1.000000000000000000 ) ) ;
#30154 = DIRECTION ( 'NONE',  ( -0.000000000000000000, 0.000000000000000000, 1.000000000000000000 ) ) ;
#30155 = VECTOR ( 'NONE', #14972, 1000.000000000000000 ) ;
#30156 = ADVANCED_FACE ( 'NONE', ( #38091 ), #2810, .T. ) ;
#30157 = CIRCLE ( 'NONE', #23009, 0.4999999999999995559 ) ;
#30158 = CARTESIAN_POINT ( 'NONE',  ( -15.64741614794215252, 37.44040872933206288, 7.500000000000004441 ) ) ;
#30159 = CARTESIAN_POINT ( 'NONE',  ( 16.99999999999999645, 22.50000000000000711, 13.00000000000000178 ) ) ;
#30160 = ORIENTED_EDGE ( 'NONE', *, *, #23125, .T. ) ;
#30161 = CARTESIAN_POINT ( 'NONE',  ( -23.05888776652749428, 5.977869874196464650, -15.81723421387264139 ) ) ;
#30162 = CARTESIAN_POINT ( 'NONE',  ( 0.000000000000000000, 22.50000000000000355, 7.000000000000000000 ) ) ;
#30163 = DIRECTION ( 'NONE',  ( 0.000000000000000000, -0.6037757019622743693, -0.7971542521494587863 ) ) ;
#30164 = CARTESIAN_POINT ( 'NONE',  ( 25.90091635383566526, -25.33841663918061116, -7.598904778598901899 ) ) ;
#30165 = LINE ( 'NONE', #29558, #14500 ) ;
#30166 = CARTESIAN_POINT ( 'NONE',  ( 6.953805871968278929, 30.22298757065274444, 13.00000000000000178 ) ) ;
#30167 = CARTESIAN_POINT ( 'NONE',  ( 10.84377413474652307, 17.80538317806753668, -26.80397311259553206 ) ) ;
#30168 = CARTESIAN_POINT ( 'NONE',  ( -15.27443809245026785, -27.57253143578022048, 15.13084544680213561 ) ) ;
#30169 = ORIENTED_EDGE ( 'NONE', *, *, #9621, .F. ) ;
#30170 = CARTESIAN_POINT ( 'NONE',  ( -13.37529537539570867, 15.55228444284129097, -30.00000000000000711 ) ) ;
#30171 = CARTESIAN_POINT ( 'NONE',  ( -26.96432039561874205, -11.11241571815037865, 20.82122704794107548 ) ) ;
#30172 = DIRECTION ( 'NONE',  ( -0.6123724356957963577, -0.3535533905932721210, -0.7071067811865466846 ) ) ;
#30173 = CARTESIAN_POINT ( 'NONE',  ( 11.02706334812793720, 17.33462162532257977, -28.70783002534086847 ) ) ;
#30174 = EDGE_LOOP ( 'NONE', ( #35358, #8539, #24986, #25778 ) ) ;
#30175 = CARTESIAN_POINT ( 'NONE',  ( 8.505700342264139735, 22.10876900990906435, 7.000000000000000000 ) ) ;
#30176 = ORIENTED_EDGE ( 'NONE', *, *, #27545, .F. ) ;
#30178 = CARTESIAN_POINT ( 'NONE',  ( -3.503793317224517700, 8.420815634768727520, 7.499999999999997335 ) ) ;
#30177 = CARTESIAN_POINT ( 'NONE',  ( -15.05848678793640971, 26.27994695046478313, -8.761354843867154685 ) ) ;
#30179 = B_SPLINE_CURVE_WITH_KNOTS ( 'NONE', 3,
 ( #12586, #40010, #31278, #37372, #6284, #30684 ),
 .UNSPECIFIED., .F., .F.,
 ( 4, 2, 4 ),
 ( 0.000000000000000000, 0.5000000000000000000, 1.000000000000000000 ),
 .UNSPECIFIED. ) ;
#30180 = CARTESIAN_POINT ( 'NONE',  ( -15.06065773102657523, -26.00907756546740401, -9.234374514430680136 ) ) ;
#30181 = LINE ( 'NONE', #6184, #5615 ) ;
#30182 = CIRCLE ( 'NONE', #19793, 1.000000000000000000 ) ;
#30183 = CARTESIAN_POINT ( 'NONE',  ( -32.17239265530350423, -18.11259179091877414, -9.280970269152343022 ) ) ;
#30184 = CARTESIAN_POINT ( 'NONE',  ( -11.56078958348037844, -25.79303082475217224, -5.948641159686665070 ) ) ;
#30185 = CYLINDRICAL_SURFACE ( 'NONE', #9884, 21.00000000000002842 ) ;
#30186 = CARTESIAN_POINT ( 'NONE',  ( 11.83150832767071314, 16.74097710667822270, -29.36572269274261870 ) ) ;
#30187 = VERTEX_POINT ( 'NONE', #13102 ) ;
#30188 = CARTESIAN_POINT ( 'NONE',  ( 24.47864856487766261, 6.389536464586502262, -10.82169681586935539 ) ) ;
#30189 = CARTESIAN_POINT ( 'NONE',  ( 17.87719828188526705, -27.21529464712563495, -5.000000000000000000 ) ) ;
#30190 = CARTESIAN_POINT ( 'NONE',  ( 16.00000000000000000, 22.50000000000000355, 11.00000000000000178 ) ) ;
#30191 = ADVANCED_FACE ( 'NONE', ( #22645 ), #1128, .T. ) ;
#30192 = DIRECTION ( 'NONE',  ( 0.000000000000000000, 0.000000000000000000, 1.000000000000000000 ) ) ;
#30193 = VECTOR ( 'NONE', #17798, 1000.000000000000000 ) ;
#30194 = EDGE_LOOP ( 'NONE', ( #28405, #27315, #26623 ) ) ;
#30195 = CARTESIAN_POINT ( 'NONE',  ( -31.53032910951097989, -1.198340018515870575, -7.780284805138951043 ) ) ;
#30196 = CARTESIAN_POINT ( 'NONE',  ( 30.33251295709586159, -0.1458810018284433796, -8.758614351443290147 ) ) ;
#30197 = AXIS2_PLACEMENT_3D ( 'NONE', #11049, #10435, #32384 ) ;
#30198 = DIRECTION ( 'NONE',  ( 0.000000000000000000, 0.000000000000000000, -1.000000000000000000 ) ) ;
#30199 = CARTESIAN_POINT ( 'NONE',  ( 23.31304291943814277, -15.59395685184307290, 20.99999999999999645 ) ) ;
#30200 = DIRECTION ( 'NONE',  ( -0.4156269377774519103, 0.5720614028176885801, -0.7071067811865450192 ) ) ;
#30201 = CARTESIAN_POINT ( 'NONE',  ( 14.98890121934608288, -28.67928442654220333, 11.00000000000000000 ) ) ;
#30202 = ORIENTED_EDGE ( 'NONE', *, *, #10619, .T. ) ;
#30203 = CARTESIAN_POINT ( 'NONE',  ( -11.69134295108998245, 15.75000000000011191, 7.000000000000000000 ) ) ;
#30204 = EDGE_CURVE ( 'NONE', #3600, #257, #22250, .T. ) ;
#30205 = CARTESIAN_POINT ( 'NONE',  ( 8.339609403135803234, 11.87216320208440834, 7.000000000000000000 ) ) ;
#30206 = ORIENTED_EDGE ( 'NONE', *, *, #32515, .F. ) ;
#30207 = ADVANCED_FACE ( 'NONE', ( #17183 ), #26710, .T. ) ;
#30208 = CARTESIAN_POINT ( 'NONE',  ( 0.4067949480120627848, 37.90417743010413432, -7.544532716226419744 ) ) ;
#30209 = LINE ( 'NONE', #30612, #3611 ) ;
#30210 = CARTESIAN_POINT ( 'NONE',  ( 6.367390439426123372, 24.26983560722166544, 20.94377226548378701 ) ) ;
#30211 = EDGE_CURVE ( 'NONE', #26292, #4871, #38904, .T. ) ;
#30212 = CYLINDRICAL_SURFACE ( 'NONE', #35642, 1.000000000000000888 ) ;
#30213 = AXIS2_PLACEMENT_3D ( 'NONE', #10630, #26467, #35620 ) ;
#30214 = CARTESIAN_POINT ( 'NONE',  ( 8.118377661053324701, 10.47536095541698486, 7.500000000000000888 ) ) ;
#30215 = CARTESIAN_POINT ( 'NONE',  ( -2.605702774688126500, 27.44183462127829642, 6.000000000000000000 ) ) ;
#30216 = DIRECTION ( 'NONE',  ( 0.000000000000000000, 0.000000000000000000, 1.000000000000000000 ) ) ;
#30217 = CARTESIAN_POINT ( 'NONE',  ( 10.07128235380245052, 18.51023362060226063, -26.10639040881114781 ) ) ;
#30219 = VECTOR ( 'NONE', #10258, 1000.000000000000114 ) ;
#30218 = CARTESIAN_POINT ( 'NONE',  ( -7.353987181296344211, 35.57359447655193208, 7.000000000000000000 ) ) ;
#30220 = ORIENTED_EDGE ( 'NONE', *, *, #17240, .F. ) ;
#30221 = EDGE_CURVE ( 'NONE', #15652, #34128, #36539, .T. ) ;
#30224 = CARTESIAN_POINT ( 'NONE',  ( 12.83926296998457950, 26.67172942406175906, 7.000000000000000000 ) ) ;
#30223 = AXIS2_PLACEMENT_3D ( 'NONE', #36776, #33746, #17504 ) ;
#30222 = CARTESIAN_POINT ( 'NONE',  ( -18.38750743028887769, 15.73877471124131233, -12.84865677469772649 ) ) ;
#30225 = CARTESIAN_POINT ( 'NONE',  ( 0.5000000000000002220, 36.50000000000000711, 7.500000000000000888 ) ) ;
#30226 = CARTESIAN_POINT ( 'NONE',  ( 9.590584324842760466, -18.26333419585273887, -28.07628972030180492 ) ) ;
#30227 = CARTESIAN_POINT ( 'NONE',  ( 15.17329373222786337, 26.28549969035456613, -8.297710605404065021 ) ) ;
#30228 = CARTESIAN_POINT ( 'NONE',  ( 11.09996104015035279, 17.63036184699812381, -26.82805355210400933 ) ) ;
#30229 = ORIENTED_EDGE ( 'NONE', *, *, #13084, .T. ) ;
#30230 = FACE_OUTER_BOUND ( 'NONE', #4888, .T. ) ;
#30231 = DIRECTION ( 'NONE',  ( -0.3535533905932740084, -0.6123724356957886972, -0.7071067811865524577 ) ) ;
#30232 = CARTESIAN_POINT ( 'NONE',  ( -22.87698515175695846, -19.07680134495290503, -15.74116178021451518 ) ) ;
#30233 = CARTESIAN_POINT ( 'NONE',  ( 3.101033983210284450, -21.57712604886545193, -21.14822272720248009 ) ) ;
#30234 = CARTESIAN_POINT ( 'NONE',  ( 15.44951243528052487, 25.68331376365496865, -7.831890575027415480 ) ) ;
#30235 = CARTESIAN_POINT ( 'NONE',  ( 21.49425838908486952, 11.96617313177288011, -7.918919338291130927 ) ) ;
#30236 = CARTESIAN_POINT ( 'NONE',  ( -6.576253646258510166, 14.29921418520934040, 10.00000000000000000 ) ) ;
#30237 = CARTESIAN_POINT ( 'NONE',  ( -7.446792957322618811, 36.70800515527383823, -5.439754417765567673 ) ) ;
#30238 = EDGE_CURVE ( 'NONE', #7488, #18790, #8222, .T. ) ;
#30239 = ORIENTED_EDGE ( 'NONE', *, *, #38771, .T. ) ;
#30240 = ADVANCED_FACE ( 'NONE', ( #11280 ), #36267, .T. ) ;
#30241 = CARTESIAN_POINT ( 'NONE',  ( -17.01882136418544889, 27.23043334309702956, 13.32518128616608877 ) ) ;
#30242 = VERTEX_POINT ( 'NONE', #14319 ) ;
#30243 = FACE_OUTER_BOUND ( 'NONE', #33383, .T. ) ;
#30244 = CARTESIAN_POINT ( 'NONE',  ( -8.380596568873706076, 10.11444759148765549, 10.76099332938163577 ) ) ;
#30245 = AXIS2_PLACEMENT_3D ( 'NONE', #36771, #14836, #30877 ) ;
#30246 = CARTESIAN_POINT ( 'NONE',  ( -30.68739395818431959, 0.1797671858537337741, -5.474131994021600889 ) ) ;
#30247 = CARTESIAN_POINT ( 'NONE',  ( 32.68782978559330843, -10.89902263858124876, -11.12137701297516479 ) ) ;
#30248 = AXIS2_PLACEMENT_3D ( 'NONE', #32674, #26966, #24709 ) ;
#30249 = AXIS2_PLACEMENT_3D ( 'NONE', #15777, #24923, #33880 ) ;
#30250 = CIRCLE ( 'NONE', #38687, 1.000000000000000888 ) ;
#30251 = ORIENTED_EDGE ( 'NONE', *, *, #25596, .T. ) ;
#30252 = DIRECTION ( 'NONE',  ( 0.000000000000000000, 0.000000000000000000, -1.000000000000000000 ) ) ;
#30253 = ORIENTED_EDGE ( 'NONE', *, *, #2219, .T. ) ;
#30254 = DIRECTION ( 'NONE',  ( -0.5877852522924796874, -0.8090169943749426773, 0.000000000000000000 ) ) ;
#30255 = CARTESIAN_POINT ( 'NONE',  ( 2.140527761532493134, 7.619874298175136396, 10.49999999999999467 ) ) ;
#30256 = EDGE_CURVE ( 'NONE', #2610, #37186, #1510, .T. ) ;
#30257 = FACE_OUTER_BOUND ( 'NONE', #7896, .T. ) ;
#30258 = ORIENTED_EDGE ( 'NONE', *, *, #24188, .F. ) ;
#30259 = EDGE_CURVE ( 'NONE', #34344, #8098, #9310, .T. ) ;
#30260 =( NAMED_UNIT ( * ) PLANE_ANGLE_UNIT ( ) SI_UNIT ( $, .RADIAN. ) );
#30261 = DIRECTION ( 'NONE',  ( 0.9945218953682729568, -0.1045284632676569680, 0.000000000000000000 ) ) ;
#30262 = CARTESIAN_POINT ( 'NONE',  ( 0.000000000000000000, 22.50000000000000355, 6.000000000000000000 ) ) ;
#30263 = CARTESIAN_POINT ( 'NONE',  ( 2.518583951651050867, 7.712953814960687104, 7.499999999999990230 ) ) ;
#30264 = CARTESIAN_POINT ( 'NONE',  ( 20.56955126053106042, -16.81405870680252690, -18.68695065117257315 ) ) ;
#30265 = CARTESIAN_POINT ( 'NONE',  ( 18.34675927358811975, 14.71332062100892202, -14.88700802970827120 ) ) ;
#30266 = CARTESIAN_POINT ( 'NONE',  ( 12.25923078083974360, 32.08250591462850565, -7.667896807040970764 ) ) ;
#30267 = EDGE_LOOP ( 'NONE', ( #7657, #6101 ) ) ;
#30268 = EDGE_CURVE ( 'NONE', #2021, #37780, #8018, .T. ) ;
#30269 = CARTESIAN_POINT ( 'NONE',  ( -18.36874938498262466, 9.174293865845140061, -28.86133430165910951 ) ) ;
#30270 = PLANE ( 'NONE',  #39771 ) ;
#30271 = CARTESIAN_POINT ( 'NONE',  ( -14.79690083935193989, 20.03899165096060386, 7.382773698552470343 ) ) ;
#30272 = CARTESIAN_POINT ( 'NONE',  ( 14.51603474985190623, -24.68602004783254245, -12.51313738316805768 ) ) ;
#30273 = DIRECTION ( 'NONE',  ( -0.1045284632676436315, 0.9945218953682742891, 0.000000000000000000 ) ) ;
#30274 = CARTESIAN_POINT ( 'NONE',  ( -9.189613563248645534, 10.70223284378013062, 10.76099332938163577 ) ) ;
#30275 = CARTESIAN_POINT ( 'NONE',  ( -11.16442365856205932, 17.77074711030141785, -26.22272145734717697 ) ) ;
#30276 = VECTOR ( 'NONE', #39713, 1000.000000000000000 ) ;
#30277 = CARTESIAN_POINT ( 'NONE',  ( -15.88203534348982693, -18.94643611089546198, -19.99739510857416036 ) ) ;
#30278 = CARTESIAN_POINT ( 'NONE',  ( 9.207210607180677187, -19.50632804910366858, -23.97127578096531053 ) ) ;
#30279 = AXIS2_PLACEMENT_3D ( 'NONE', #24626, #36627, #12038 ) ;
#30280 = CARTESIAN_POINT ( 'NONE',  ( 11.56190694343555947, 31.61076883254013126, 10.49999999999999822 ) ) ;
#30281 = ORIENTED_EDGE ( 'NONE', *, *, #3071, .T. ) ;
#30282 = ORIENTED_EDGE ( 'NONE', *, *, #16486, .F. ) ;
#30283 = CARTESIAN_POINT ( 'NONE',  ( -12.49268588895353105, 31.85193245464213518, -7.673184180311376501 ) ) ;
#30284 = EDGE_CURVE ( 'NONE', #40053, #2398, #30165, .T. ) ;
#30285 = LINE ( 'NONE', #38819, #13304 ) ;
#30286 = LINE ( 'NONE', #2253, #10728 ) ;
#30287 = EDGE_CURVE ( 'NONE', #13580, #36183, #19016, .T. ) ;
#30288 = CARTESIAN_POINT ( 'NONE',  ( -9.426561227484903327, 11.13126706419782508, 10.49999999999999822 ) ) ;
#30289 = ORIENTED_EDGE ( 'NONE', *, *, #7760, .F. ) ;
#30290 = CARTESIAN_POINT ( 'NONE',  ( 27.68069398113840052, 0.2662808206736965722, -13.51781012861318843 ) ) ;
#30291 = LINE ( 'NONE', #35987, #25169 ) ;
#30292 = DIRECTION ( 'NONE',  ( 0.9135454576426048634, 0.4067366430757912710, 0.000000000000000000 ) ) ;
#30293 = ORIENTED_EDGE ( 'NONE', *, *, #23075, .T. ) ;
#30294 = CARTESIAN_POINT ( 'NONE',  ( -30.59254050256992841, 0.006261417149339938010, -7.357959963668824876 ) ) ;
#30295 = DIRECTION ( 'NONE',  ( 0.6123724356957959136, 0.3535533905932670140, 0.7071067811865496822 ) ) ;
#30296 = ORIENTED_EDGE ( 'NONE', *, *, #15922, .T. ) ;
#30297 = CARTESIAN_POINT ( 'NONE',  ( 20.48544130033148747, -2.888783638426572598, -27.89533876242412447 ) ) ;
#30298 = CARTESIAN_POINT ( 'NONE',  ( 35.19094867589885212, -3.640833979052563674, 13.92931973827808534 ) ) ;
#30299 = EDGE_LOOP ( 'NONE', ( #32573, #1882, #36557 ) ) ;
#30300 = CARTESIAN_POINT ( 'NONE',  ( 16.03057579644872988, 28.88256098452291454, 14.53008259254079881 ) ) ;
#30301 = CARTESIAN_POINT ( 'NONE',  ( -11.45923940081499559, -19.42154971137169639, 20.25080042701605976 ) ) ;
#30302 = CARTESIAN_POINT ( 'NONE',  ( 7.929471891321336230, 25.60217271033461373, 9.000000000000001776 ) ) ;
#30303 = CARTESIAN_POINT ( 'NONE',  ( -8.504221777570748486, 25.88639746736783565, 20.50957957746009797 ) ) ;
#30304 = AXIS2_PLACEMENT_3D ( 'NONE', #11504, #21241, #2366 ) ;
#30305 = AXIS2_PLACEMENT_3D ( 'NONE', #26581, #13781, #1198 ) ;
#30306 = CARTESIAN_POINT ( 'NONE',  ( 0.000000000000000000, 22.50000000000000355, 11.00000000000000178 ) ) ;
#30307 = EDGE_LOOP ( 'NONE', ( #12064, #26380 ) ) ;
#30308 = EDGE_CURVE ( 'NONE', #13430, #12503, #10582, .T. ) ;
#30309 = DIRECTION ( 'NONE',  ( -0.9510565162951503115, 0.3090169943749573878, -0.000000000000000000 ) ) ;
#30310 = DIRECTION ( 'NONE',  ( 0.9781476007338067991, 0.2079116908177533474, -0.000000000000000000 ) ) ;
#30311 = AXIS2_PLACEMENT_3D ( 'NONE', #6016, #6217, #21460 ) ;
#30312 = CARTESIAN_POINT ( 'NONE',  ( 4.305481116379047180, 22.27104015248967173, -23.09767284345425509 ) ) ;
#30313 = DIRECTION ( 'NONE',  ( 1.000000000000000000, 0.000000000000000000, 0.000000000000000000 ) ) ;
#30314 = CARTESIAN_POINT ( 'NONE',  ( 4.817371740575477013, 23.83900317890016751, 20.99999999999999645 ) ) ;
#30315 = CARTESIAN_POINT ( 'NONE',  ( 17.34618997557657849, -22.82648989626997604, -15.08118710441591048 ) ) ;
#30316 = DIRECTION ( 'NONE',  ( -0.000000000000000000, -0.000000000000000000, -1.000000000000000000 ) ) ;
#30317 = CARTESIAN_POINT ( 'NONE',  ( -9.665073660138977729, 25.11464168560200250, 10.00000000000000000 ) ) ;
#30318 = CARTESIAN_POINT ( 'NONE',  ( -4.794796183862964689, 36.71301971979259804, 7.000000000000000000 ) ) ;
#30319 = ORIENTED_EDGE ( 'NONE', *, *, #27745, .T. ) ;
#30320 = CARTESIAN_POINT ( 'NONE',  ( 15.15030103098511383, 26.36342365734200399, -8.294678768621148279 ) ) ;
#30321 = ORIENTED_EDGE ( 'NONE', *, *, #21849, .T. ) ;
#30322 = CARTESIAN_POINT ( 'NONE',  ( -11.51726355202159624, 17.19569276542222269, -27.48129831304505899 ) ) ;
#30323 = CARTESIAN_POINT ( 'NONE',  ( -24.79887074938341840, -23.91042127310561938, 18.42518152272108978 ) ) ;
#30324 = CARTESIAN_POINT ( 'NONE',  ( -3.513409677696690991, 8.375574215747771945, 10.99999999999999289 ) ) ;
#30325 = CARTESIAN_POINT ( 'NONE',  ( 12.71338354207696497, 20.96606222537368325, -18.46259050867353579 ) ) ;
#30326 = VERTEX_POINT ( 'NONE', #4977 ) ;
#30327 = CARTESIAN_POINT ( 'NONE',  ( 32.65952487167601248, -19.32530057143253543, -7.543753945995782750 ) ) ;
#30328 = VERTEX_POINT ( 'NONE', #10880 ) ;
#30330 = CARTESIAN_POINT ( 'NONE',  ( 7.899339922805233449, 10.02167583667219830, 10.49999999999999822 ) ) ;
#30329 = CARTESIAN_POINT ( 'NONE',  ( -15.06956279710928293, 27.24103417575508246, -7.338594085143288481 ) ) ;
#30331 = CARTESIAN_POINT ( 'NONE',  ( -12.01071536255492944, -19.67856823503798935, -21.46176309291517015 ) ) ;
#30332 = CARTESIAN_POINT ( 'NONE',  ( 13.63581098909226519, 27.45627467658428600, 11.00000000000000000 ) ) ;
#30333 = CIRCLE ( 'NONE', #22509, 0.5000000000000001110 ) ;
#30334 = VECTOR ( 'NONE', #13127, 1000.000000000000000 ) ;
#30335 = ORIENTED_EDGE ( 'NONE', *, *, #2345, .F. ) ;
#30336 = CARTESIAN_POINT ( 'NONE',  ( -19.38376532770186600, -6.700500133912340672, -30.00000000000000711 ) ) ;
#30337 = CARTESIAN_POINT ( 'NONE',  ( -12.02355362826419949, -22.03127078142710360, -17.46066762549815010 ) ) ;
#30338 = CARTESIAN_POINT ( 'NONE',  ( 29.22254794994939786, -28.85350742528249413, 11.00000000000000000 ) ) ;
#30339 = ORIENTED_EDGE ( 'NONE', *, *, #25728, .F. ) ;
#30340 = CARTESIAN_POINT ( 'NONE',  ( 21.01898744346075887, 2.370978427325546534, -25.17228136638972913 ) ) ;
#30341 = EDGE_CURVE ( 'NONE', #10782, #22765, #27113, .T. ) ;
#30342 = CARTESIAN_POINT ( 'NONE',  ( -8.087160441415543133, 9.969847506823033001, 10.49999999999999822 ) ) ;
#30343 = CARTESIAN_POINT ( 'NONE',  ( -35.72300736400902110, -23.12593624637910850, 11.00000000000000000 ) ) ;
#30344 = EDGE_CURVE ( 'NONE', #32472, #6988, #20335, .T. ) ;
#30345 = AXIS2_PLACEMENT_3D ( 'NONE', #21841, #36698, #117 ) ;
#30346 = ORIENTED_EDGE ( 'NONE', *, *, #15317, .F. ) ;
#30347 = CARTESIAN_POINT ( 'NONE',  ( -20.48527248842334458, 0.7769947089114559446, -30.00000000000000000 ) ) ;
#30348 = VERTEX_POINT ( 'NONE', #38703 ) ;
#30349 = CARTESIAN_POINT ( 'NONE',  ( 23.60161110719205269, -0.2824371959814870880, -20.42950721209147602 ) ) ;
#30350 = VECTOR ( 'NONE', #11106, 1000.000000000000227 ) ;
#30351 = CARTESIAN_POINT ( 'NONE',  ( 26.77946264071975691, -24.43926981373490648, 17.42190598798353207 ) ) ;
#30352 = ORIENTED_EDGE ( 'NONE', *, *, #16352, .T. ) ;
#30353 = CARTESIAN_POINT ( 'NONE',  ( -27.59133651858127578, 3.518468992289588648, -6.427306901501287584 ) ) ;
#30354 = EDGE_CURVE ( 'NONE', #31788, #8093, #14519, .T. ) ;
#30355 = LINE ( 'NONE', #9011, #22272 ) ;
#30356 = DIRECTION ( 'NONE',  ( -0.4067366430757889395, 0.9135454576426058626, 0.000000000000000000 ) ) ;
#30357 = CARTESIAN_POINT ( 'NONE',  ( -15.07283634910000814, -28.35394831540519789, 13.32518128616608699 ) ) ;
#30358 = DIRECTION ( 'NONE',  ( 0.000000000000000000, 0.000000000000000000, 1.000000000000000000 ) ) ;
#30359 = AXIS2_PLACEMENT_3D ( 'NONE', #12224, #33177, #37008 ) ;
#30360 = VECTOR ( 'NONE', #6883, 1000.000000000000000 ) ;
#30361 = AXIS2_PLACEMENT_3D ( 'NONE', #30394, #14345, #5203 ) ;
#30362 = FACE_BOUND ( 'NONE', #30858, .T. ) ;
#30363 = FACE_OUTER_BOUND ( 'NONE', #10304, .T. ) ;
#30364 = EDGE_LOOP ( 'NONE', ( #39584, #2685, #5483, #5953 ) ) ;
#30365 = CARTESIAN_POINT ( 'NONE',  ( -24.79570961235407012, 6.146241236260801877, -10.32277382243248454 ) ) ;
#30366 = DIRECTION ( 'NONE',  ( 1.000000000000000000, 0.000000000000000000, 0.000000000000000000 ) ) ;
#30367 = ADVANCED_FACE ( 'NONE', ( #20221 ), #19680, .T. ) ;
#30368 = CARTESIAN_POINT ( 'NONE',  ( -8.859192577249677569, 12.20922670551869516, 20.99999999999999645 ) ) ;
#30369 = CARTESIAN_POINT ( 'NONE',  ( 24.20444226731742177, -25.16656729849181673, -9.375567471260238150 ) ) ;
#30370 = CIRCLE ( 'NONE', #23229, 1.000000000000000888 ) ;
#30371 = DIRECTION ( 'NONE',  ( -1.000000000000000000, 0.000000000000000000, 0.000000000000000000 ) ) ;
#30372 = CARTESIAN_POINT ( 'NONE',  ( 15.17781109110005389, 26.90704365139002974, -7.347467770236907114 ) ) ;
#30373 = CARTESIAN_POINT ( 'NONE',  ( 10.13173764377233077, -27.22067640325132487, 12.73282698324872442 ) ) ;
#30374 = B_SPLINE_CURVE_WITH_KNOTS ( 'NONE', 3,
 ( #15713, #37055, #21608, #13255, #16723, #15917 ),
 .UNSPECIFIED., .F., .F.,
 ( 4, 2, 4 ),
 ( 0.3333333336416847703, 0.6666666668208423019, 1.000000000000000000 ),
 .UNSPECIFIED. ) ;
#30375 = ORIENTED_EDGE ( 'NONE', *, *, #17620, .T. ) ;
#30376 = CARTESIAN_POINT ( 'NONE',  ( -13.60555342264946432, 17.51225866673465248, -21.88651860859232201 ) ) ;
#30377 = CARTESIAN_POINT ( 'NONE',  ( -26.77583779507883932, -12.71777209950081655, 20.82122704794079837 ) ) ;
#30378 = DIRECTION ( 'NONE',  ( 1.000000000000000000, 0.000000000000000000, 0.000000000000000000 ) ) ;
#30379 = CARTESIAN_POINT ( 'NONE',  ( 11.20492248755046916, 17.74145648390907581, -26.22707998456911227 ) ) ;
#30380 = ORIENTED_EDGE ( 'NONE', *, *, #5773, .T. ) ;
#30381 = CARTESIAN_POINT ( 'NONE',  ( 13.48758456246939375, 22.82324740036658994, -15.44989232396194723 ) ) ;
#30382 = VERTEX_POINT ( 'NONE', #31295 ) ;
#30384 = PLANE ( 'NONE',  #12087 ) ;
#30383 = CARTESIAN_POINT ( 'NONE',  ( -15.24884605207680899, 26.67307980227703013, -7.353820275870864620 ) ) ;
#30385 = CARTESIAN_POINT ( 'NONE',  ( -9.583030972882045972, -18.26713118289615068, -28.07671138377387621 ) ) ;
#30386 = CARTESIAN_POINT ( 'NONE',  ( -12.05736835487443237, 14.38397459621567442, 7.000000000000000000 ) ) ;
#30387 = CARTESIAN_POINT ( 'NONE',  ( -18.22632359083961973, -10.26709115745145695, -26.96482044692446678 ) ) ;
#30388 = CARTESIAN_POINT ( 'NONE',  ( -13.67153465227740305, -25.94622658622995814, -8.309525041132507894 ) ) ;
#30389 = CYLINDRICAL_SURFACE ( 'NONE', #145, 1.000000000000000888 ) ;
#30390 = CARTESIAN_POINT ( 'NONE',  ( 15.89516500601641624, 24.02346326373800167, -8.316517264783472640 ) ) ;
#30391 = ORIENTED_EDGE ( 'NONE', *, *, #1712, .T. ) ;
#30392 = CARTESIAN_POINT ( 'NONE',  ( 21.45806756224683554, 6.896564397286524262, -18.96977795570283831 ) ) ;
#30393 = EDGE_CURVE ( 'NONE', #2857, #28430, #4053, .T. ) ;
#30394 = CARTESIAN_POINT ( 'NONE',  ( -0.9819677022348329842, 30.37627742347970283, 13.00000000000000178 ) ) ;
#30395 = CARTESIAN_POINT ( 'NONE',  ( -75.15099915297791711, 43.38844959084113384, 23.00000000000000000 ) ) ;
#30396 = DIRECTION ( 'NONE',  ( -0.000000000000000000, -0.000000000000000000, -1.000000000000000000 ) ) ;
#30397 = VERTEX_POINT ( 'NONE', #3859 ) ;
#30398 = CARTESIAN_POINT ( 'NONE',  ( -27.89312612946301684, -0.8754152598143283281, -14.35503880984175495 ) ) ;
#30399 = EDGE_CURVE ( 'NONE', #10635, #35497, #28041, .T. ) ;
#30401 = CARTESIAN_POINT ( 'NONE',  ( 25.94993652933962736, 0.1776616952070861344, -16.42543414208182639 ) ) ;
#30400 = AXIS2_PLACEMENT_3D ( 'NONE', #22479, #4403, #35286 ) ;
#30402 = CIRCLE ( 'NONE', #12855, 0.5000000000000004441 ) ;
#30403 = CARTESIAN_POINT ( 'NONE',  ( 5.034171952702011232, 35.03623199971301005, 9.500000000000000000 ) ) ;
#30404 = ADVANCED_FACE ( 'NONE', ( #19100 ), #218, .T. ) ;
#30405 = CARTESIAN_POINT ( 'NONE',  ( 28.38958307348582366, -9.126824876479627591, 20.50957957746028626 ) ) ;
#30406 = EDGE_CURVE ( 'NONE', #30744, #29890, #17770, .T. ) ;
#30407 = AXIS2_PLACEMENT_3D ( 'NONE', #15802, #27795, #37340 ) ;
#30408 = LINE ( 'NONE', #39733, #9263 ) ;
#30410 = AXIS2_PLACEMENT_3D ( 'NONE', #28378, #31234, #19043 ) ;
#30409 = CARTESIAN_POINT ( 'NONE',  ( 37.13148535761800417, -14.80270701502663044, 11.00000000000000000 ) ) ;
#30411 = VERTEX_POINT ( 'NONE', #12998 ) ;
#30412 = CYLINDRICAL_SURFACE ( 'NONE', #24269, 1.000000000000000888 ) ;
#30413 = CARTESIAN_POINT ( 'NONE',  ( 13.63581098909226874, 27.45627467658428955, 9.000000000000001776 ) ) ;
#30414 = CARTESIAN_POINT ( 'NONE',  ( -7.354454053420251824, 35.54304081427989814, 7.000000000000000000 ) ) ;
#30415 = CARTESIAN_POINT ( 'NONE',  ( 0.2743609694596454984, 25.73594535306035525, -19.62891333975765207 ) ) ;
#30416 = FACE_OUTER_BOUND ( 'NONE', #10278, .T. ) ;
#30417 = ADVANCED_FACE ( 'NONE', ( #15856 ), #34945, .F. ) ;
#30418 = DIRECTION ( 'NONE',  ( 0.9781476007338072431, 0.2079116908177519041, 0.000000000000000000 ) ) ;
#30419 = ADVANCED_FACE ( 'NONE', ( #19293 ), #34542, .F. ) ;
#30420 = CARTESIAN_POINT ( 'NONE',  ( -13.05736835487441994, 16.11602540378456183, 11.00000000000000000 ) ) ;
#30421 = CARTESIAN_POINT ( 'NONE',  ( 6.706335727061685681, 24.35410196624994583, 13.00000000000000178 ) ) ;
#30422 = CARTESIAN_POINT ( 'NONE',  ( -1.247473515615844075, 16.63111439559750693, 12.00000000000000000 ) ) ;
#30423 = DIRECTION ( 'NONE',  ( -0.000000000000000000, 0.000000000000000000, -1.000000000000000000 ) ) ;
#30424 = VECTOR ( 'NONE', #3430, 1000.000000000000000 ) ;
#30425 = CARTESIAN_POINT ( 'NONE',  ( 11.44973932604695754, 21.65318152733180668, -19.31446654788366502 ) ) ;
#30426 = LINE ( 'NONE', #18032, #28292 ) ;
#30427 = CIRCLE ( 'NONE', #12893, 1.000000000000000888 ) ;
#30428 = EDGE_LOOP ( 'NONE', ( #16812, #5901, #39825, #3863 ) ) ;
#30430 = DIRECTION ( 'NONE',  ( -0.9510565162951543083, -0.3090169943749450088, 0.000000000000000000 ) ) ;
#30429 = CARTESIAN_POINT ( 'NONE',  ( -15.91172688669051283, 12.94523012445180399, -29.42231075624701475 ) ) ;
#30431 = CARTESIAN_POINT ( 'NONE',  ( -14.00731263743711885, 27.57698287931463454, 10.82238861112334760 ) ) ;
#30432 = CARTESIAN_POINT ( 'NONE',  ( 10.24068639920821688, -19.15891185376089112, -23.85198230486452076 ) ) ;
#30433 = CARTESIAN_POINT ( 'NONE',  ( 32.28722999652337933, 1.315479119629256788, 12.14047268033097460 ) ) ;
#30434 = CARTESIAN_POINT ( 'NONE',  ( 14.72828018990482235, 25.42434042747754219, -10.65132935642424350 ) ) ;
#30435 = AXIS2_PLACEMENT_3D ( 'NONE', #12259, #22793, #29097 ) ;
#30436 = EDGE_LOOP ( 'NONE', ( #12266, #35791, #31178, #28321 ) ) ;
#30437 = DIRECTION ( 'NONE',  ( -0.7071067811865451302, -0.7071067811865499042, 1.559530880411979857E-16 ) ) ;
#30438 = DIRECTION ( 'NONE',  ( 0.3535533905932750631, -0.6123724356958023529, -0.7071067811865401342 ) ) ;
#30439 = CARTESIAN_POINT ( 'NONE',  ( -19.60827666070207087, -16.31332699639156303, -19.71403864979324538 ) ) ;
#30440 = CARTESIAN_POINT ( 'NONE',  ( 1.243865831159307822, -20.57034976483239319, -28.30086564174369457 ) ) ;
#30441 = CARTESIAN_POINT ( 'NONE',  ( 11.24974104459727009, 17.28524465445085667, -28.08974055294966732 ) ) ;
#30442 = CARTESIAN_POINT ( 'NONE',  ( 18.33234679620570873, 10.26058583535126267, -24.41653352660923204 ) ) ;
#30443 = CARTESIAN_POINT ( 'NONE',  ( -17.34253826607186966, 27.32041144404027122, -5.000000000000000000 ) ) ;
#30444 = CARTESIAN_POINT ( 'NONE',  ( -3.989573575045165743, 23.25966083313679889, -21.92851973090041184 ) ) ;
#30445 = ORIENTED_EDGE ( 'NONE', *, *, #27220, .T. ) ;
#30446 = EDGE_CURVE ( 'NONE', #32040, #6084, #37833, .T. ) ;
#30447 = CARTESIAN_POINT ( 'NONE',  ( -23.13582672293654596, 13.35747578641134048, 12.14047268033097282 ) ) ;
#30448 = ORIENTED_EDGE ( 'NONE', *, *, #15825, .T. ) ;
#30449 = DIRECTION ( 'NONE',  ( 0.1045284632676436315, -0.9945218953682742891, 0.000000000000000000 ) ) ;
#30450 = CYLINDRICAL_SURFACE ( 'NONE', #34276, 1.000000000000000000 ) ;
#30451 = CARTESIAN_POINT ( 'NONE',  ( -30.51074951646900857, 0.1921439302265571525, -6.888518465258303358 ) ) ;
#30452 = ADVANCED_FACE ( 'NONE', ( #9957 ), #4105, .T. ) ;
#30453 = CARTESIAN_POINT ( 'NONE',  ( 35.15679305665209142, -10.61876882962838486, -7.156232860489364356 ) ) ;
#30454 = CIRCLE ( 'NONE', #10986, 0.5000000000000004441 ) ;
#30455 = AXIS2_PLACEMENT_3D ( 'NONE', #9482, #30820, #9082 ) ;
#30456 = ORIENTED_EDGE ( 'NONE', *, *, #19932, .T. ) ;
#30457 = SHAPE_DEFINITION_REPRESENTATION ( #272, #28068 ) ;
#30458 = CARTESIAN_POINT ( 'NONE',  ( 0.000000000000000000, 22.50000000000000355, 11.00000000000000178 ) ) ;
#30459 = ORIENTED_EDGE ( 'NONE', *, *, #3542, .T. ) ;
#30460 = PLANE ( 'NONE',  #38502 ) ;
#30461 = CARTESIAN_POINT ( 'NONE',  ( -11.19134295108999311, 14.88397459621566554, 9.500000000000000000 ) ) ;
#30462 = DIRECTION ( 'NONE',  ( 0.000000000000000000, 0.000000000000000000, 1.000000000000000000 ) ) ;
#30463 = ORIENTED_EDGE ( 'NONE', *, *, #24459, .T. ) ;
#30464 = DIRECTION ( 'NONE',  ( 0.000000000000000000, 0.000000000000000000, 1.000000000000000000 ) ) ;
#30465 = CARTESIAN_POINT ( 'NONE',  ( -6.151085731882353969, 35.08626808545859888, 7.500000000000000888 ) ) ;
#30466 = DIRECTION ( 'NONE',  ( -0.9945218953682744001, -0.1045284632676437564, 0.000000000000000000 ) ) ;
#30467 = CARTESIAN_POINT ( 'NONE',  ( 16.64356867624101000, -11.98442300389733539, -29.21688973832524994 ) ) ;
#30468 = EDGE_CURVE ( 'NONE', #26406, #22335, #10160, .T. ) ;
#30469 = CARTESIAN_POINT ( 'NONE',  ( 19.25847470691681096, 15.64464181457198322, -9.379364711887674844 ) ) ;
#30470 = CARTESIAN_POINT ( 'NONE',  ( 6.931030674386980728, 19.37776282368324487, -28.55341591256747691 ) ) ;
#30471 = ORIENTED_EDGE ( 'NONE', *, *, #22084, .F. ) ;
#30472 = CARTESIAN_POINT ( 'NONE',  ( -20.09127696847111366, 8.941272172551848030, -20.10129515931187072 ) ) ;
#30473 = DIRECTION ( 'NONE',  ( 1.000000000000000000, 0.000000000000000000, 0.000000000000000000 ) ) ;
#30474 = CARTESIAN_POINT ( 'NONE',  ( -14.75241816305527642, 19.78287871224842220, 7.203056206335838318 ) ) ;
#30475 = CARTESIAN_POINT ( 'NONE',  ( 15.16669826860400150, -26.03282984618214968, -9.229254182688153563 ) ) ;
#30476 = DIRECTION ( 'NONE',  ( 1.000000000000000000, 0.000000000000000000, 0.000000000000000000 ) ) ;
#30477 = CARTESIAN_POINT ( 'NONE',  ( 33.62187204924162387, 0.04418559750794539415, -5.000000000000000000 ) ) ;
#30479 = AXIS2_PLACEMENT_3D ( 'NONE', #13098, #6798, #28344 ) ;
#30478 = CARTESIAN_POINT ( 'NONE',  ( -15.32703306334495785, 26.65709472084694909, -6.887131183944945612 ) ) ;
#30480 = CARTESIAN_POINT ( 'NONE',  ( -23.88751137688053561, -26.63245304365073807, -5.000000000000000888 ) ) ;
#30481 = CARTESIAN_POINT ( 'NONE',  ( 14.29043209799990777, -26.44292502402198863, -5.474004566143001682 ) ) ;
#30482 = FACE_OUTER_BOUND ( 'NONE', #24235, .T. ) ;
#30483 = ORIENTED_EDGE ( 'NONE', *, *, #1825, .F. ) ;
#30484 = EDGE_LOOP ( 'NONE', ( #17628, #7033, #7007, #4745 ) ) ;
#30485 = AXIS2_PLACEMENT_3D ( 'NONE', #3810, #9914, #35501 ) ;
#30486 = CARTESIAN_POINT ( 'NONE',  ( -10.82977346427968435, 32.86428370503693941, -8.960981340570279841 ) ) ;
#30487 = CARTESIAN_POINT ( 'NONE',  ( 30.90412082983257136, -0.04211290444282138334, 0.000000000000000000 ) ) ;
#30488 = EDGE_CURVE ( 'NONE', #25929, #29830, #16256, .T. ) ;
#30489 = DIRECTION ( 'NONE',  ( 1.000000000000000000, 0.000000000000000000, 0.000000000000000000 ) ) ;
#30490 = CARTESIAN_POINT ( 'NONE',  ( -9.353067506536522302, 10.78869951827630302, 10.49999999999999822 ) ) ;
#30491 = EDGE_LOOP ( 'NONE', ( #19372, #16280, #33814, #11355 ) ) ;
#30492 = CARTESIAN_POINT ( 'NONE',  ( 28.86207495170819826, 0.1351350256458582755, -11.60025332016630450 ) ) ;
#30493 = EDGE_CURVE ( 'NONE', #34024, #31085, #34590, .T. ) ;
#30494 = CARTESIAN_POINT ( 'NONE',  ( -3.118678732975735279, 7.827785988993307242, 12.00000000000000000 ) ) ;
#30495 = CARTESIAN_POINT ( 'NONE',  ( 0.5000000000000002220, 36.50000000000000711, 7.500000000000000888 ) ) ;
#30496 = ORIENTED_EDGE ( 'NONE', *, *, #1205, .F. ) ;
#30497 = CARTESIAN_POINT ( 'NONE',  ( -26.50117175307022421, 0.2815291374478115505, -15.45087338150947609 ) ) ;
#30498 = CARTESIAN_POINT ( 'NONE',  ( 14.36830325120613239, 20.48707633493483371, 11.00000000000000000 ) ) ;
#30499 = ORIENTED_EDGE ( 'NONE', *, *, #115, .T. ) ;
#30500 = CARTESIAN_POINT ( 'NONE',  ( 33.02287403607468264, -4.040597451033075771, -8.593868954784237957 ) ) ;
#30501 = ADVANCED_FACE ( 'NONE', ( #28642 ), #12552, .T. ) ;
#30502 = CARTESIAN_POINT ( 'NONE',  ( 22.69490999519655006, -28.86496244640809650, 12.73282698324817552 ) ) ;
#30503 = VERTEX_POINT ( 'NONE', #37596 ) ;
#30504 = CARTESIAN_POINT ( 'NONE',  ( -15.75274587708708474, 28.77197995862396240, 15.13084544680146770 ) ) ;
#30505 = CARTESIAN_POINT ( 'NONE',  ( 4.283810552457587037E-14, -19.51153516500234630, 19.99202127657103389 ) ) ;
#30506 = CARTESIAN_POINT ( 'NONE',  ( -5.237540274239745663, 35.49300472853438038, 9.500000000000000000 ) ) ;
#30507 = CARTESIAN_POINT ( 'NONE',  ( -1.161969254298623522, 33.23463598332011770, 19.99202127657103034 ) ) ;
#30508 = AXIS2_PLACEMENT_3D ( 'NONE', #26814, #33125, #39400 ) ;
#30509 = CARTESIAN_POINT ( 'NONE',  ( 4.003810537522394242, 8.420815593655317954, 10.49999999999999822 ) ) ;
#30510 = ORIENTED_EDGE ( 'NONE', *, *, #26514, .F. ) ;
#30511 = CARTESIAN_POINT ( 'NONE',  ( -6.953812613386785912, 14.77701242934787906, 12.00000000000000000 ) ) ;
#30512 = DIRECTION ( 'NONE',  ( 0.1564344650402373915, 0.9876883405951366601, 1.143885345364396926E-15 ) ) ;
#30513 = VECTOR ( 'NONE', #21846, 1000.000000000000000 ) ;
#30514 = ADVANCED_FACE ( 'NONE', ( #21946 ), #22142, .T. ) ;
#30515 = EDGE_CURVE ( 'NONE', #7567, #16860, #1019, .T. ) ;
#30516 = CARTESIAN_POINT ( 'NONE',  ( 8.151676898411890804, 36.26115058741275732, -5.869408836369663263 ) ) ;
#30517 = DIRECTION ( 'NONE',  ( 0.000000000000000000, 0.000000000000000000, 1.000000000000000000 ) ) ;
#30518 = CARTESIAN_POINT ( 'NONE',  ( 26.56332897235149559, -4.302820985781383278, 20.25080042701566541 ) ) ;
#30519 = CARTESIAN_POINT ( 'NONE',  ( 12.21416419421548660, -19.63058848957433256, -21.43431398639220831 ) ) ;
#30520 = SURFACE_STYLE_USAGE ( .BOTH. , #11822 ) ;
#30521 = DIRECTION ( 'NONE',  ( -0.6691306063588678965, -0.7431448254773855844, 0.000000000000000000 ) ) ;
#30522 = DIRECTION ( 'NONE',  ( 0.000000000000000000, 0.000000000000000000, 1.000000000000000000 ) ) ;
#30523 = ORIENTED_EDGE ( 'NONE', *, *, #21762, .F. ) ;
#30524 = CARTESIAN_POINT ( 'NONE',  ( 14.81250384572173395, 25.69514127254151603, -10.17503788168345302 ) ) ;
#30525 = ORIENTED_EDGE ( 'NONE', *, *, #16636, .F. ) ;
#30526 = CARTESIAN_POINT ( 'NONE',  ( -15.37753457773980870, 26.65290648949110874, -6.417023895753770191 ) ) ;
#30527 = CIRCLE ( 'NONE', #34400, 1.000000000000016431 ) ;
#30528 = CARTESIAN_POINT ( 'NONE',  ( -29.15792305772344761, -20.09428552990363670, 18.87996532025785257 ) ) ;
#30529 = CARTESIAN_POINT ( 'NONE',  ( 10.79086491057129393, -20.00149296152361345, -21.62300246481197874 ) ) ;
#30530 = FACE_OUTER_BOUND ( 'NONE', #36218, .T. ) ;
#30531 = CARTESIAN_POINT ( 'NONE',  ( 13.55580735823829208, 22.69008329597610540, -15.45968526880065141 ) ) ;
#30532 = ORIENTED_EDGE ( 'NONE', *, *, #28950, .F. ) ;
#30533 = ORIENTED_EDGE ( 'NONE', *, *, #8280, .T. ) ;
#30535 = CARTESIAN_POINT ( 'NONE',  ( -6.677405195726899834, 35.94657184102484138, 10.49999999999999822 ) ) ;
#30534 = CARTESIAN_POINT ( 'NONE',  ( -15.19527047305266443, 27.50996873332976378, -5.470726252303037995 ) ) ;
#30536 = CARTESIAN_POINT ( 'NONE',  ( -18.50146268769051261, -26.05940927080308001, -9.995050714716832374 ) ) ;
#30537 = EDGE_CURVE ( 'NONE', #6333, #11673, #21742, .T. ) ;
#30538 = DIRECTION ( 'NONE',  ( 0.3090169943749451198, -0.9510565162951544194, 0.000000000000000000 ) ) ;
#30539 = ORIENTED_EDGE ( 'NONE', *, *, #11114, .F. ) ;
#30540 = CARTESIAN_POINT ( 'NONE',  ( -21.26011989971568994, -8.067792608035599500, -23.06233089094039101 ) ) ;
#30541 = CARTESIAN_POINT ( 'NONE',  ( -12.74073895253298616, -23.07826477149550826, -15.46828449374485892 ) ) ;
#30542 = CARTESIAN_POINT ( 'NONE',  ( 38.42882785865609918, -4.479089857565665689, 22.99999999999905853 ) ) ;
#30543 = ORIENTED_EDGE ( 'NONE', *, *, #31738, .T. ) ;
#30544 = CARTESIAN_POINT ( 'NONE',  ( 20.64171730712855535, 2.398676254270919017, -26.94157980996323687 ) ) ;
#30545 = EDGE_CURVE ( 'NONE', #4057, #17936, #3262, .T. ) ;
#30546 = DIRECTION ( 'NONE',  ( -0.5000000000000039968, -0.8660254037844363761, 0.000000000000000000 ) ) ;
#30547 = DIRECTION ( 'NONE',  ( 0.000000000000000000, 0.000000000000000000, 1.000000000000000000 ) ) ;
#30548 = AXIS2_PLACEMENT_3D ( 'NONE', #12616, #15866, #24608 ) ;
#30549 = ORIENTED_EDGE ( 'NONE', *, *, #3550, .F. ) ;
#30550 = CARTESIAN_POINT ( 'NONE',  ( -30.25321886983080333, -0.06122810112208476596, -8.763529956286015832 ) ) ;
#30551 = VERTEX_POINT ( 'NONE', #29247 ) ;
#30552 = CARTESIAN_POINT ( 'NONE',  ( 20.49959133494802543, 0.2219702378425628120, -29.33667080960374562 ) ) ;
#30553 = CARTESIAN_POINT ( 'NONE',  ( 32.94564365859739752, -13.95995841273500915, 18.42518152272108978 ) ) ;
#30554 = EDGE_LOOP ( 'NONE', ( #25074, #8012, #629, #1512 ) ) ;
#30555 = CARTESIAN_POINT ( 'NONE',  ( -20.68010352585984535, 2.885225430730191221, -26.38554717714988129 ) ) ;
#30556 = CARTESIAN_POINT ( 'NONE',  ( -8.917741276437942233, 30.52956727630665057, 13.00000000000000178 ) ) ;
#30557 = CARTESIAN_POINT ( 'NONE',  ( 4.984135866956514782, 36.15314577889351000, 10.49999999999999467 ) ) ;
#30558 = CIRCLE ( 'NONE', #36, 6.000000000000003553 ) ;
#30559 = FACE_OUTER_BOUND ( 'NONE', #4380, .T. ) ;
#30560 = CIRCLE ( 'NONE', #33145, 1.000000000000000888 ) ;
#30561 = CARTESIAN_POINT ( 'NONE',  ( 0.000000000000000000, 22.50000000000000355, 11.00000000000000178 ) ) ;
#30562 = FACE_BOUND ( 'NONE', #23226, .T. ) ;
#30563 = CYLINDRICAL_SURFACE ( 'NONE', #19187, 1.000000000000000000 ) ;
#30564 = ORIENTED_EDGE ( 'NONE', *, *, #23023, .T. ) ;
#30565 = CARTESIAN_POINT ( 'NONE',  ( -21.17445498011162996, 7.452892634864654475, -18.99389871435994337 ) ) ;
#30566 = DIRECTION ( 'NONE',  ( 1.000000000000000000, 0.000000000000000000, 0.000000000000000000 ) ) ;
#30567 = PLANE ( 'NONE',  #628 ) ;
#30568 = CARTESIAN_POINT ( 'NONE',  ( 22.95814010875989197, -22.53209843378533606, -12.99612941548552492 ) ) ;
#30569 = EDGE_CURVE ( 'NONE', #32217, #25659, #35232, .T. ) ;
#30570 = VECTOR ( 'NONE', #16217, 1000.000000000000000 ) ;
#30571 = DIRECTION ( 'NONE',  ( 0.3535533905932713994, -0.6123724356958013537, -0.7071067811865427988 ) ) ;
#30572 = CARTESIAN_POINT ( 'NONE',  ( 14.83882917549554037, 26.09951300090577320, -9.692528519113288610 ) ) ;
#30573 = CARTESIAN_POINT ( 'NONE',  ( 10.24066009500897856, -26.58087177406422796, 14.53008259253875067 ) ) ;
#30574 = VERTEX_POINT ( 'NONE', #1827 ) ;
#30575 = CARTESIAN_POINT ( 'NONE',  ( -12.39465856751968609, 16.66586351761176843, -26.93958671274752348 ) ) ;
#30576 = CARTESIAN_POINT ( 'NONE',  ( -25.38348611796456922, -5.460896781496030528, 20.69868183039781684 ) ) ;
#30577 = DIRECTION ( 'NONE',  ( 0.000000000000000000, 0.000000000000000000, -1.000000000000000000 ) ) ;
#30578 = CARTESIAN_POINT ( 'NONE',  ( 12.94545362548832124, 21.62528871782362216, -17.44060035758700522 ) ) ;
#30579 = ORIENTED_EDGE ( 'NONE', *, *, #1944, .T. ) ;
#30580 = B_SPLINE_CURVE_WITH_KNOTS ( 'NONE', 3,
 ( #26150, #38548, #23511, #21069 ),
 .UNSPECIFIED., .F., .F.,
 ( 4, 4 ),
 ( 0.000000000000000000, 1.000000000000000000 ),
 .UNSPECIFIED. ) ;
#30581 = DIRECTION ( 'NONE',  ( 1.000000000000000000, 0.000000000000000000, 0.000000000000000000 ) ) ;
#30582 = EDGE_LOOP ( 'NONE', ( #4042, #27153, #34629 ) ) ;
#30584 = CARTESIAN_POINT ( 'NONE',  ( 13.32151712420403555, 20.09434385051836358, 10.00000000000000000 ) ) ;
#30583 = CARTESIAN_POINT ( 'NONE',  ( -14.95596380865394970, 26.16937309837150138, -9.228359069169592033 ) ) ;
#30585 = CARTESIAN_POINT ( 'NONE',  ( -13.40009855081921053, -23.62524794187952892, -14.47403050587199225 ) ) ;
#30586 = CARTESIAN_POINT ( 'NONE',  ( -14.06524961900331760, 27.71236540882611621, 7.499999999999993783 ) ) ;
#30587 = VECTOR ( 'NONE', #17327, 1000.000000000000000 ) ;
#30588 = CARTESIAN_POINT ( 'NONE',  ( -17.63393726088407121, -10.64200091597105846, -28.44387009623618212 ) ) ;
#30589 = CARTESIAN_POINT ( 'NONE',  ( -12.39553123186617611, -23.97331200851148125, -13.57268788837447637 ) ) ;
#30590 = CARTESIAN_POINT ( 'NONE',  ( -5.767236651883567156, 13.71142893291686171, 10.50000000000000000 ) ) ;
#30591 = CARTESIAN_POINT ( 'NONE',  ( 16.25725326718474406, 23.79337420548043980, -6.422359314754682025 ) ) ;
#30592 = ORIENTED_EDGE ( 'NONE', *, *, #27474, .T. ) ;
#30593 = CARTESIAN_POINT ( 'NONE',  ( 23.36873701481537680, 7.189358073232670954, -12.82796446375462551 ) ) ;
#30594 = CIRCLE ( 'NONE', #19548, 1.000000000000000888 ) ;
#30595 = DIRECTION ( 'NONE',  ( -0.000000000000000000, 0.000000000000000000, -1.000000000000000000 ) ) ;
#30596 = CARTESIAN_POINT ( 'NONE',  ( -8.910254037844422825, 17.93301270189230223, 10.49999999999999822 ) ) ;
#30597 = CARTESIAN_POINT ( 'NONE',  ( -9.941034666242671847, 32.57396620494226624, 11.00000000000000000 ) ) ;
#30598 = EDGE_LOOP ( 'NONE', ( #35861, #22723, #36896, #10886 ) ) ;
#30599 = CARTESIAN_POINT ( 'NONE',  ( -28.28993293699624090, -0.5497182594458693838, -13.43537464208401033 ) ) ;
#30600 = CARTESIAN_POINT ( 'NONE',  ( 30.76969935483850804, -0.1781414310780859711, -7.352071795213825922 ) ) ;
#30601 = CARTESIAN_POINT ( 'NONE',  ( 5.034171952702011232, 35.03623199971301005, 9.500000000000000000 ) ) ;
#30602 = CARTESIAN_POINT ( 'NONE',  ( 17.21213525677114120, -20.06193531423682685, 20.50957957746029692 ) ) ;
#30603 = CARTESIAN_POINT ( 'NONE',  ( 33.62187204924162387, 0.04418559750795045954, -13.79123840944733992 ) ) ;
#30604 = CARTESIAN_POINT ( 'NONE',  ( 0.6237317017440463518, 25.43444280220171194, 13.00000000000000178 ) ) ;
#30605 = ORIENTED_EDGE ( 'NONE', *, *, #36449, .T. ) ;
#30606 = FACE_OUTER_BOUND ( 'NONE', #30364, .T. ) ;
#30607 = AXIS2_PLACEMENT_3D ( 'NONE', #14012, #29050, #23563 ) ;
#30608 = CARTESIAN_POINT ( 'NONE',  ( 23.60287484585659001, 26.76891282270896610, 9.500000000000000000 ) ) ;
#30609 = CARTESIAN_POINT ( 'NONE',  ( 9.677076426724163127, 26.69573495723207657, 10.50000000000000000 ) ) ;
#30610 = CARTESIAN_POINT ( 'NONE',  ( 2.163616898793370602, 30.08412298609989222, -15.68737937765401291 ) ) ;
#30611 = CIRCLE ( 'NONE', #13076, 1.000000000000000888 ) ;
#30612 = CARTESIAN_POINT ( 'NONE',  ( -12.53024597560957609, 27.62278594035707968, 10.00000000000000000 ) ) ;
#30613 = EDGE_CURVE ( 'NONE', #35248, #11406, #1418, .T. ) ;
#30614 = CARTESIAN_POINT ( 'NONE',  ( 9.697889840765411051, 31.90483559858327212, 10.00000000000000000 ) ) ;
#30615 = DIRECTION ( 'NONE',  ( 0.000000000000000000, -0.000000000000000000, 1.000000000000000000 ) ) ;
#30616 = DIRECTION ( 'NONE',  ( 0.9135454576426005335, -0.4067366430758009299, 0.000000000000000000 ) ) ;
#30617 = CARTESIAN_POINT ( 'NONE',  ( -9.593266739736646898, 18.11602540378452986, 11.00000000000000000 ) ) ;
#30618 = CARTESIAN_POINT ( 'NONE',  ( -9.997483185316569987, 21.95197631500770896, 10.49999999999999467 ) ) ;
#30619 = CARTESIAN_POINT ( 'NONE',  ( 14.77611408087021694, 27.12164188139913534, -8.725285341602761591 ) ) ;
#30620 = CARTESIAN_POINT ( 'NONE',  ( -4.940908595777636414, 35.94977745735568675, 7.500000000000000888 ) ) ;
#30621 = ORIENTED_EDGE ( 'NONE', *, *, #35046, .T. ) ;
#30623 = FACE_OUTER_BOUND ( 'NONE', #7334, .T. ) ;
#30622 = CARTESIAN_POINT ( 'NONE',  ( -19.20284012471338642, 16.64839643360665633, -5.480717218555573034 ) ) ;
#30624 = EDGE_CURVE ( 'NONE', #5290, #31950, #22890, .T. ) ;
#30625 = DIRECTION ( 'NONE',  ( 0.000000000000000000, 0.000000000000000000, 1.000000000000000000 ) ) ;
#30626 = CIRCLE ( 'NONE', #37748, 16.00000000000000000 ) ;
#30627 = CARTESIAN_POINT ( 'NONE',  ( 14.36179435970547402, -25.07121135651426869, -11.59890311405379748 ) ) ;
#30628 = EDGE_CURVE ( 'NONE', #36251, #6243, #17066, .T. ) ;
#30629 = CARTESIAN_POINT ( 'NONE',  ( -22.42780984720763371, -26.55233249316436428, -7.652769933138617198 ) ) ;
#30630 = CARTESIAN_POINT ( 'NONE',  ( 32.33143948541787438, 1.358872982501792226, 11.00000000000000000 ) ) ;
#30631 = CARTESIAN_POINT ( 'NONE',  ( 14.51908200401363302, 25.00878969398502960, -11.59620987194703012 ) ) ;
#30632 = ORIENTED_EDGE ( 'NONE', *, *, #19203, .F. ) ;
#30633 = CYLINDRICAL_SURFACE ( 'NONE', #34134, 6.000000000000001776 ) ;
#30634 = DIRECTION ( 'NONE',  ( 0.8660254037844431485, 0.4999999999999921174, -0.000000000000000000 ) ) ;
#30635 = CARTESIAN_POINT ( 'NONE',  ( -33.02831943717539787, -0.5583946152437758714, 14.53008259253993728 ) ) ;
#30636 = CARTESIAN_POINT ( 'NONE',  ( -28.98287275701582644, -24.11882464604644127, -5.863716236549250560 ) ) ;
#30637 = CARTESIAN_POINT ( 'NONE',  ( -0.3811350534766741460, -24.48451870251001594, -8.900403566480946438 ) ) ;
#30638 = CARTESIAN_POINT ( 'NONE',  ( 11.51224750557763699, 17.87894272431910991, -25.04142208898249677 ) ) ;
#30639 = CARTESIAN_POINT ( 'NONE',  ( 17.89753197511066674, 10.02670602479014228, -29.99999999999999645 ) ) ;
#30640 = CARTESIAN_POINT ( 'NONE',  ( -8.315274455032252376, 10.01576150750523375, 7.500000000000000888 ) ) ;
#30641 = CARTESIAN_POINT ( 'NONE',  ( -4.212426069905327530, 37.97930161814787198, -5.436632083248686520 ) ) ;
#30642 = ORIENTED_EDGE ( 'NONE', *, *, #29059, .F. ) ;
#30643 = CARTESIAN_POINT ( 'NONE',  ( -33.92430155621369892, -6.368002694854169476, -8.531665187152857044 ) ) ;
#30644 = CARTESIAN_POINT ( 'NONE',  ( -17.34253826607185545, 27.32041144404030675, 11.00000000000000000 ) ) ;
#30645 = ORIENTED_EDGE ( 'NONE', *, *, #11083, .T. ) ;
#30646 = CARTESIAN_POINT ( 'NONE',  ( -14.47283171447380390, 21.48159823030330884, 7.500000000000004441 ) ) ;
#30647 = EDGE_CURVE ( 'NONE', #14093, #32234, #11164, .T. ) ;
#30648 = DIRECTION ( 'NONE',  ( -0.3090169943749449533, 0.9510565162951544194, 0.000000000000000000 ) ) ;
#30649 = EDGE_CURVE ( 'NONE', #15047, #11157, #1535, .T. ) ;
#30650 = CARTESIAN_POINT ( 'NONE',  ( -20.46571904345125148, 1.196608941699672357, -30.00000000000000000 ) ) ;
#30651 = CARTESIAN_POINT ( 'NONE',  ( 34.48754613114789436, -12.67185989539148849, -8.433237745870078683 ) ) ;
#30652 = VERTEX_POINT ( 'NONE', #14004 ) ;
#30653 = VECTOR ( 'NONE', #24096, 1000.000000000000114 ) ;
#30654 = CARTESIAN_POINT ( 'NONE',  ( 13.63581098909226519, 27.45627467658428600, 7.500000000000000888 ) ) ;
#30655 = ORIENTED_EDGE ( 'NONE', *, *, #28735, .F. ) ;
#30656 = CARTESIAN_POINT ( 'NONE',  ( -5.400683141673551901, 15.91724817395922997, 9.000000000000001776 ) ) ;
#30657 = DIRECTION ( 'NONE',  ( -1.000000000000000000, 0.000000000000000000, 0.000000000000000000 ) ) ;
#30658 = VECTOR ( 'NONE', #999, 1000.000000000000000 ) ;
#30659 = CARTESIAN_POINT ( 'NONE',  ( -1.265509184090266137, 8.754836972118123839, 6.000000000000000000 ) ) ;
#30660 = ORIENTED_EDGE ( 'NONE', *, *, #33302, .T. ) ;
#30661 = CARTESIAN_POINT ( 'NONE',  ( -2.340242103211412239, 21.29936263313340206, -25.60352335172182947 ) ) ;
#30662 = CARTESIAN_POINT ( 'NONE',  ( -10.41268156625113228, 18.79179606750104981, 13.00000000000000178 ) ) ;
#30663 = DIRECTION ( 'NONE',  ( 1.000000000000000000, 0.000000000000000000, 0.000000000000000000 ) ) ;
#30664 = DIRECTION ( 'NONE',  ( -0.5000000000000038858, -0.8660254037844364872, 0.000000000000000000 ) ) ;
#30665 = EDGE_CURVE ( 'NONE', #33664, #9387, #17122, .T. ) ;
#30666 = CARTESIAN_POINT ( 'NONE',  ( 28.95584039848980140, -23.67695839038157857, -7.136634946781046374 ) ) ;
#30667 = CARTESIAN_POINT ( 'NONE',  ( 16.46100146899417993, 13.93030935198141229, -22.17668661662577279 ) ) ;
#30668 = CARTESIAN_POINT ( 'NONE',  ( 7.299606265389828152, 20.47042108248343695, -24.54268700408873372 ) ) ;
#30669 = ORIENTED_EDGE ( 'NONE', *, *, #1313, .T. ) ;
#30670 = CARTESIAN_POINT ( 'NONE',  ( -21.80410373500361487, 11.76501844773795824, -5.967298349106835431 ) ) ;
#30671 = AXIS2_PLACEMENT_3D ( 'NONE', #37452, #39701, #21215 ) ;
#30672 = DIRECTION ( 'NONE',  ( 0.5000000000000026645, 0.8660254037844372643, 0.000000000000000000 ) ) ;
#30673 = CARTESIAN_POINT ( 'NONE',  ( 12.80584978270169394, -22.56157762115984866, -16.42713908487053587 ) ) ;
#30674 = DIRECTION ( 'NONE',  ( 0.3535533905932903287, 0.6123724356957876980, 0.7071067811865451302 ) ) ;
#30675 = DIRECTION ( 'NONE',  ( 0.000000000000000000, 0.000000000000000000, -1.000000000000000000 ) ) ;
#30676 = CARTESIAN_POINT ( 'NONE',  ( -15.40119896161133006, 26.83624744099596171, -5.000000000000001776 ) ) ;
#30677 = CARTESIAN_POINT ( 'NONE',  ( -22.86303537443307476, -25.58751383834528070, -9.408386063524703857 ) ) ;
#30678 = CARTESIAN_POINT ( 'NONE',  ( 10.74915096743506027, -25.64641579889018885, -5.950130972811642494 ) ) ;
#30679 = AXIS2_PLACEMENT_3D ( 'NONE', #27239, #30694, #28036 ) ;
#30680 = FACE_OUTER_BOUND ( 'NONE', #36988, .T. ) ;
#30681 = ORIENTED_EDGE ( 'NONE', *, *, #37651, .T. ) ;
#30682 = EDGE_LOOP ( 'NONE', ( #1656, #10937, #18290, #16592, #32750 ) ) ;
#30683 = CARTESIAN_POINT ( 'NONE',  ( -10.96238246107026626, 33.32429186611522454, -8.073152806041559160 ) ) ;
#30684 = CARTESIAN_POINT ( 'NONE',  ( 1.000000000000000000, 37.00000000000000711, 10.50000000000000178 ) ) ;
#30685 = AXIS2_PLACEMENT_3D ( 'NONE', #9194, #27286, #14897 ) ;
#30686 = CARTESIAN_POINT ( 'NONE',  ( -7.111215932167764819, 17.81698729810783988, 9.000000000000001776 ) ) ;
#30687 = ORIENTED_EDGE ( 'NONE', *, *, #33477, .T. ) ;
#30688 = CARTESIAN_POINT ( 'NONE',  ( 27.73864469095863683, 0.1886746684874264501, -13.51343220089273167 ) ) ;
#30689 = DIRECTION ( 'NONE',  ( 0.000000000000000000, 0.000000000000000000, 1.000000000000000000 ) ) ;
#30690 = DIRECTION ( 'NONE',  ( -0.000000000000000000, 0.000000000000000000, 1.000000000000000000 ) ) ;
#30691 = EDGE_CURVE ( 'NONE', #802, #39848, #29845, .T. ) ;
#30692 = EDGE_LOOP ( 'NONE', ( #27681, #11358 ) ) ;
#30693 = CARTESIAN_POINT ( 'NONE',  ( -20.48057623381365033, 0.8922431241703840943, -29.34897116163656960 ) ) ;
#30694 = DIRECTION ( 'NONE',  ( 0.000000000000000000, 0.000000000000000000, 1.000000000000000000 ) ) ;
#30695 = AXIS2_PLACEMENT_3D ( 'NONE', #15168, #28346, #15366 ) ;
#30696 = ORIENTED_EDGE ( 'NONE', *, *, #20027, .F. ) ;
#30697 = CARTESIAN_POINT ( 'NONE',  ( 31.61045151917019069, -6.540495618978702907, -12.13482048140255287 ) ) ;
#30698 = ORIENTED_EDGE ( 'NONE', *, *, #9857, .T. ) ;
#30699 = CARTESIAN_POINT ( 'NONE',  ( 10.77072277543604351, 36.67279993932673676, 12.73282698324853435 ) ) ;
#30700 = CARTESIAN_POINT ( 'NONE',  ( 4.287285461719674021E-14, -18.69445663741131014, 20.25080042701566541 ) ) ;
#30701 = DIRECTION ( 'NONE',  ( 1.000000000000000000, 0.000000000000000000, -0.000000000000000000 ) ) ;
#30702 = CARTESIAN_POINT ( 'NONE',  ( -7.420252307062940034, 30.34362403113889073, 19.99202127657163075 ) ) ;
#30703 = VECTOR ( 'NONE', #20257, 1000.000000000000000 ) ;
#30704 = LINE ( 'NONE', #21, #29807 ) ;
#30705 = ORIENTED_EDGE ( 'NONE', *, *, #32462, .F. ) ;
#30706 = DIRECTION ( 'NONE',  ( -1.000000000000000000, 0.000000000000000000, 0.000000000000000000 ) ) ;
#30707 = VECTOR ( 'NONE', #37262, 1000.000000000000000 ) ;
#30708 = CARTESIAN_POINT ( 'NONE',  ( -3.835137251120299684, 29.44922644035488446, 6.000000000000000000 ) ) ;
#30709 = DIRECTION ( 'NONE',  ( 1.000000000000000000, 0.000000000000000000, 0.000000000000000000 ) ) ;
#30710 = ADVANCED_FACE ( 'NONE', ( #13600 ), #19048, .T. ) ;
#30711 = CARTESIAN_POINT ( 'NONE',  ( 8.159785424745114923, 36.31054560068550785, -5.440753753161995832 ) ) ;
#30712 = VECTOR ( 'NONE', #19495, 1000.000000000000000 ) ;
#30713 = EDGE_CURVE ( 'NONE', #5055, #18400, #894, .T. ) ;
#30714 = DIRECTION ( 'NONE',  ( 0.9781476007338067991, 0.2079116908177533474, -0.000000000000000000 ) ) ;
#30715 = ADVANCED_FACE ( 'NONE', ( #23356 ), #23147, .T. ) ;
#30716 = CARTESIAN_POINT ( 'NONE',  ( 12.51578678884064466, -18.90026018402930674, -22.47850626938384266 ) ) ;
#30717 =( NAMED_UNIT ( * ) PLANE_ANGLE_UNIT ( ) SI_UNIT ( $, .RADIAN. ) );
#30718 = CARTESIAN_POINT ( 'NONE',  ( -12.97058434440066677, 15.58877990640330857, 10.96580508970284384 ) ) ;
#30719 = PLANE ( 'NONE',  #35544 ) ;
#30720 = CIRCLE ( 'NONE', #21637, 1.000000000000000888 ) ;
#30721 = EDGE_LOOP ( 'NONE', ( #4658, #34604 ) ) ;
#30722 = CARTESIAN_POINT ( 'NONE',  ( -13.34174550214330957, 22.00054098145283277, -16.46453111791931079 ) ) ;
#30723 = EDGE_CURVE ( 'NONE', #8916, #38300, #25988, .T. ) ;
#30724 = CARTESIAN_POINT ( 'NONE',  ( -30.82027224585467096, -2.301877357439013227, 17.92354375535249389 ) ) ;
#30725 = CARTESIAN_POINT ( 'NONE',  ( 15.16712867651880003, -26.63505783696666640, -5.946131006634350236 ) ) ;
#30726 = CARTESIAN_POINT ( 'NONE',  ( -3.553336972204574007, 8.187731063815915533, 10.94387467463493913 ) ) ;
#30727 = ORIENTED_EDGE ( 'NONE', *, *, #11540, .F. ) ;
#30728 = EDGE_LOOP ( 'NONE', ( #4597, #26508, #38925, #4865 ) ) ;
#30729 = CARTESIAN_POINT ( 'NONE',  ( -11.09811852199402082, 22.05552288639037073, -19.25227300847279110 ) ) ;
#30730 = CARTESIAN_POINT ( 'NONE',  ( -13.36679029698933086, -19.22344594692958708, -21.28930016379315404 ) ) ;
#30731 = CARTESIAN_POINT ( 'NONE',  ( -1.485571585149978668, -11.24999999999982236, 3.000000000000000000 ) ) ;
#30732 = ORIENTED_EDGE ( 'NONE', *, *, #32717, .T. ) ;
#30733 = CARTESIAN_POINT ( 'NONE',  ( -35.47307300072858283, -9.938437602308624719, -5.442375005290738699 ) ) ;
#30734 = CARTESIAN_POINT ( 'NONE',  ( -9.245064759184387526, -18.29713783020200424, -30.00000000000000000 ) ) ;
#30735 = DIRECTION ( 'NONE',  ( -0.000000000000000000, -0.000000000000000000, -1.000000000000000000 ) ) ;
#30736 = ORIENTED_EDGE ( 'NONE', *, *, #2196, .T. ) ;
#30737 = CARTESIAN_POINT ( 'NONE',  ( 20.51663963794920065, 1.053696994703543055, -28.71375515118313970 ) ) ;
#30738 = CARTESIAN_POINT ( 'NONE',  ( -21.39877161664097827, 15.54711762656374141, 7.000000000000000000 ) ) ;
#30739 = CARTESIAN_POINT ( 'NONE',  ( -14.26585111513660031, 17.86474508437623143, 12.00000000000000000 ) ) ;
#30740 = ADVANCED_FACE ( 'NONE', ( #35545 ), #25532, .T. ) ;
#30741 = ORIENTED_EDGE ( 'NONE', *, *, #22739, .F. ) ;
#30742 = ADVANCED_FACE ( 'NONE', ( #38990 ), #4859, .T. ) ;
#30743 = CARTESIAN_POINT ( 'NONE',  ( -23.97549446410291552, 0.4047595829504309628, -19.48518163238001577 ) ) ;
#30745 = EDGE_CURVE ( 'NONE', #38528, #18297, #9710, .T. ) ;
#30744 = VERTEX_POINT ( 'NONE', #26598 ) ;
#30746 = CARTESIAN_POINT ( 'NONE',  ( 30.19373506806564933, -1.611421832312862179, -11.45916374511738489 ) ) ;
#30747 = AXIS2_PLACEMENT_3D ( 'NONE', #2620, #5462, #5264 ) ;
#30748 = CARTESIAN_POINT ( 'NONE',  ( 13.80182853280054900, -15.17292971133294444, -30.00000000000000355 ) ) ;
#30749 = CARTESIAN_POINT ( 'NONE',  ( 32.91936639158326017, -8.047070124325959029, 18.42518152272108622 ) ) ;
#30750 = ORIENTED_EDGE ( 'NONE', *, *, #4509, .T. ) ;
#30751 = CARTESIAN_POINT ( 'NONE',  ( -27.53998928449781047, 3.518557584072389943, -6.903689457210364644 ) ) ;
#30752 = CARTESIAN_POINT ( 'NONE',  ( -30.90412082983255715, -0.04211290444283005696, -5.000000000000000000 ) ) ;
#30753 = DIRECTION ( 'NONE',  ( -0.000000000000000000, -0.000000000000000000, -1.000000000000000000 ) ) ;
#30754 = AXIS2_PLACEMENT_3D ( 'NONE', #12902, #13093, #34643 ) ;
#30755 = CARTESIAN_POINT ( 'NONE',  ( -18.00000000000000000, 22.50000000000001066, 6.000000000000000000 ) ) ;
#30756 = CARTESIAN_POINT ( 'NONE',  ( -39.48557158514991272, -11.24999999999982414, 3.000000000000000000 ) ) ;
#30757 = EDGE_CURVE ( 'NONE', #708, #27813, #5421, .T. ) ;
#30758 = AXIS2_PLACEMENT_3D ( 'NONE', #6511, #8775, #33571 ) ;
#30759 = FACE_BOUND ( 'NONE', #32288, .T. ) ;
#30760 = EDGE_CURVE ( 'NONE', #15620, #9244, #17492, .T. ) ;
#30761 = CARTESIAN_POINT ( 'NONE',  ( 23.01716326618264574, 13.28896540771174628, 12.73282698324853257 ) ) ;
#30762 = ORIENTED_EDGE ( 'NONE', *, *, #2234, .F. ) ;
#30763 = CARTESIAN_POINT ( 'NONE',  ( -24.79671477329043228, 7.114048960549892442, -6.442296327763719965 ) ) ;
#30764 = CARTESIAN_POINT ( 'NONE',  ( -7.577547685840081648, 11.84256962714647798, 12.00000000000000000 ) ) ;
#30765 = DIRECTION ( 'NONE',  ( 1.000000000000000000, 0.000000000000000000, 0.000000000000000000 ) ) ;
#30766 = CARTESIAN_POINT ( 'NONE',  ( 14.27600272946170890, -15.79691008733334634, -25.79950180772068080 ) ) ;
#30767 = CARTESIAN_POINT ( 'NONE',  ( 0.000000000000000000, 22.50000000000000355, 6.000000000000000000 ) ) ;
#30768 = CARTESIAN_POINT ( 'NONE',  ( 15.29414933734400428, 26.94219312171647118, -6.412878494969166177 ) ) ;
#30769 = EDGE_LOOP ( 'NONE', ( #3991, #26674 ) ) ;
#30770 = AXIS2_PLACEMENT_3D ( 'NONE', #37291, #21843, #22046 ) ;
#30771 = CARTESIAN_POINT ( 'NONE',  ( -12.27438659830399104, 16.41897796854597047, -29.37404837115920131 ) ) ;
#30772 = CARTESIAN_POINT ( 'NONE',  ( -25.82695741053184335, -7.282955883995192892, 20.82122704794065982 ) ) ;
#30773 = DIRECTION ( 'NONE',  ( 0.000000000000000000, 0.000000000000000000, 1.000000000000000000 ) ) ;
#30774 = CARTESIAN_POINT ( 'NONE',  ( 13.22333277151671105, 22.21094483373017425, -16.44622722129113512 ) ) ;
#30775 = ORIENTED_EDGE ( 'NONE', *, *, #17882, .T. ) ;
#30776 = CARTESIAN_POINT ( 'NONE',  ( 0.000000000000000000, 22.50000000000000355, 0.000000000000000000 ) ) ;
#30777 = ORIENTED_EDGE ( 'NONE', *, *, #31891, .F. ) ;
#30779 = FACE_OUTER_BOUND ( 'NONE', #37557, .T. ) ;
#30778 = CARTESIAN_POINT ( 'NONE',  ( -15.25716400807983142, 26.89584191905160537, -6.881959249777203524 ) ) ;
#30780 = CARTESIAN_POINT ( 'NONE',  ( -14.49768878875645051, -25.09694979747337484, -11.58902682695292441 ) ) ;
#30781 = CARTESIAN_POINT ( 'NONE',  ( -8.796116341590805021, 23.42450908139092647, 9.000000000000001776 ) ) ;
#30782 = CARTESIAN_POINT ( 'NONE',  ( -31.54497719551462609, -17.75878470093167039, -10.17196054166158348 ) ) ;
#30783 = VECTOR ( 'NONE', #32258, 1000.000000000000114 ) ;
#30784 = CARTESIAN_POINT ( 'NONE',  ( -12.10239668256580003, -23.52241704728540128, -14.54534583956947102 ) ) ;
#30785 = DIRECTION ( 'NONE',  ( -0.000000000000000000, -0.000000000000000000, 1.000000000000000000 ) ) ;
#30786 = CARTESIAN_POINT ( 'NONE',  ( 15.11671161907844585, 23.43369355923603337, -11.64535646599357577 ) ) ;
#30787 = VERTEX_POINT ( 'NONE', #16866 ) ;
#30788 = CARTESIAN_POINT ( 'NONE',  ( 25.58814899322283409, 5.549420531236951781, -8.847774912381147772 ) ) ;
#30789 = DIRECTION ( 'NONE',  ( -0.2079116908177663647, -0.9781476007338042455, 0.000000000000000000 ) ) ;
#30790 = CARTESIAN_POINT ( 'NONE',  ( 7.353987181296509412, 35.57359447655183970, 7.000000000000000000 ) ) ;
#30791 = CARTESIAN_POINT ( 'NONE',  ( -10.73859285986284640, 31.49625607628545154, 7.500000000000004441 ) ) ;
#30792 = ORIENTED_EDGE ( 'NONE', *, *, #2330, .T. ) ;
#30793 = CARTESIAN_POINT ( 'NONE',  ( -24.35468204290444660, -0.5538618444963721021, -19.35839232206769367 ) ) ;
#30794 = EDGE_CURVE ( 'NONE', #3290, #36352, #32037, .T. ) ;
#30795 = AXIS2_PLACEMENT_3D ( 'NONE', #35563, #17290, #4680 ) ;
#30796 = CARTESIAN_POINT ( 'NONE',  ( 20.48413544616686011, 0.8063757131868728445, -29.34740462186751486 ) ) ;
#30797 = LINE ( 'NONE', #11709, #30653 ) ;
#30798 = CARTESIAN_POINT ( 'NONE',  ( 26.93475362026859088, -11.92845428170237909, 20.82122704794080548 ) ) ;
#30799 = ORIENTED_EDGE ( 'NONE', *, *, #38183, .F. ) ;
#30800 = CARTESIAN_POINT ( 'NONE',  ( 17.34253826539385201, 27.32041144647958575, -5.000000000000000000 ) ) ;
#30801 = CARTESIAN_POINT ( 'NONE',  ( -6.064571727552472424, 31.45661825943146894, 12.00000000000000000 ) ) ;
#30802 = VECTOR ( 'NONE', #4356, 1000.000000000000000 ) ;
#30803 = ORIENTED_EDGE ( 'NONE', *, *, #9565, .F. ) ;
#30804 = FACE_OUTER_BOUND ( 'NONE', #7322, .T. ) ;
#30805 = LINE ( 'NONE', #2970, #3903 ) ;
#30806 = LINE ( 'NONE', #6404, #8660 ) ;
#30807 = CARTESIAN_POINT ( 'NONE',  ( 1.613298393356113136, 22.76613432878109222, -22.99758612101997102 ) ) ;
#30808 = ADVANCED_FACE ( 'NONE', ( #18266 ), #2227, .F. ) ;
#30809 = CARTESIAN_POINT ( 'NONE',  ( -11.41268156625113406, 18.79179606750104981, 12.00000000000000000 ) ) ;
#30810 = FACE_OUTER_BOUND ( 'NONE', #9311, .T. ) ;
#30811 = CARTESIAN_POINT ( 'NONE',  ( 6.404490139165906371, 34.42612703509930583, 10.00000000000000000 ) ) ;
#30812 = CARTESIAN_POINT ( 'NONE',  ( 7.118377661053320260, 10.47536095541698486, 7.000000000000000000 ) ) ;
#30813 = DIRECTION ( 'NONE',  ( 1.000000000000000000, 0.000000000000000000, 0.000000000000000000 ) ) ;
#30814 = DIRECTION ( 'NONE',  ( 1.000000000000000000, 0.000000000000000000, 0.000000000000000000 ) ) ;
#30815 = AXIS2_PLACEMENT_3D ( 'NONE', #6663, #37758, #25164 ) ;
#30816 = CARTESIAN_POINT ( 'NONE',  ( 11.93556763155846134, 21.07774700547179236, -19.40385465495243977 ) ) ;
#30817 = DIRECTION ( 'NONE',  ( 0.000000000000000000, 0.000000000000000000, 1.000000000000000000 ) ) ;
#30818 = ORIENTED_EDGE ( 'NONE', *, *, #5915, .F. ) ;
#30820 = DIRECTION ( 'NONE',  ( 0.000000000000000000, 0.000000000000000000, 1.000000000000000000 ) ) ;
#30819 = CARTESIAN_POINT ( 'NONE',  ( -17.32349603665394966, 15.91288547668971631, -15.86201918625455853 ) ) ;
#30821 = CARTESIAN_POINT ( 'NONE',  ( 13.21633695260872976, 15.44689457190012227, 10.68306085400107541 ) ) ;
#30822 = CARTESIAN_POINT ( 'NONE',  ( 9.704060306507821920, -18.43476937023081419, -26.82927739930571320 ) ) ;
#30823 = CARTESIAN_POINT ( 'NONE',  ( -12.79957064338231554, -17.39491785756841935, -24.68155700860378232 ) ) ;
#30824 = CARTESIAN_POINT ( 'NONE',  ( 14.93529390890676822, 25.79829262747118790, -9.709001792061668468 ) ) ;
#30825 = CARTESIAN_POINT ( 'NONE',  ( 14.02229904730994292, 23.95306976838152480, -13.51159946331490147 ) ) ;
#30826 = ORIENTED_EDGE ( 'NONE', *, *, #710, .F. ) ;
#30827 = CARTESIAN_POINT ( 'NONE',  ( 4.082600654608392610, 21.41965916404854298, 13.00000000000000178 ) ) ;
#30828 = CARTESIAN_POINT ( 'NONE',  ( -15.43577743098634159, -26.72909887300547283, -5.000000000000000888 ) ) ;
#30829 = CARTESIAN_POINT ( 'NONE',  ( -37.03605016781039438, -10.92602907108566868, 13.92931973827882253 ) ) ;
#30830 = VECTOR ( 'NONE', #2973, 1000.000000000000114 ) ;
#30831 = CARTESIAN_POINT ( 'NONE',  ( -28.07145589138256270, -22.01881091388684197, -10.19667367662031054 ) ) ;
#30832 = CARTESIAN_POINT ( 'NONE',  ( -0.2799713375976506380, -20.99526500827598596, -24.41369975650612645 ) ) ;
#30833 = CARTESIAN_POINT ( 'NONE',  ( 12.95423034502591442, 20.61663634441624993, -18.50330793998235990 ) ) ;
#30834 = CARTESIAN_POINT ( 'NONE',  ( 20.50834976286951772, 11.43410818086181280, -13.90707920088669702 ) ) ;
#30835 = CARTESIAN_POINT ( 'NONE',  ( -1.653273178848928050E-15, 36.00000000000000711, 7.000000000000000000 ) ) ;
#30836 = CARTESIAN_POINT ( 'NONE',  ( -5.213701606270112698, 36.61873165587430634, -8.423533786119408617 ) ) ;
#30837 = ORIENTED_EDGE ( 'NONE', *, *, #19484, .F. ) ;
#30838 = CARTESIAN_POINT ( 'NONE',  ( -23.49268708087237201, -3.611016997205812373, -21.11844712770017907 ) ) ;
#30839 = CARTESIAN_POINT ( 'NONE',  ( -22.45707936798516968, 12.96560081831745670, 14.53008259254011136 ) ) ;
#30840 = ORIENTED_EDGE ( 'NONE', *, *, #25740, .T. ) ;
#30841 = FACE_BOUND ( 'NONE', #12369, .T. ) ;
#30842 = EDGE_CURVE ( 'NONE', #18489, #29040, #27596, .T. ) ;
#30843 = CARTESIAN_POINT ( 'NONE',  ( 21.92391373441417102, -15.64922772886939661, 23.00000000000000711 ) ) ;
#30844 = CARTESIAN_POINT ( 'NONE',  ( -30.25911448991262276, 0.6236314785230308022, -5.000000000000000000 ) ) ;
#30845 = CARTESIAN_POINT ( 'NONE',  ( 30.88550645483323009, -11.32616882505672784, -12.93498916185149028 ) ) ;
#30846 = AXIS2_PLACEMENT_3D ( 'NONE', #17096, #17901, #36179 ) ;
#30847 = ADVANCED_FACE ( 'NONE', ( #36349 ), #27202, .T. ) ;
#30848 = ORIENTED_EDGE ( 'NONE', *, *, #16868, .F. ) ;
#30849 = CARTESIAN_POINT ( 'NONE',  ( 4.458865582155095986, 18.48521636184714012, 13.00000000000000178 ) ) ;
#30850 = EDGE_LOOP ( 'NONE', ( #35222, #25019, #11705, #15847 ) ) ;
#30851 = ADVANCED_FACE ( 'NONE', ( #36149 ), #17676, .F. ) ;
#30852 = CARTESIAN_POINT ( 'NONE',  ( 11.11016527260166420, 31.83082137946473367, 9.000000000000001776 ) ) ;
#30853 = AXIS2_PLACEMENT_3D ( 'NONE', #6812, #25709, #10477 ) ;
#30854 = CARTESIAN_POINT ( 'NONE',  ( 33.75875814100320582, 2.759858869446452978, 11.00000000000000000 ) ) ;
#30855 = CIRCLE ( 'NONE', #1652, 15.00000000000000000 ) ;
#30856 = AXIS2_PLACEMENT_3D ( 'NONE', #8590, #36820, #15284 ) ;
#30857 = CARTESIAN_POINT ( 'NONE',  ( 13.95683075005237050, 28.08631143191933432, 10.50000000000000533 ) ) ;
#30858 = EDGE_LOOP ( 'NONE', ( #29562, #30980 ) ) ;
#30859 = CARTESIAN_POINT ( 'NONE',  ( -4.123717629018512021, 36.95811013929738920, -8.415836676720722664 ) ) ;
#30860 = CARTESIAN_POINT ( 'NONE',  ( -1.000000000000000888, 36.50000000000000711, 9.500000000000000000 ) ) ;
#30861 = DIRECTION ( 'NONE',  ( 1.000000000000000000, 0.000000000000000000, 0.000000000000000000 ) ) ;
#30862 = CARTESIAN_POINT ( 'NONE',  ( 3.161220354320216863, 12.43736188311278212, 10.49999999999999289 ) ) ;
#30863 = CARTESIAN_POINT ( 'NONE',  ( 28.01677963356848622, -22.94489307428302993, -9.311317233667166349 ) ) ;
#30864 = CARTESIAN_POINT ( 'NONE',  ( 19.75473557947194436, 14.68794674279743795, -9.387208291950921435 ) ) ;
#30865 = CARTESIAN_POINT ( 'NONE',  ( 11.34888309589563882, 25.00279730542691325, -16.12364529934884771 ) ) ;
#30866 = ORIENTED_EDGE ( 'NONE', *, *, #16849, .T. ) ;
#30867 = CARTESIAN_POINT ( 'NONE',  ( -17.90340069958895697, 10.65400709177240302, -25.51243598403177870 ) ) ;
#30868 = FACE_OUTER_BOUND ( 'NONE', #31183, .T. ) ;
#30869 = EDGE_CURVE ( 'NONE', #20339, #21746, #18414, .T. ) ;
#30870 = CARTESIAN_POINT ( 'NONE',  ( 11.63721313908758681, -20.96583099751724077, -19.48517461635267267 ) ) ;
#30871 = CYLINDRICAL_SURFACE ( 'NONE', #17838, 1.000000000000000000 ) ;
#30872 = CARTESIAN_POINT ( 'NONE',  ( -3.859759734048395785E-14, -22.74351282448223799, -30.00000000000000355 ) ) ;
#30873 = DIRECTION ( 'NONE',  ( 0.000000000000000000, 0.000000000000000000, 1.000000000000000000 ) ) ;
#30874 = CARTESIAN_POINT ( 'NONE',  ( -14.72734366533763506, 25.42720644217061832, -10.65114164413067677 ) ) ;
#30875 = CARTESIAN_POINT ( 'NONE',  ( -13.61442942725709315, -16.31983737738216433, -25.85608801652313460 ) ) ;
#30876 = CARTESIAN_POINT ( 'NONE',  ( 12.98099092732498683, -25.97363603336197357, -7.367975789372572137 ) ) ;
#30877 = DIRECTION ( 'NONE',  ( -0.4067366430757891060, 0.9135454576426058626, 1.734723475976806700E-15 ) ) ;
#30878 = ORIENTED_EDGE ( 'NONE', *, *, #32363, .T. ) ;
#30879 = CARTESIAN_POINT ( 'NONE',  ( -6.485893174894165725, 19.45725460019876252, -29.99999999999998224 ) ) ;
#30880 = CARTESIAN_POINT ( 'NONE',  ( -14.86556419889029534, 20.43481210330121556, 10.49999999999999822 ) ) ;
#30881 = CARTESIAN_POINT ( 'NONE',  ( -12.89070168820775386, 15.82735026918974341, 10.83333333333333037 ) ) ;
#30882 = CONICAL_SURFACE ( 'NONE', #28263, 0.5000000000000002220, 0.7853981633974524978 ) ;
#30883 = DIRECTION ( 'NONE',  ( -0.9945218953682745111, -0.1045284632676425907, 0.000000000000000000 ) ) ;
#30884 = VERTEX_POINT ( 'NONE', #24148 ) ;
#30885 = CARTESIAN_POINT ( 'NONE',  ( 30.68637370779745055, 0.009861439750234452309, -6.888001205752280143 ) ) ;
#30886 = DIRECTION ( 'NONE',  ( 0.000000000000000000, 0.000000000000000000, 1.000000000000000000 ) ) ;
#30887 = AXIS2_PLACEMENT_3D ( 'NONE', #4019, #25954, #16421 ) ;
#30888 = DIRECTION ( 'NONE',  ( 0.000000000000000000, 0.000000000000000000, 1.000000000000000000 ) ) ;
#30889 = ORIENTED_EDGE ( 'NONE', *, *, #11888, .F. ) ;
#30890 = CARTESIAN_POINT ( 'NONE',  ( -29.96087079451076818, 0.06295573032941799430, -9.238980554428115610 ) ) ;
#30891 = ADVANCED_FACE ( 'NONE', ( #9113 ), #18461, .T. ) ;
#30892 = DIRECTION ( 'NONE',  ( -0.000000000000000000, -0.000000000000000000, 1.000000000000000000 ) ) ;
#30893 = ORIENTED_EDGE ( 'NONE', *, *, #24059, .T. ) ;
#30894 = CARTESIAN_POINT ( 'NONE',  ( 30.54975010973276994, -5.406317539725979948, -13.10619709277712985 ) ) ;
#30895 = EDGE_LOOP ( 'NONE', ( #20333, #795, #28979 ) ) ;
#30896 = CARTESIAN_POINT ( 'NONE',  ( -9.166052203149666511, 37.72018303275904572, 13.32518128616555586 ) ) ;
#30897 = EDGE_CURVE ( 'NONE', #17512, #28635, #24552, .T. ) ;
#30898 = CARTESIAN_POINT ( 'NONE',  ( 5.938964939929074482, -16.21345324574345170, 20.82122704794080192 ) ) ;
#30899 = DIRECTION ( 'NONE',  ( 1.000000000000000000, 0.000000000000000000, 0.000000000000000000 ) ) ;
#30900 = CARTESIAN_POINT ( 'NONE',  ( 8.207473342610013489, 28.06734471880750093, 20.25080042701566896 ) ) ;
#30901 = DIRECTION ( 'NONE',  ( 0.000000000000000000, 0.000000000000000000, 1.000000000000000000 ) ) ;
#30902 = EDGE_LOOP ( 'NONE', ( #33943, #19979, #7699, #35701 ) ) ;
#30903 = FACE_OUTER_BOUND ( 'NONE', #1902, .T. ) ;
#30904 = CARTESIAN_POINT ( 'NONE',  ( -10.44103466624267185, 32.57396620494226624, 11.00000000000000000 ) ) ;
#30905 = CARTESIAN_POINT ( 'NONE',  ( 3.713592597587208832, 7.966960743906818188, 7.000000000000000000 ) ) ;
#30906 = VECTOR ( 'NONE', #38215, 1000.000000000000114 ) ;
#30907 = CARTESIAN_POINT ( 'NONE',  ( -3.724378136954612284, 12.76962061027129458, 13.00000000000000178 ) ) ;
#30908 = CARTESIAN_POINT ( 'NONE',  ( 4.496862015843432481, 20.00989232716073118, -30.00000000000000000 ) ) ;
#30909 = VECTOR ( 'NONE', #8033, 1000.000000000000000 ) ;
#30910 = CARTESIAN_POINT ( 'NONE',  ( 6.354454053420414361, 35.54304081427980577, 7.000000000000000000 ) ) ;
#30911 = VECTOR ( 'NONE', #10032, 1000.000000000000000 ) ;
#30912 = EDGE_CURVE ( 'NONE', #4851, #31336, #3017, .T. ) ;
#30913 = EDGE_CURVE ( 'NONE', #37715, #15690, #31369, .T. ) ;
#30914 = CARTESIAN_POINT ( 'NONE',  ( 15.14693761635412983, -23.74175418701464579, -14.31586175695692020 ) ) ;
#30915 = CARTESIAN_POINT ( 'NONE',  ( 8.306370210276320165, 9.993911548625739272, 10.49999999999999645 ) ) ;
#30916 = DIRECTION ( 'NONE',  ( 0.4067366430758010409, 0.9135454576426005335, -0.000000000000000000 ) ) ;
#30917 = CARTESIAN_POINT ( 'NONE',  ( 0.9028139003476853830, 37.47297129542256755, 7.381627713044571770 ) ) ;
#30918 = ORIENTED_EDGE ( 'NONE', *, *, #30284, .T. ) ;
#30919 = CARTESIAN_POINT ( 'NONE',  ( -14.14736404216506571, 23.66099997246980635, -13.52656865009267406 ) ) ;
#30920 = CARTESIAN_POINT ( 'NONE',  ( -29.39157470508739323, -22.49273609621608827, 17.42190598798392998 ) ) ;
#30921 = CARTESIAN_POINT ( 'NONE',  ( 13.13573601262098478, -23.60207374655375645, -14.48926436058232881 ) ) ;
#30922 = CARTESIAN_POINT ( 'NONE',  ( -4.002483478063582290, 8.479530061156673071, 10.49999999999999822 ) ) ;
#30923 = ORIENTED_EDGE ( 'NONE', *, *, #29321, .F. ) ;
#30924 = ORIENTED_EDGE ( 'NONE', *, *, #15295, .T. ) ;
#30925 = CARTESIAN_POINT ( 'NONE',  ( -13.81624380675895836, 30.37090005602236431, -6.364651089629193237 ) ) ;
#30926 = CARTESIAN_POINT ( 'NONE',  ( -20.14086777909864168, -26.69671822894133228, -8.145045410496569716 ) ) ;
#30927 =( BOUNDED_CURVE ( )  B_SPLINE_CURVE ( 2, ( #26311, #36062, #8627 ),
 .UNSPECIFIED., .F., .F. ) 
 B_SPLINE_CURVE_WITH_KNOTS ( ( 3, 3 ),
 ( 0.000000000000000000, 1.000000000000000000 ),
 .UNSPECIFIED. ) 
 CURVE ( )  GEOMETRIC_REPRESENTATION_ITEM ( )  RATIONAL_B_SPLINE_CURVE ( ( 1.000000000000000000, 0.7071067811865474617, 1.000000000000000000 ) ) 
 REPRESENTATION_ITEM ( '' )  );
#30928 = FACE_BOUND ( 'NONE', #11075, .T. ) ;
#30929 = ORIENTED_EDGE ( 'NONE', *, *, #34976, .T. ) ;
#30930 = CARTESIAN_POINT ( 'NONE',  ( -22.56600422072800782, -6.300902944093242475, -22.03183368421533928 ) ) ;
#30931 = CARTESIAN_POINT ( 'NONE',  ( -15.18562876168915565, -26.54301761587689867, -6.888309856460237413 ) ) ;
#30932 = CARTESIAN_POINT ( 'NONE',  ( -9.303655249773276736, 10.73386218874833631, 7.500000000000000888 ) ) ;
#30933 = ORIENTED_EDGE ( 'NONE', *, *, #3071, .F. ) ;
#30934 = CARTESIAN_POINT ( 'NONE',  ( 30.54320699650084947, 0.2260830151874697325, -6.417392023155034764 ) ) ;
#30935 = DIRECTION ( 'NONE',  ( 0.000000000000000000, 1.000000000000000000, 0.000000000000000000 ) ) ;
#30936 = CARTESIAN_POINT ( 'NONE',  ( 3.992867117591230919, 8.524771480177550487, 10.49999999999999289 ) ) ;
#30937 = VERTEX_POINT ( 'NONE', #11566 ) ;
#30938 = CARTESIAN_POINT ( 'NONE',  ( -29.83105174024096229, 0.01200203450569401441, -9.707336131520873934 ) ) ;
#30939 = EDGE_CURVE ( 'NONE', #1970, #18869, #5860, .T. ) ;
#30940 = VERTEX_POINT ( 'NONE', #39588 ) ;
#30941 = CARTESIAN_POINT ( 'NONE',  ( 22.47524216860800195, -0.4976999769275546881, -22.58728816505331949 ) ) ;
#30942 = CIRCLE ( 'NONE', #14081, 0.5000000000000004441 ) ;
#30943 = CYLINDRICAL_SURFACE ( 'NONE', #34964, 18.00000000000000000 ) ;
#30944 = CARTESIAN_POINT ( 'NONE',  ( 30.14286744058976453, -20.99504498967356270, 17.92354375535288824 ) ) ;
#30945 = ORIENTED_EDGE ( 'NONE', *, *, #1074, .F. ) ;
#30946 = CARTESIAN_POINT ( 'NONE',  ( -26.88094701073862325, 3.517601285915260334, -9.781306404757943440 ) ) ;
#30947 = LINE ( 'NONE', #15699, #8509 ) ;
#30948 = CYLINDRICAL_SURFACE ( 'NONE', #23898, 18.00000000000002487 ) ;
#30949 = CARTESIAN_POINT ( 'NONE',  ( 8.401171878996485987, 21.11424711454080594, 7.000000000000000000 ) ) ;
#30950 = CARTESIAN_POINT ( 'NONE',  ( -13.63581098909220479, 27.45627467658446008, 9.500000000000000000 ) ) ;
#30951 = FACE_BOUND ( 'NONE', #30769, .T. ) ;
#30952 = CARTESIAN_POINT ( 'NONE',  ( 19.89620541518914010, 17.40116461633694911, 14.53008259253988044 ) ) ;
#30953 = CARTESIAN_POINT ( 'NONE',  ( -22.10669899577159825, 7.630206710036005369, -15.88546095289416016 ) ) ;
#30954 = DIRECTION ( 'NONE',  ( 1.000000000000000000, 0.000000000000000000, 0.000000000000000000 ) ) ;
#30955 = DIRECTION ( 'NONE',  ( 1.000000000000000000, -6.938893903907197612E-15, 0.000000000000000000 ) ) ;
#30956 = CARTESIAN_POINT ( 'NONE',  ( 15.60359587640040679, -17.23679362701221152, -22.13449739431376884 ) ) ;
#30957 = DIRECTION ( 'NONE',  ( 0.6724985119639553810, -0.2185080122244117407, -0.7071067811865489050 ) ) ;
#30958 = EDGE_CURVE ( 'NONE', #15928, #4057, #18066, .T. ) ;
#30959 = CARTESIAN_POINT ( 'NONE',  ( 14.94231797702671471, 26.21208174917623523, -9.226265064744874067 ) ) ;
#30960 = AXIS2_PLACEMENT_3D ( 'NONE', #25232, #457, #12839 ) ;
#30961 = EDGE_LOOP ( 'NONE', ( #2559, #30499, #31955, #26347, #33188, #27363, #31637 ) ) ;
#30962 = CARTESIAN_POINT ( 'NONE',  ( -15.94479093369340106, 23.58249151255476406, -8.795490714381706709 ) ) ;
#30963 = CARTESIAN_POINT ( 'NONE',  ( -28.07442828530314216, -16.20877872786413576, 20.25080042701565830 ) ) ;
#30964 = CARTESIAN_POINT ( 'NONE',  ( -4.475131784526824141, 8.183115020678636498, 7.000000000000000000 ) ) ;
#30965 = CARTESIAN_POINT ( 'NONE',  ( 15.44165670342503205, 26.69129292160669920, -5.474180254959668090 ) ) ;
#30966 = ORIENTED_EDGE ( 'NONE', *, *, #36100, .F. ) ;
#30967 = CARTESIAN_POINT ( 'NONE',  ( 13.28503138821879581, 15.53523575316139649, 7.000000000000000000 ) ) ;
#30968 = ORIENTED_EDGE ( 'NONE', *, *, #19438, .F. ) ;
#30969 = AXIS2_PLACEMENT_3D ( 'NONE', #5053, #39177, #35937 ) ;
#30971 = DIRECTION ( 'NONE',  ( -0.6724985119639492748, 0.2185080122244156264, -0.7071067811865536790 ) ) ;
#30970 = CARTESIAN_POINT ( 'NONE',  ( -14.65347711145498444, 25.64673223685113612, -10.63691246398533430 ) ) ;
#30972 = CARTESIAN_POINT ( 'NONE',  ( -12.01613607123918648, -21.47750082395870663, -18.43867415038402768 ) ) ;
#30973 = CARTESIAN_POINT ( 'NONE',  ( -12.49038105676665644, 14.13397459621567798, 10.50000000000000000 ) ) ;
#30974 = VECTOR ( 'NONE', #33276, 1000.000000000000000 ) ;
#30975 = VERTEX_POINT ( 'NONE', #14612 ) ;
#30976 = CARTESIAN_POINT ( 'NONE',  ( -24.72872997693725949, -12.95474267484971698, -17.60025526371827098 ) ) ;
#30977 = CARTESIAN_POINT ( 'NONE',  ( -13.85493750717612471, -26.22870991353853753, -6.891751044494506928 ) ) ;
#30978 = CARTESIAN_POINT ( 'NONE',  ( 1.525645716490520387, 8.212903943950921715, 7.000000000000000000 ) ) ;
#30979 = CARTESIAN_POINT ( 'NONE',  ( 15.59579652599576782, 23.45568014046210337, -10.22222026387747107 ) ) ;
#30980 = ORIENTED_EDGE ( 'NONE', *, *, #15452, .T. ) ;
#30981 = CARTESIAN_POINT ( 'NONE',  ( 26.01521168343815305, 5.578082495604143709, -5.477568960753655958 ) ) ;
#30982 = DIRECTION ( 'NONE',  ( 0.000000000000000000, 0.000000000000000000, 1.000000000000000000 ) ) ;
#30983 = DIRECTION ( 'NONE',  ( -0.1045284632676566766, -0.9945218953682730678, 0.000000000000000000 ) ) ;
#30984 = FACE_OUTER_BOUND ( 'NONE', #21942, .T. ) ;
#30985 = ORIENTED_EDGE ( 'NONE', *, *, #4164, .F. ) ;
#30986 = CARTESIAN_POINT ( 'NONE',  ( -30.25735003896744857, -0.2604941155819015530, -9.220310513660999518 ) ) ;
#30987 = ADVANCED_FACE ( 'NONE', ( #36750, #15008 ), #30460, .T. ) ;
#30988 = CARTESIAN_POINT ( 'NONE',  ( 20.70339734419210131, 0.6992704487685735826, -27.43878474189266115 ) ) ;
#30989 = CARTESIAN_POINT ( 'NONE',  ( 1.278175571583998860, 14.08178954835375940, 7.000000000000000000 ) ) ;
#30990 = EDGE_CURVE ( 'NONE', #15434, #16182, #6079, .T. ) ;
#30991 = CARTESIAN_POINT ( 'NONE',  ( 24.79273775960278314, -6.040746354376016924, 20.82122704794079837 ) ) ;
#30992 = ORIENTED_EDGE ( 'NONE', *, *, #26995, .T. ) ;
#30993 = CARTESIAN_POINT ( 'NONE',  ( 37.49625565938770677, -14.69322820095495530, -14.45070082761205832 ) ) ;
#30994 = DIRECTION ( 'NONE',  ( 1.000000000000000000, 0.000000000000000000, 0.000000000000000000 ) ) ;
#30995 = AXIS2_PLACEMENT_3D ( 'NONE', #6927, #32338, #35177 ) ;
#30996 = VECTOR ( 'NONE', #36483, 1000.000000000000000 ) ;
#30997 = EDGE_CURVE ( 'NONE', #15842, #19485, #16470, .T. ) ;
#30998 = ORIENTED_EDGE ( 'NONE', *, *, #11386, .T. ) ;
#30999 = B_SPLINE_CURVE_WITH_KNOTS ( 'NONE', 3,
 ( #3080, #28260, #6910, #30917, #21758, #37801, #12420, #6120 ),
 .UNSPECIFIED., .F., .F.,
 ( 4, 2, 2, 4 ),
 ( 0.000000000000000000, 0.0002364868538934269395, 0.0004729737077868538791, 0.0009459474155737077582 ),
 .UNSPECIFIED. ) ;
#31000 = FACE_OUTER_BOUND ( 'NONE', #20293, .T. ) ;
#31001 = AXIS2_PLACEMENT_3D ( 'NONE', #21449, #25091, #40131 ) ;
#31002 = AXIS2_PLACEMENT_3D ( 'NONE', #8144, #23786, #5694 ) ;
#31003 = CARTESIAN_POINT ( 'NONE',  ( -5.064571727552472424, 31.45661825943146894, 13.00000000000000178 ) ) ;
#31004 = DIRECTION ( 'NONE',  ( 0.000000000000000000, 0.000000000000000000, 1.000000000000000000 ) ) ;
#31005 = CARTESIAN_POINT ( 'NONE',  ( 2.666049144303739293, 36.98651336572240922, -8.847562779496046304 ) ) ;
#31006 = FACE_OUTER_BOUND ( 'NONE', #30307, .T. ) ;
#31007 = CARTESIAN_POINT ( 'NONE',  ( 14.75678334372855538, 20.44624543189430099, 10.82238861112334760 ) ) ;
#31008 = LINE ( 'NONE', #28151, #16853 ) ;
#31009 = EDGE_CURVE ( 'NONE', #13548, #12651, #22287, .T. ) ;
#31010 = CARTESIAN_POINT ( 'NONE',  ( 9.665073660139013256, 25.11464168560187460, 10.50000000000000533 ) ) ;
#31011 = CARTESIAN_POINT ( 'NONE',  ( 10.78893975237932956, 23.27376113029817617, 13.00000000000000178 ) ) ;
#31012 = DIRECTION ( 'NONE',  ( -0.5877852522924807976, -0.8090169943749417891, 0.000000000000000000 ) ) ;
#31013 = ADVANCED_FACE ( 'NONE', ( #19244 ), #19445, .F. ) ;
#31014 = CARTESIAN_POINT ( 'NONE',  ( 13.93706817763407457, 25.34829717239110991, -12.47786359530666900 ) ) ;
#31015 = CARTESIAN_POINT ( 'NONE',  ( -12.77091082532341382, 29.60251629318183575, 6.000000000000000000 ) ) ;
#31016 = ORIENTED_EDGE ( 'NONE', *, *, #20636, .T. ) ;
#31018 = DIRECTION ( 'NONE',  ( 0.000000000000000000, 0.000000000000000000, 1.000000000000000000 ) ) ;
#31017 = CARTESIAN_POINT ( 'NONE',  ( -17.52995626189967737, 16.16943778198609749, -14.84323570916496493 ) ) ;
#31019 = CARTESIAN_POINT ( 'NONE',  ( 11.87435565298210882, 15.06698729810772619, 7.499999999999997335 ) ) ;
#31020 = CARTESIAN_POINT ( 'NONE',  ( 15.38694898889602136, -26.59324455761997896, -6.887897242969529543 ) ) ;
#31021 = CARTESIAN_POINT ( 'NONE',  ( -21.59438778490832789, -27.03632430179366963, -6.341461391377428924 ) ) ;
#31022 = CARTESIAN_POINT ( 'NONE',  ( 14.73787879266531853, 25.39503920881752208, -10.65324680268566127 ) ) ;
#31023 = CARTESIAN_POINT ( 'NONE',  ( 10.98733276423893201, 17.36017109950246251, -28.70617518134429602 ) ) ;
#31024 = EDGE_LOOP ( 'NONE', ( #28888, #13629, #28237, #28869 ) ) ;
#31025 = DIRECTION ( 'NONE',  ( 0.000000000000000000, 0.000000000000000000, 1.000000000000000000 ) ) ;
#31026 = CARTESIAN_POINT ( 'NONE',  ( -11.45863972089735405, -20.98773559138341227, -19.50614846912421996 ) ) ;
#31027 = CARTESIAN_POINT ( 'NONE',  ( -33.17211272335762118, -21.25822893968250327, 15.13084544680185850 ) ) ;
#31028 = VECTOR ( 'NONE', #19237, 1000.000000000000000 ) ;
#31029 = CIRCLE ( 'NONE', #18069, 1.000000000000000000 ) ;
#31030 = CARTESIAN_POINT ( 'NONE',  ( -29.70672294952053250, -21.88546735577168789, -8.854887924351043438 ) ) ;
#31031 = CARTESIAN_POINT ( 'NONE',  ( -2.582945274031032579, -24.71752041314383774, -6.939050857786467574 ) ) ;
#31032 = CARTESIAN_POINT ( 'NONE',  ( 12.38854343360681654, 19.61926878829738996, -20.58590829373904540 ) ) ;
#31033 = CARTESIAN_POINT ( 'NONE',  ( 22.57201939060207252, 10.08208122992440003, -8.403798546843612272 ) ) ;
#31034 = DIRECTION ( 'NONE',  ( 0.8090169943749504489, 0.5877852522924690293, -0.000000000000000000 ) ) ;
#31035 = CARTESIAN_POINT ( 'NONE',  ( -2.937749330471188358, 20.92723910012711031, -26.29585176386288126 ) ) ;
#31036 = VECTOR ( 'NONE', #12056, 1000.000000000000000 ) ;
#31037 = VERTEX_POINT ( 'NONE', #16207 ) ;
#31038 = B_SPLINE_CURVE_WITH_KNOTS ( 'NONE', 3,
 ( #1660, #11007, #29684, #36187, #32945, #5103, #29882, #14440, #23392, #35787, #7941, #26835, #8354, #39226, #11405, #23788, #27039, #28232 ),
 .UNSPECIFIED., .F., .F.,
 ( 4, 2, 2, 2, 2, 2, 2, 2, 4 ),
 ( 0.000000000000000000, 0.08767823854539483208, 0.1753564770907896642, 0.2630347156361845240, 0.3507129541815793283, 0.4383911927269741327, 0.5260694312723690480, 0.6137476698177638523, 0.7014259083631586567 ),
 .UNSPECIFIED. ) ;
#31039 = CARTESIAN_POINT ( 'NONE',  ( -34.60931334941528803, -6.532660442264273115, -6.767915967295159874 ) ) ;
#31040 = ADVANCED_FACE ( 'NONE', ( #40185 ), #18660, .F. ) ;
#31041 = AXIS2_PLACEMENT_3D ( 'NONE', #8547, #15040, #33350 ) ;
#31042 = CARTESIAN_POINT ( 'NONE',  ( -18.85374159600211641, 16.91074157332653982, 16.30093088680128233 ) ) ;
#31043 = EDGE_LOOP ( 'NONE', ( #28473, #20525, #24891, #1217 ) ) ;
#31044 = EDGE_CURVE ( 'NONE', #34387, #22937, #31052, .T. ) ;
#31045 = CARTESIAN_POINT ( 'NONE',  ( -1.278175571584109660, 14.08178954835378427, 7.000000000000000000 ) ) ;
#31046 = CYLINDRICAL_SURFACE ( 'NONE', #38821, 1.000000000000000000 ) ;
#31047 = CARTESIAN_POINT ( 'NONE',  ( -22.56602591100718769, 1.155315371689267012, -21.68362715205212155 ) ) ;
#31048 = CARTESIAN_POINT ( 'NONE',  ( 32.45817255219479591, -13.02753558049290561, -11.09164157653418847 ) ) ;
#31049 = ORIENTED_EDGE ( 'NONE', *, *, #337, .T. ) ;
#31050 = FACE_OUTER_BOUND ( 'NONE', #1986, .T. ) ;
#31051 = EDGE_LOOP ( 'NONE', ( #10759, #15530 ) ) ;
#31052 = LINE ( 'NONE', #18855, #11286 ) ;
#31053 = CARTESIAN_POINT ( 'NONE',  ( 30.33922525716342733, 6.243664897651060919, 23.00000000003197798 ) ) ;
#31054 = CIRCLE ( 'NONE', #1216, 1.000000000000000888 ) ;
#31055 = LINE ( 'NONE', #30857, #38277 ) ;
#31056 = ORIENTED_EDGE ( 'NONE', *, *, #37830, .T. ) ;
#31057 = CARTESIAN_POINT ( 'NONE',  ( -3.698881800131589070, 33.04102055638166746, -12.90738243435495747 ) ) ;
#31058 = CARTESIAN_POINT ( 'NONE',  ( -9.221287281574667816, 10.65863771052209863, 10.49999999999999822 ) ) ;
#31059 = CARTESIAN_POINT ( 'NONE',  ( 13.14827996435953494, 25.72067290776660897, 9.500000000000000000 ) ) ;
#31060 = AXIS2_PLACEMENT_3D ( 'NONE', #10662, #16763, #29750 ) ;
#31061 = CARTESIAN_POINT ( 'NONE',  ( 13.49038105676655164, 15.86602540378438064, 11.00000000000000000 ) ) ;
#31062 = CARTESIAN_POINT ( 'NONE',  ( 16.59050531452238175, -12.72231626870975774, -26.99548381761250937 ) ) ;
#31063 = CARTESIAN_POINT ( 'NONE',  ( 15.77861697390694395, 13.11959191132365099, -28.84590463088538570 ) ) ;
#31064 = CARTESIAN_POINT ( 'NONE',  ( 11.41068916750651674, 27.22167306763704175, -14.12609294827662154 ) ) ;
#31065 = VERTEX_POINT ( 'NONE', #12751 ) ;
#31066 = CARTESIAN_POINT ( 'NONE',  ( -19.48170590106686717, 10.58249606826150035, -19.06244706679226297 ) ) ;
#31067 = CARTESIAN_POINT ( 'NONE',  ( -8.007761790012255076, 9.776959832083379709, 11.00000000000000000 ) ) ;
#31068 = CARTESIAN_POINT ( 'NONE',  ( 14.53923885275054495, -25.10454186404201238, -11.58604102348432896 ) ) ;
#31069 = FACE_OUTER_BOUND ( 'NONE', #3697, .T. ) ;
#31070 = ADVANCED_FACE ( 'NONE', ( #3217 ), #3408, .F. ) ;
#31071 = CARTESIAN_POINT ( 'NONE',  ( 7.289639608743136989, -27.06962010326278545, -13.42901749168595593 ) ) ;
#31072 = CARTESIAN_POINT ( 'NONE',  ( -12.39464589777671044, 26.66807349098043289, 12.00000000000000000 ) ) ;
#31073 = CARTESIAN_POINT ( 'NONE',  ( -15.32247945677889334, 26.67302399322529283, -6.886783351072488735 ) ) ;
#31074 = CARTESIAN_POINT ( 'NONE',  ( -19.96046382237359751, -23.75384511009722033, -13.10646546221969544 ) ) ;
#31075 = CARTESIAN_POINT ( 'NONE',  ( 8.289791691739285540, -18.78981145098772387, -28.75044738397058808 ) ) ;
#31076 = CARTESIAN_POINT ( 'NONE',  ( 18.89841941734945152, -12.77170018320259182, -23.00035857315318921 ) ) ;
#31077 = CARTESIAN_POINT ( 'NONE',  ( 5.644276917315955266, 36.40655018617680838, 10.59344459855566534 ) ) ;
#31078 = EDGE_LOOP ( 'NONE', ( #9559, #27491, #9448, #5052, #37414, #34072, #26276, #5306, #4704, #7449, #31837, #29162, #22354, #24133, #37796, #31056, #28911, #7378, #23685, #8753, #19210, #33903, #24522, #13179, #38217, #20559, #27769, #26989, #10293, #17094, #1996, #23858, #28282, #12157, #24934, #20940, #12748, #11851, #31512, #32707, #32305, #27595, #3662, #14375, #33576, #9888 ) ) ;
#31079 = CARTESIAN_POINT ( 'NONE',  ( -11.13950323990193603, 33.98129016598238650, -5.885180931403255933 ) ) ;
#31080 = FACE_OUTER_BOUND ( 'NONE', #11285, .T. ) ;
#31081 = DIRECTION ( 'NONE',  ( 0.000000000000000000, 0.000000000000000000, 1.000000000000000000 ) ) ;
#31082 = AXIS2_PLACEMENT_3D ( 'NONE', #11741, #17449, #2006 ) ;
#31083 = AXIS2_PLACEMENT_3D ( 'NONE', #5435, #33082, #5031 ) ;
#31084 = LINE ( 'NONE', #30686, #6590 ) ;
#31085 = VERTEX_POINT ( 'NONE', #37544 ) ;
#31086 = CARTESIAN_POINT ( 'NONE',  ( 28.33402286304662709, 0.1460920933068121652, -12.55056911448999379 ) ) ;
#31087 = CARTESIAN_POINT ( 'NONE',  ( 15.41558956984165363, 26.78481017248027740, -5.000000000000000000 ) ) ;
#31088 = CARTESIAN_POINT ( 'NONE',  ( -1.829593030691901284E-15, 22.50000000000001066, 0.000000000000000000 ) ) ;
#31089 = AXIS2_PLACEMENT_3D ( 'NONE', #5712, #14662, #2275 ) ;
#31090 = B_SPLINE_SURFACE_WITH_KNOTS ( 'NONE', 1, 3, ( 
 ( #790, #22320, #13173, #25568, #12976, #28418, #9741, #594, #39665, #22123 ),
 ( #28218, #398, #37767, #19079, #39858, #22514, #34924, #36818, #25366, #12779 ) ),
 .UNSPECIFIED., .F., .F., .F.,
 ( 2, 2 ),
 ( 4, 2, 2, 2, 4 ),
 ( 0.000000000000000000, 1.000000000000000000 ),
 ( 1.796630036486493109, 2.189329118185220580, 2.582028199883947828, 2.974727281582675076, 3.367426363281402768 ),
 .UNSPECIFIED. ) ;
#31091 = VERTEX_POINT ( 'NONE', #25144 ) ;
#31092 = CARTESIAN_POINT ( 'NONE',  ( -30.56608372293882780, 0.03382379541455289573, -7.358089190805260138 ) ) ;
#31093 = LINE ( 'NONE', #21539, #32628 ) ;
#31094 = ORIENTED_EDGE ( 'NONE', *, *, #11585, .T. ) ;
#31095 = CARTESIAN_POINT ( 'NONE',  ( 21.32230761661163143, -4.380135932481430849, -24.50474909882916918 ) ) ;
#31096 = VERTEX_POINT ( 'NONE', #21894 ) ;
#31097 = CARTESIAN_POINT ( 'NONE',  ( 12.20958131808574798, 35.40723086407815856, 13.32518128616605324 ) ) ;
#31098 = ADVANCED_FACE ( 'NONE', ( #34689 ), #31838, .T. ) ;
#31099 = DIRECTION ( 'NONE',  ( 0.000000000000000000, 0.000000000000000000, 1.000000000000000000 ) ) ;
#31100 = CARTESIAN_POINT ( 'NONE',  ( -1.000000000000000000, 37.50000000000000711, 7.000000000000000000 ) ) ;
#31101 = CARTESIAN_POINT ( 'NONE',  ( -6.000734348601507229, 30.39614672895594438, 20.25080042701566541 ) ) ;
#31102 = FACE_OUTER_BOUND ( 'NONE', #8183, .T. ) ;
#31103 = VERTEX_POINT ( 'NONE', #15407 ) ;
#31104 = CARTESIAN_POINT ( 'NONE',  ( 3.542977516905554847, 8.236468469132553594, 10.96580508970283141 ) ) ;
#31105 = DIRECTION ( 'NONE',  ( 0.000000000000000000, 0.000000000000000000, 1.000000000000000000 ) ) ;
#31106 = CARTESIAN_POINT ( 'NONE',  ( -13.01838097023000707, 23.73363068877903359, 13.00000000000000178 ) ) ;
#31107 = CARTESIAN_POINT ( 'NONE',  ( 13.77067693704748308, 28.44713853003850801, 7.000000000000000000 ) ) ;
#31109 = AXIS2_PLACEMENT_3D ( 'NONE', #22243, #326, #37501 ) ;
#31108 = CARTESIAN_POINT ( 'NONE',  ( 8.739825649919259476, 33.88938738370909931, -9.801802266497743332 ) ) ;
#31110 = ADVANCED_FACE ( 'NONE', ( #28590 ), #12556, .F. ) ;
#31111 = CARTESIAN_POINT ( 'NONE',  ( 17.32315637682313536, -26.79968999324490753, -7.764865353756197131 ) ) ;
#31112 = CARTESIAN_POINT ( 'NONE',  ( -7.929471891321299815, 25.60217271033470965, 9.000000000000001776 ) ) ;
#31113 = CARTESIAN_POINT ( 'NONE',  ( -12.74038105676665289, 14.56698729810790027, 10.49999999999999822 ) ) ;
#31114 = EDGE_CURVE ( 'NONE', #10357, #28074, #4779, .T. ) ;
#31115 = ORIENTED_EDGE ( 'NONE', *, *, #3618, .F. ) ;
#31116 = CARTESIAN_POINT ( 'NONE',  ( -12.41574746403112073, 20.45786098935373687, -19.50078492736341573 ) ) ;
#31117 = CARTESIAN_POINT ( 'NONE',  ( -15.74227866054087066, -25.75916161678338412, 17.42190598798392642 ) ) ;
#31118 = CARTESIAN_POINT ( 'NONE',  ( 13.78902572764358503, -24.57398664863276139, -12.55976489257005646 ) ) ;
#31119 = EDGE_CURVE ( 'NONE', #15928, #17936, #35291, .T. ) ;
#31120 = CARTESIAN_POINT ( 'NONE',  ( 4.003793312560324225, 8.307369216259063549, 10.49999999999999645 ) ) ;
#31121 = EDGE_CURVE ( 'NONE', #35485, #11948, #22929, .T. ) ;
#31122 = ORIENTED_EDGE ( 'NONE', *, *, #13984, .T. ) ;
#31123 = ORIENTED_EDGE ( 'NONE', *, *, #2643, .T. ) ;
#31124 = CARTESIAN_POINT ( 'NONE',  ( -9.599378963044831181, 18.58950176588487224, -26.68917543542165305 ) ) ;
#31125 = CARTESIAN_POINT ( 'NONE',  ( -12.96962488765257859, -18.70490450770867596, -22.42242649434588486 ) ) ;
#31126 = FACE_BOUND ( 'NONE', #23649, .T. ) ;
#31127 = VERTEX_POINT ( 'NONE', #34297 ) ;
#31128 = CARTESIAN_POINT ( 'NONE',  ( -31.02555858839200553, -8.613196645477771085, -12.99421017137874479 ) ) ;
#31129 = CARTESIAN_POINT ( 'NONE',  ( -9.680704677217148557, -18.61067064102984148, -26.23473070599376911 ) ) ;
#31130 = CARTESIAN_POINT ( 'NONE',  ( 35.27625572565171552, 1.213838575767202776, 11.00000000000000000 ) ) ;
#31131 = ORIENTED_EDGE ( 'NONE', *, *, #19715, .F. ) ;
#31132 = CARTESIAN_POINT ( 'NONE',  ( 30.24006331749171039, 0.2466258206598069269, -7.829658031761377757 ) ) ;
#31133 = DIRECTION ( 'NONE',  ( 0.000000000000000000, 0.000000000000000000, 1.000000000000000000 ) ) ;
#31134 = CARTESIAN_POINT ( 'NONE',  ( -6.706342468480190000, 20.64589803375067945, 6.000000000000000000 ) ) ;
#31135 = ORIENTED_EDGE ( 'NONE', *, *, #5610, .T. ) ;
#31136 = CARTESIAN_POINT ( 'NONE',  ( -20.81788500015936805, 0.8029186697791972360, -26.82846150896363469 ) ) ;
#31137 = VERTEX_POINT ( 'NONE', #3806 ) ;
#31138 = CARTESIAN_POINT ( 'NONE',  ( 23.12890676149806168, -0.9096562629385716026, -21.41733200613340315 ) ) ;
#31139 = CIRCLE ( 'NONE', #36336, 0.4999999999999988898 ) ;
#31140 = APPLICATION_CONTEXT ( 'automotive_design' ) ;
#31141 = CARTESIAN_POINT ( 'NONE',  ( 21.91981567634946870, -15.65087685632042103, 20.99999999999999289 ) ) ;
#31142 = CARTESIAN_POINT ( 'NONE',  ( 23.60877407455211596, -25.08990816561031778, 17.92354375535291666 ) ) ;
#31143 = ADVANCED_FACE ( 'NONE', ( #27993 ), #37936, .T. ) ;
#31144 = ORIENTED_EDGE ( 'NONE', *, *, #36568, .F. ) ;
#31145 = CARTESIAN_POINT ( 'NONE',  ( -25.89993925104446504, 4.384403972809999495, -10.77364034502635093 ) ) ;
#31146 = EDGE_CURVE ( 'NONE', #22179, #36577, #34497, .T. ) ;
#31147 = AXIS2_PLACEMENT_3D ( 'NONE', #15409, #8919, #34301 ) ;
#31148 = CARTESIAN_POINT ( 'NONE',  ( 5.440908595777814050, 35.94977745735560859, 9.000000000000001776 ) ) ;
#31149 = CARTESIAN_POINT ( 'NONE',  ( 14.36830325120613239, 20.48707633493483371, 7.000000000000000000 ) ) ;
#31150 = CARTESIAN_POINT ( 'NONE',  ( 3.399837471815457590, 8.909889435135580626, 7.499999999999991118 ) ) ;
#31151 = CARTESIAN_POINT ( 'NONE',  ( -8.927394655428429360, 11.06314620770957013, 11.00000000000000000 ) ) ;
#31152 = DIRECTION ( 'NONE',  ( 1.000000000000000000, 0.000000000000000000, 0.000000000000000000 ) ) ;
#31153 = CARTESIAN_POINT ( 'NONE',  ( 16.81416712650777256, 27.17354907311674950, 13.92931973827808712 ) ) ;
#31154 = CARTESIAN_POINT ( 'NONE',  ( -20.37168883225173843, 6.509893064140952923, -23.23508475207167834 ) ) ;
#31155 = DIRECTION ( 'NONE',  ( 0.000000000000000000, 0.000000000000000000, 1.000000000000000000 ) ) ;
#31156 = LINE ( 'NONE', #9221, #33097 ) ;
#31157 = CARTESIAN_POINT ( 'NONE',  ( 23.01790674491153155, -26.73296861964898241, -6.329011521549396946 ) ) ;
#31158 = CARTESIAN_POINT ( 'NONE',  ( -12.53024597560957787, 27.62278594035707613, 10.50000000000000000 ) ) ;
#31159 = EDGE_CURVE ( 'NONE', #27076, #4088, #6259, .T. ) ;
#31160 = CARTESIAN_POINT ( 'NONE',  ( 11.49726645599677077, 19.09130336471316980, -22.70238085401357253 ) ) ;
#31161 = ORIENTED_EDGE ( 'NONE', *, *, #22087, .F. ) ;
#31162 = CARTESIAN_POINT ( 'NONE',  ( -15.60095462958403978, 23.83721962407788908, -9.740729558853310266 ) ) ;
#31163 = CARTESIAN_POINT ( 'NONE',  ( -22.09885373566634925, -20.02268770624659311, 20.50957957746052074 ) ) ;
#31164 = DIRECTION ( 'NONE',  ( 1.000000000000000000, 0.000000000000000000, 0.000000000000000000 ) ) ;
#31165 = CARTESIAN_POINT ( 'NONE',  ( 11.06517245712214859, 17.40842300371218698, -28.07890772714004868 ) ) ;
#31166 = ORIENTED_EDGE ( 'NONE', *, *, #9771, .T. ) ;
#31167 = DIRECTION ( 'NONE',  ( -0.2079116908177663647, -0.9781476007338042455, 0.000000000000000000 ) ) ;
#31168 = ORIENTED_EDGE ( 'NONE', *, *, #1523, .F. ) ;
#31170 = DIRECTION ( 'NONE',  ( 1.000000000000000000, 0.000000000000000000, 0.000000000000000000 ) ) ;
#31169 = CARTESIAN_POINT ( 'NONE',  ( -15.33616239741719234, 27.06134930142311745, -5.000000000000000888 ) ) ;
#31171 = CARTESIAN_POINT ( 'NONE',  ( -15.68099505712324060, -26.76486360534729414, -5.943857969596352042 ) ) ;
#31172 = LINE ( 'NONE', #16536, #30911 ) ;
#31173 = ORIENTED_EDGE ( 'NONE', *, *, #33022, .T. ) ;
#31174 = CARTESIAN_POINT ( 'NONE',  ( -34.19171386303132465, -16.60390462771976416, -7.120391363458460354 ) ) ;
#31175 = CARTESIAN_POINT ( 'NONE',  ( -8.172265125310115508, -20.22694128226171273, -23.00038051252499116 ) ) ;
#31176 = DIRECTION ( 'NONE',  ( 0.6916548014802308408, 0.1470157664651821627, 0.7071067811865456854 ) ) ;
#31177 = CARTESIAN_POINT ( 'NONE',  ( 16.47653236464018889, 23.28601002705642742, -5.949066710759219667 ) ) ;
#31178 = ORIENTED_EDGE ( 'NONE', *, *, #29670, .T. ) ;
#31179 = CARTESIAN_POINT ( 'NONE',  ( 25.05645393585312064, 4.615297387997106426, -12.74457131153767619 ) ) ;
#31180 = DIRECTION ( 'NONE',  ( -0.000000000000000000, -0.000000000000000000, -1.000000000000000000 ) ) ;
#31181 = FACE_OUTER_BOUND ( 'NONE', #35963, .T. ) ;
#31182 = DIRECTION ( 'NONE',  ( -0.9781476007338069101, -0.2079116908177532363, 0.000000000000000000 ) ) ;
#31183 = EDGE_LOOP ( 'NONE', ( #34567, #11011, #28119, #5859, #15285 ) ) ;
#31184 = CARTESIAN_POINT ( 'NONE',  ( -29.60645268812572084, -0.2125446482488342892, -10.63052326569164663 ) ) ;
#31185 = CARTESIAN_POINT ( 'NONE',  ( 30.41973907439335534, -0.2412478344116361639, -8.753233025701321779 ) ) ;
#31186 = CIRCLE ( 'NONE', #5862, 1.000000000000000888 ) ;
#31187 = CARTESIAN_POINT ( 'NONE',  ( 26.87422832650572602, -16.65342898056121257, 20.50957957746029336 ) ) ;
#31188 = CONICAL_SURFACE ( 'NONE', #28596, 0.4999999999999970024, 0.7853981633974447263 ) ;
#31189 = EDGE_LOOP ( 'NONE', ( #738, #7994, #14001 ) ) ;
#31190 = EDGE_CURVE ( 'NONE', #35341, #22029, #22487, .T. ) ;
#31191 = CARTESIAN_POINT ( 'NONE',  ( -17.81784622497958281, -13.85677843414106292, -19.80438750953545579 ) ) ;
#31192 = CARTESIAN_POINT ( 'NONE',  ( 13.32151712420403555, 20.09434385051835292, 10.50000000000000000 ) ) ;
#31193 = EDGE_LOOP ( 'NONE', ( #36530, #37015, #29961, #1854 ) ) ;
#31194 = AXIS2_PLACEMENT_3D ( 'NONE', #38596, #19913, #10770 ) ;
#31195 = DIRECTION ( 'NONE',  ( 0.000000000000000000, 0.000000000000000000, 1.000000000000000000 ) ) ;
#31196 = FACE_OUTER_BOUND ( 'NONE', #1804, .T. ) ;
#31197 = CARTESIAN_POINT ( 'NONE',  ( 14.09933648065468503, 26.02968990214155198, 10.50000000000000533 ) ) ;
#31198 = CARTESIAN_POINT ( 'NONE',  ( 1.827785273732315696, 25.64871398411360559, -19.64121285127799865 ) ) ;
#31199 = CARTESIAN_POINT ( 'NONE',  ( -6.354454053420242943, 35.54304081427989814, 11.00000000000000000 ) ) ;
#31200 = CARTESIAN_POINT ( 'NONE',  ( 10.41267482483262619, 26.20820393249957192, 12.00000000000000000 ) ) ;
#31201 = DIRECTION ( 'NONE',  ( -0.3583679495453109265, -0.9335804264971976352, 5.551115123125782702E-17 ) ) ;
#31202 = PLANE ( 'NONE',  #38094 ) ;
#31203 = DIRECTION ( 'NONE',  ( 0.5877852522924796874, 0.8090169943749426773, -0.000000000000000000 ) ) ;
#31204 = EDGE_CURVE ( 'NONE', #20904, #19280, #22290, .T. ) ;
#31205 = DIRECTION ( 'NONE',  ( 1.000000000000000000, 0.000000000000000000, 0.000000000000000000 ) ) ;
#31206 = CARTESIAN_POINT ( 'NONE',  ( 14.98678706335186028, 28.02796269202450929, -5.933300154731170117 ) ) ;
#31207 = DIRECTION ( 'NONE',  ( 0.000000000000000000, 0.000000000000000000, -1.000000000000000000 ) ) ;
#31208 = EDGE_LOOP ( 'NONE', ( #19925, #33111, #8394, #5892, #34459, #26059, #7513 ) ) ;
#31209 = CIRCLE ( 'NONE', #705, 0.4999999999999986122 ) ;
#31211 = CARTESIAN_POINT ( 'NONE',  ( -5.490944681523145299, 34.83286367817517259, 7.000000000000000000 ) ) ;
#31210 = CARTESIAN_POINT ( 'NONE',  ( -15.63638767905510463, 15.05447610871748232, -22.11642785074873174 ) ) ;
#31212 = DIRECTION ( 'NONE',  ( 0.9945218953682729568, -0.1045284632676569958, 0.000000000000000000 ) ) ;
#31213 = ADVANCED_FACE ( 'NONE', ( #20061 ), #38538, .T. ) ;
#31214 = VECTOR ( 'NONE', #9612, 1000.000000000000000 ) ;
#31215 = CARTESIAN_POINT ( 'NONE',  ( 12.25532247806346930, -22.02373625454399786, -17.44060027023390091 ) ) ;
#31216 = CARTESIAN_POINT ( 'NONE',  ( -15.74452436455642967, -19.93752133503633317, -19.02658665625699896 ) ) ;
#31217 = CARTESIAN_POINT ( 'NONE',  ( 11.12593219165437652, 17.61232244839224492, -26.83050114061178704 ) ) ;
#31218 = CARTESIAN_POINT ( 'NONE',  ( 11.29390759324882509, 18.05061880014659792, -25.01236529811382781 ) ) ;
#31219 = ORIENTED_EDGE ( 'NONE', *, *, #35003, .T. ) ;
#31220 = DIRECTION ( 'NONE',  ( 1.000000000000000000, 0.000000000000000000, 0.000000000000000000 ) ) ;
#31221 = CARTESIAN_POINT ( 'NONE',  ( -13.27830748821643425, -23.61430804126850092, -14.48142061928604818 ) ) ;
#31222 = CARTESIAN_POINT ( 'NONE',  ( -35.62872793493689727, -3.428732413881794727, 12.14047268033097460 ) ) ;
#31223 = ADVANCED_FACE ( 'NONE', ( #13549 ), #26348, .F. ) ;
#31224 = CARTESIAN_POINT ( 'NONE',  ( -30.48519299957962048, -21.05274509396561555, -8.849016827759179193 ) ) ;
#31225 = CARTESIAN_POINT ( 'NONE',  ( -0.3766544288610457758, -24.32970240761073555, -9.889122670036343266 ) ) ;
#31226 = CARTESIAN_POINT ( 'NONE',  ( 14.91791411132470380, 23.94192138950630877, -11.62984915953536458 ) ) ;
#31227 = CARTESIAN_POINT ( 'NONE',  ( 18.31926634591793501, 9.392207553935453035, -27.73388598276786965 ) ) ;
#31228 = DIRECTION ( 'NONE',  ( -0.000000000000000000, -0.000000000000000000, -1.000000000000000000 ) ) ;
#31229 = CONICAL_SURFACE ( 'NONE', #9161, 0.9999999999999981126, 0.7853981633974562726 ) ;
#31230 = ORIENTED_EDGE ( 'NONE', *, *, #20179, .F. ) ;
#31231 = CARTESIAN_POINT ( 'NONE',  ( -31.10576488114211102, -3.143594509563115924, -11.36259591356684062 ) ) ;
#31232 = CARTESIAN_POINT ( 'NONE',  ( -17.25967040862722612, 21.92197836111047593, 15.72805884749868532 ) ) ;
#31233 = ORIENTED_EDGE ( 'NONE', *, *, #7069, .F. ) ;
#31234 = DIRECTION ( 'NONE',  ( 0.5138379476002949975, 0.6345370204113977008, 0.5773502691896332806 ) ) ;
#31235 = DIRECTION ( 'NONE',  ( 0.000000000000000000, 0.000000000000000000, 1.000000000000000000 ) ) ;
#31236 = EDGE_CURVE ( 'NONE', #21311, #2857, #27513, .T. ) ;
#31237 = CARTESIAN_POINT ( 'NONE',  ( -20.57568126879977299, 1.353978323836376507, -28.10186790039112026 ) ) ;
#31238 = EDGE_CURVE ( 'NONE', #15391, #5046, #35899, .T. ) ;
#31239 = CARTESIAN_POINT ( 'NONE',  ( 20.00198754538222445, -6.713423164100702500, -26.34058677862946851 ) ) ;
#31240 = EDGE_CURVE ( 'NONE', #19274, #21780, #8058, .T. ) ;
#31241 = CARTESIAN_POINT ( 'NONE',  ( 20.76390118686654418, -28.86769433464313650, 13.32518128616608344 ) ) ;
#31242 = CIRCLE ( 'NONE', #31874, 1.000000000000000000 ) ;
#31243 = AXIS2_PLACEMENT_3D ( 'NONE', #18709, #12606, #12403 ) ;
#31244 = ORIENTED_EDGE ( 'NONE', *, *, #9844, .T. ) ;
#31245 = CARTESIAN_POINT ( 'NONE',  ( -16.99999999999999645, 22.50000000000000355, 6.000000000000000000 ) ) ;
#31246 = VERTEX_POINT ( 'NONE', #20261 ) ;
#31247 = CARTESIAN_POINT ( 'NONE',  ( 10.47804177580207607, 33.28010392086025604, 11.00000000000000000 ) ) ;
#31248 = CARTESIAN_POINT ( 'NONE',  ( -0.4999999999999995559, 37.00000000000000711, 11.00000000000000000 ) ) ;
#31249 = DIRECTION ( 'NONE',  ( -0.6691306063588662312, -0.7431448254773869166, 0.000000000000000000 ) ) ;
#31250 = VERTEX_POINT ( 'NONE', #35498 ) ;
#31251 = CARTESIAN_POINT ( 'NONE',  ( -3.459042231567057257, 30.96747855261283178, -14.75290876766932335 ) ) ;
#31252 = DIRECTION ( 'NONE',  ( 0.000000000000000000, 0.000000000000000000, 1.000000000000000000 ) ) ;
#31253 = DIRECTION ( 'NONE',  ( 1.000000000000000000, 0.000000000000000000, 0.000000000000000000 ) ) ;
#31254 = AXIS2_PLACEMENT_3D ( 'NONE', #35581, #7739, #20143 ) ;
#31255 = CARTESIAN_POINT ( 'NONE',  ( -8.411683849014160330, 19.76687823897114882, 9.000000000000001776 ) ) ;
#31256 = CARTESIAN_POINT ( 'NONE',  ( 10.36408355391611913, 20.65655971416340009, 10.75000000000000888 ) ) ;
#31257 = EDGE_CURVE ( 'NONE', #25284, #29357, #25562, .T. ) ;
#31258 = DIRECTION ( 'NONE',  ( -0.9945218953682730678, 0.1045284632676569819, 0.000000000000000000 ) ) ;
#31259 = CARTESIAN_POINT ( 'NONE',  ( 10.45266244534071021, 24.84435709915603852, -17.03677774345998230 ) ) ;
#31260 = EDGE_LOOP ( 'NONE', ( #28233, #23945, #25610, #25985 ) ) ;
#31261 = CARTESIAN_POINT ( 'NONE',  ( -20.65776629622001082, 13.64123596302417241, -6.939388818800391157 ) ) ;
#31262 = DIRECTION ( 'NONE',  ( 1.000000000000000000, 0.000000000000000000, 0.000000000000000000 ) ) ;
#31263 = EDGE_CURVE ( 'NONE', #15556, #12231, #9368, .T. ) ;
#31264 = CARTESIAN_POINT ( 'NONE',  ( 11.31736706274068460, -20.44517872681216986, -20.52400851952886285 ) ) ;
#31265 = DIRECTION ( 'NONE',  ( 0.9781476007338069101, 0.2079116908177532641, 0.000000000000000000 ) ) ;
#31266 = CARTESIAN_POINT ( 'NONE',  ( 13.99558646605622414, 24.01852084437423684, -13.50539560667067107 ) ) ;
#31267 = CARTESIAN_POINT ( 'NONE',  ( 37.62663912510992503, -8.659558992827964374, -5.000000000000018652 ) ) ;
#31268 = DIRECTION ( 'NONE',  ( 0.4067366430757905493, -0.9135454576426051965, 0.000000000000000000 ) ) ;
#31269 = CARTESIAN_POINT ( 'NONE',  ( -17.19550777949286768, -18.19888545701767768, -19.88174267863434608 ) ) ;
#31270 = CARTESIAN_POINT ( 'NONE',  ( 12.41040698953132448, -25.06815925899662645, -10.70177142058002140 ) ) ;
#31271 = CARTESIAN_POINT ( 'NONE',  ( 11.10914253955145448, 17.37933916143984447, -28.08151274450654711 ) ) ;
#31272 = CARTESIAN_POINT ( 'NONE',  ( 31.02556648718628196, -22.39342206112319289, -5.436432259396653421 ) ) ;
#31273 = DIRECTION ( 'NONE',  ( 0.000000000000000000, 0.000000000000000000, 1.000000000000000000 ) ) ;
#31274 = CARTESIAN_POINT ( 'NONE',  ( 5.440908595777817602, 35.94977745735560859, 11.00000000000000000 ) ) ;
#31275 = B_SPLINE_CURVE_WITH_KNOTS ( 'NONE', 3,
 ( #30218, #2389, #14779, #34653, #37896, #9478, #31404, #19014 ),
 .UNSPECIFIED., .F., .F.,
 ( 4, 2, 2, 4 ),
 ( 0.000000000000000000, 0.0004726692273637104840, 0.0007090038410455680841, 0.0009453384547274256301 ),
 .UNSPECIFIED. ) ;
#31276 = ORIENTED_EDGE ( 'NONE', *, *, #31386, .F. ) ;
#31277 = CARTESIAN_POINT ( 'NONE',  ( -11.05743542808008506, 33.66909318204464086, -7.195062545379004249 ) ) ;
#31278 = CARTESIAN_POINT ( 'NONE',  ( 0.7609933293816413258, 37.44611345180491213, 10.49999999999999822 ) ) ;
#31279 = DIRECTION ( 'NONE',  ( 1.000000000000000000, 0.000000000000000000, 0.000000000000000000 ) ) ;
#31280 = DIRECTION ( 'NONE',  ( 1.000000000000000000, 0.000000000000000000, 0.000000000000000000 ) ) ;
#31281 = ORIENTED_EDGE ( 'NONE', *, *, #39802, .T. ) ;
#31282 = CARTESIAN_POINT ( 'NONE',  ( 29.79977705054515269, 0.04608879464290485672, -9.709215146590867818 ) ) ;
#31283 = CARTESIAN_POINT ( 'NONE',  ( -11.06069781764612081, 34.19033620402620954, -4.999999999999999112 ) ) ;
#31284 = AXIS2_PLACEMENT_3D ( 'NONE', #15347, #20859, #39731 ) ;
#31285 = CARTESIAN_POINT ( 'NONE',  ( 6.330070799514983193, 27.28854476845134513, 13.00000000000000178 ) ) ;
#31286 = VERTEX_POINT ( 'NONE', #25738 ) ;
#31287 = CARTESIAN_POINT ( 'NONE',  ( -26.48491323965393462, 0.3066557059962052301, -15.45283448520972769 ) ) ;
#31288 = FACE_OUTER_BOUND ( 'NONE', #14197, .T. ) ;
#31289 = VERTEX_POINT ( 'NONE', #4208 ) ;
#31290 = CARTESIAN_POINT ( 'NONE',  ( 35.04727437832835335, -7.360793022001182351, -5.000000000000008882 ) ) ;
#31291 = AXIS2_PLACEMENT_3D ( 'NONE', #8849, #15733, #22027 ) ;
#31292 = CIRCLE ( 'NONE', #13769, 0.5000000000000004441 ) ;
#31293 = ORIENTED_EDGE ( 'NONE', *, *, #5012, .F. ) ;
#31294 = CARTESIAN_POINT ( 'NONE',  ( -3.857345576530716968, 39.98449713665793581, 12.73282698324867823 ) ) ;
#31295 = CARTESIAN_POINT ( 'NONE',  ( 12.77090408390491305, 15.39748370681878775, 13.00000000000000178 ) ) ;
#31296 = CARTESIAN_POINT ( 'NONE',  ( -1.591208726688853492, -0.2560543600718806490, 10.00000000000000000 ) ) ;
#31297 = CARTESIAN_POINT ( 'NONE',  ( -3.920592112299368104, 34.13862021880815689, 19.27171037444158230 ) ) ;
#31298 = DIRECTION ( 'NONE',  ( -1.000000000000000000, 0.000000000000000000, 0.000000000000000000 ) ) ;
#31299 = ORIENTED_EDGE ( 'NONE', *, *, #16593, .F. ) ;
#31300 = AXIS2_PLACEMENT_3D ( 'NONE', #39051, #27065, #20779 ) ;
#31301 = CARTESIAN_POINT ( 'NONE',  ( 3.992867117591230919, 8.524771480177550487, 11.00000000000000000 ) ) ;
#31302 = CARTESIAN_POINT ( 'NONE',  ( -5.728515882982030405, 19.68564878121862094, -29.99999999999996803 ) ) ;
#31303 = CARTESIAN_POINT ( 'NONE',  ( 9.343266739736582949, 17.68301270189218855, 10.00000000000000000 ) ) ;
#31304 = CARTESIAN_POINT ( 'NONE',  ( 17.03483695331121339, 19.02378625293593473, -11.77568025449220457 ) ) ;
#31305 = CARTESIAN_POINT ( 'NONE',  ( 4.514778716083354126, 20.08757060652311921, -28.49112518072664813 ) ) ;
#31306 = CARTESIAN_POINT ( 'NONE',  ( 10.66098508067554995, -17.52284468788354843, -30.00000000000000000 ) ) ;
#31307 = CARTESIAN_POINT ( 'NONE',  ( 6.151085731882510288, 35.08626808545850650, 9.500000000000000000 ) ) ;
#31308 = DIRECTION ( 'NONE',  ( -1.000000000000000000, 0.000000000000000000, 0.000000000000000000 ) ) ;
#31309 = ORIENTED_EDGE ( 'NONE', *, *, #1870, .F. ) ;
#31310 = CARTESIAN_POINT ( 'NONE',  ( -14.54807450344172892, 24.92773171820151035, -11.60025354066594794 ) ) ;
#31311 = CIRCLE ( 'NONE', #30685, 0.5000000000000004441 ) ;
#31312 = CARTESIAN_POINT ( 'NONE',  ( -35.11176058605715156, -10.96173827525908706, 16.87380292611522847 ) ) ;
#31313 = CARTESIAN_POINT ( 'NONE',  ( 14.47253599967204529, -25.59814919913764442, -10.18550332105856349 ) ) ;
#31314 = CARTESIAN_POINT ( 'NONE',  ( 2.568190708544436429, 12.82247983807081226, 10.00000000000000000 ) ) ;
#31315 = ORIENTED_EDGE ( 'NONE', *, *, #4531, .F. ) ;
#31316 = ORIENTED_EDGE ( 'NONE', *, *, #29321, .T. ) ;
#31317 = CARTESIAN_POINT ( 'NONE',  ( -10.81309686280113525, 19.72027827561758428, -22.58649785105329499 ) ) ;
#31318 = CARTESIAN_POINT ( 'NONE',  ( -15.34191545795870404, -23.11243443870917602, -15.23041013548281697 ) ) ;
#31319 = FACE_BOUND ( 'NONE', #35124, .T. ) ;
#31320 = EDGE_LOOP ( 'NONE', ( #10599, #8499, #31676, #31299 ) ) ;
#31321 = CARTESIAN_POINT ( 'NONE',  ( -20.55867917417221591, -5.738195990446767425, -25.72316019435383438 ) ) ;
#31322 = CARTESIAN_POINT ( 'NONE',  ( -14.71730574774288058, -25.79995879924697633, -9.711345329922794534 ) ) ;
#31323 = DIRECTION ( 'NONE',  ( -1.000000000000000000, 0.000000000000000000, 0.000000000000000000 ) ) ;
#31324 = VERTEX_POINT ( 'NONE', #35703 ) ;
#31325 = CARTESIAN_POINT ( 'NONE',  ( 30.52654454056548872, 0.1756249017533851042, -6.888467937754702675 ) ) ;
#31326 = DIRECTION ( 'NONE',  ( -0.000000000000000000, -0.000000000000000000, -1.000000000000000000 ) ) ;
#31327 = DIRECTION ( 'NONE',  ( 0.000000000000000000, 0.000000000000000000, -1.000000000000000000 ) ) ;
#31328 = ORIENTED_EDGE ( 'NONE', *, *, #18510, .F. ) ;
#31329 = CARTESIAN_POINT ( 'NONE',  ( -29.38226363743932978, 0.04289305711785689618, -10.65132950999735151 ) ) ;
#31330 = ORIENTED_EDGE ( 'NONE', *, *, #21652, .F. ) ;
#31331 = CARTESIAN_POINT ( 'NONE',  ( 27.98788956557562813, -1.032887576452447886, -14.33963790881665368 ) ) ;
#31332 = AXIS2_PLACEMENT_3D ( 'NONE', #10062, #22441, #35048 ) ;
#31333 = DIRECTION ( 'NONE',  ( 1.000000000000000000, 3.469446951953622866E-15, 0.000000000000000000 ) ) ;
#31334 = CARTESIAN_POINT ( 'NONE',  ( 35.51887168742078416, -12.71114019210517121, 16.30093088680192537 ) ) ;
#31335 = EDGE_CURVE ( 'NONE', #16497, #23691, #3503, .T. ) ;
#31336 = VERTEX_POINT ( 'NONE', #23501 ) ;
#31337 = AXIS2_PLACEMENT_3D ( 'NONE', #30776, #21815, #37463 ) ;
#31338 = CARTESIAN_POINT ( 'NONE',  ( -26.32076408150614455, 4.396639818092925367, -9.315417411894323152 ) ) ;
#31339 = LINE ( 'NONE', #15508, #36407 ) ;
#31340 = CARTESIAN_POINT ( 'NONE',  ( -2.109751222703438955, 28.76298082888541785, 20.94377226548378346 ) ) ;
#31341 = DIRECTION ( 'NONE',  ( 1.000000000000000000, 0.000000000000000000, 0.000000000000000000 ) ) ;
#31342 = EDGE_CURVE ( 'NONE', #24101, #4798, #4155, .T. ) ;
#31343 = CARTESIAN_POINT ( 'NONE',  ( 2.525645716490518833, 8.212903943950921715, 11.00000000000000000 ) ) ;
#31344 = ADVANCED_FACE ( 'NONE', ( #19645 ), #38944, .F. ) ;
#31345 = VECTOR ( 'NONE', #36906, 1000.000000000000000 ) ;
#31346 = DIRECTION ( 'NONE',  ( -0.9781476007338041345, 0.2079116908177664202, 0.000000000000000000 ) ) ;
#31347 = DIRECTION ( 'NONE',  ( 1.000000000000000000, 0.000000000000000000, 0.000000000000000000 ) ) ;
#31348 = CARTESIAN_POINT ( 'NONE',  ( -24.48289593984599932, 7.070685527441074925, -8.868132332187178335 ) ) ;
#31349 = CARTESIAN_POINT ( 'NONE',  ( 7.111215932167701759, 17.81698729810774751, 9.000000000000001776 ) ) ;
#31350 = CARTESIAN_POINT ( 'NONE',  ( 22.28594499719783784, -24.59284248905922254, -11.20638719456909804 ) ) ;
#31351 = DIRECTION ( 'NONE',  ( 0.000000000000000000, 0.000000000000000000, 1.000000000000000000 ) ) ;
#31352 = CARTESIAN_POINT ( 'NONE',  ( 12.77624441107838038, 21.90293805066523092, -17.40359543253437380 ) ) ;
#31353 = CIRCLE ( 'NONE', #34603, 1.000000000000000000 ) ;
#31354 = VERTEX_POINT ( 'NONE', #10507 ) ;
#31355 = CARTESIAN_POINT ( 'NONE',  ( -15.51521182627543105, 23.67341184179000990, -10.21785028279580310 ) ) ;
#31356 = CARTESIAN_POINT ( 'NONE',  ( -29.41993030479137516, -12.15499915640478257, 20.25080042701567962 ) ) ;
#31357 = ADVANCED_FACE ( 'NONE', ( #22888 ), #28792, .T. ) ;
#31358 = COLOUR_RGB ( '', 0.09019608, 0.27058824, 0.51372549) ;
#31359 = ADVANCED_FACE ( 'NONE', ( #7450 ), #7854, .F. ) ;
#31360 = PLANE ( 'NONE',  #24379 ) ;
#31361 = CARTESIAN_POINT ( 'NONE',  ( 15.43643446434663069, 26.70998168114506299, -5.474185214589514459 ) ) ;
#31362 = ORIENTED_EDGE ( 'NONE', *, *, #22155, .T. ) ;
#31363 = CARTESIAN_POINT ( 'NONE',  ( 19.48557158514982746, -11.25000000000009415, 3.000000000000000000 ) ) ;
#31364 = ORIENTED_EDGE ( 'NONE', *, *, #8626, .F. ) ;
#31366 = DIRECTION ( 'NONE',  ( 0.8090169943749505599, 0.5877852522924689183, 0.000000000000000000 ) ) ;
#31365 = CARTESIAN_POINT ( 'NONE',  ( -11.00725108063220681, 17.69432998924965261, -26.81932462650155102 ) ) ;
#31367 = CARTESIAN_POINT ( 'NONE',  ( -15.57539791909990257, -26.68962352245197778, -6.414612666884428549 ) ) ;
#31368 = CARTESIAN_POINT ( 'NONE',  ( 12.05736835487432401, 14.38397459621550389, 10.49999999999999822 ) ) ;
#31369 = CIRCLE ( 'NONE', #232, 0.4999999999999995559 ) ;
#31370 = VERTEX_POINT ( 'NONE', #1366 ) ;
#31371 = CARTESIAN_POINT ( 'NONE',  ( -33.62363858789468196, -16.31856935978158418, -8.408815523728231156 ) ) ;
#31372 = CARTESIAN_POINT ( 'NONE',  ( -14.18466236126857716, -26.34951843640821423, -6.418711051328147121 ) ) ;
#31373 = CARTESIAN_POINT ( 'NONE',  ( -12.30736835487442704, 14.81698729810789672, 9.000000000000001776 ) ) ;
#31374 = CARTESIAN_POINT ( 'NONE',  ( 14.35173073918922704, 19.39993939583603222, -17.65283020193257002 ) ) ;
#31375 = ORIENTED_EDGE ( 'NONE', *, *, #3116, .T. ) ;
#31376 = CARTESIAN_POINT ( 'NONE',  ( 24.13344123527126683, 5.447041238337571478, -13.77537616045479574 ) ) ;
#31377 = CYLINDRICAL_SURFACE ( 'NONE', #8930, 0.4999999999999986122 ) ;
#31378 = DIRECTION ( 'NONE',  ( -0.8090169943749426773, 0.5877852522924796874, 0.000000000000000000 ) ) ;
#31379 = DIRECTION ( 'NONE',  ( 0.000000000000000000, -0.000000000000000000, -1.000000000000000000 ) ) ;
#31380 = VERTEX_POINT ( 'NONE', #19857 ) ;
#31381 = CARTESIAN_POINT ( 'NONE',  ( -21.77226783765452822, 0.3831960823903834967, -23.81190093888698556 ) ) ;
#31382 = CARTESIAN_POINT ( 'NONE',  ( 20.53334354118885585, 0.7178733630065357030, -28.70205288258643250 ) ) ;
#31383 = CIRCLE ( 'NONE', #13864, 0.5000000000000004441 ) ;
#31384 = CARTESIAN_POINT ( 'NONE',  ( 28.84864528223400271, -18.09713003384586827, 19.66345542862528362 ) ) ;
#31385 = EDGE_LOOP ( 'NONE', ( #19797, #30929, #39278, #13158, #7201, #32536, #18187 ) ) ;
#31386 = EDGE_CURVE ( 'NONE', #1970, #36443, #32248, .T. ) ;
#31387 = CARTESIAN_POINT ( 'NONE',  ( -3.859759734048395785E-14, -22.74351282448223799, -30.00000000000000355 ) ) ;
#31388 = AXIS2_PLACEMENT_3D ( 'NONE', #33478, #30423, #9077 ) ;
#31389 = CARTESIAN_POINT ( 'NONE',  ( 14.86556419889027048, 20.43481210330100240, 10.49999999999999822 ) ) ;
#31390 = ADVANCED_FACE ( 'NONE', ( #30903 ), #426, .F. ) ;
#31391 = ORIENTED_EDGE ( 'NONE', *, *, #30268, .F. ) ;
#31392 = DIRECTION ( 'NONE',  ( 0.5254827454987569535, 0.4731467892558117172, -0.7071067811865512365 ) ) ;
#31393 = AXIS2_PLACEMENT_3D ( 'NONE', #6402, #34445, #3167 ) ;
#31394 = CARTESIAN_POINT ( 'NONE',  ( -13.64211604268330724, 20.79918788657763429, 6.000000000000000000 ) ) ;
#31395 = CARTESIAN_POINT ( 'NONE',  ( -8.917741276437942233, 30.52956727630665057, 6.000000000000000000 ) ) ;
#31396 = CARTESIAN_POINT ( 'NONE',  ( 1.491327628155283636, 21.09632261899129801, -26.26494682969926941 ) ) ;
#31397 = DIRECTION ( 'NONE',  ( -0.4067366430757888840, 0.9135454576426058626, 0.000000000000000000 ) ) ;
#31398 = FACE_OUTER_BOUND ( 'NONE', #39631, .T. ) ;
#31399 = DIRECTION ( 'NONE',  ( -0.000000000000000000, -0.000000000000000000, -1.000000000000000000 ) ) ;
#31400 = DIRECTION ( 'NONE',  ( 0.000000000000000000, 0.000000000000000000, 1.000000000000000000 ) ) ;
#31401 = CARTESIAN_POINT ( 'NONE',  ( -10.29511041547402073, 24.79362192464190073, 10.50000000000000533 ) ) ;
#31402 =( NAMED_UNIT ( * ) SI_UNIT ( $, .STERADIAN. ) SOLID_ANGLE_UNIT ( ) );
#31403 = CARTESIAN_POINT ( 'NONE',  ( 14.96927680770918911, 27.53662669054819290, -7.330861191698205381 ) ) ;
#31404 = CARTESIAN_POINT ( 'NONE',  ( -6.724783417411255293, 35.90833771957834131, 7.485646746502371940 ) ) ;
#31405 = ORIENTED_EDGE ( 'NONE', *, *, #26893, .F. ) ;
#31407 = CARTESIAN_POINT ( 'NONE',  ( -13.94482798346716201, 26.50521816028930999, 7.000000000000000000 ) ) ;
#31406 = CARTESIAN_POINT ( 'NONE',  ( -18.27253818691323062, 18.69021931283398530, -5.000000000000000000 ) ) ;
#31408 = CIRCLE ( 'NONE', #13900, 1.000000000000002665 ) ;
#31409 = CARTESIAN_POINT ( 'NONE',  ( -12.03571151536224271, 31.45218678977246896, 7.000000000000000000 ) ) ;
#31410 = ADVANCED_FACE ( 'NONE', ( #29199 ), #13751, .F. ) ;
#31411 = CARTESIAN_POINT ( 'NONE',  ( 15.31235917916896128, -26.57453613593431285, -6.888046241755874100 ) ) ;
#31412 = EDGE_CURVE ( 'NONE', #12134, #24274, #34641, .T. ) ;
#31413 = CARTESIAN_POINT ( 'NONE',  ( -13.16997831943846364, -17.85564823066885154, -23.48525575126764764 ) ) ;
#31414 = CARTESIAN_POINT ( 'NONE',  ( 15.23754071310550096, 26.38830581798780983, -7.827869159341425132 ) ) ;
#31415 = CARTESIAN_POINT ( 'NONE',  ( 11.10861966544563728, 17.62435334769741857, -26.82886945948915525 ) ) ;
#31416 = B_SPLINE_SURFACE_WITH_KNOTS ( 'NONE', 3, 3, ( 
 ( #37242, #9414, #268, #12655, #25045, #37439, #21204, #33610, #6547, #5761, #32147, #15906, #22791, #22189, #26040, #1067, #3509, #7347, #12851, #864, #3705, #19545, #6741, #469, #29096 ),
 ( #25840, #4310, #38442, #16105, #16712, #28893, #28689, #28487, #22590, #25242, #34589, #663, #10612, #37642, #31742, #7149, #13043, #19148, #3905, #25432, #13245, #31541, #13448, #38034, #37832 ),
 ( #31936, #10004, #4104, #19752, #1269, #22994, #7555, #28291, #9809, #10410, #13653, #35189, #22384, #34790, #35397, #31340, #6942, #38240, #19347, #16302, #25635, #10206, #34997, #16508, #1672 ),
 ( #20768, #30100, #36003, #35601, #13857, #2274, #14256, #23800, #32759, #4515, #8159, #7756, #33163, #29698, #36205, #17322, #20161, #32354, #26446, #26648, #11020, #39437, #4717, #5117, #19959 ),
 ( #27053, #38641, #39036, #11215, #10815, #17121, #23202, #24000, #1880, #32558, #29499, #14053, #20566, #32961, #17523, #2077, #23605, #5313, #16917, #38843, #11418, #26245, #36399, #23404, #35799 ),
 ( #1469, #29895, #7954, #14452, #20367, #29299, #17724, #26849, #39238, #8367, #14661, #4917, #11619, #12009, #8561, #28044, #24399, #5506, #15257, #18710, #11812, #36791, #33763, #30303, #24999 ),
 ( #14862, #18511, #27645, #30900, #21547, #27249, #5909, #40027, #36995, #21153, #9164, #24796, #34151, #3264, #20956, #33364, #17920, #27847, #31101, #20, #8765, #36594, #12405, #15658, #24197 ),
 ( #221, #12607, #21744, #5710, #8968, #2476, #39636, #21356, #18312, #6301, #15055, #18120, #33561, #30507, #37193, #24602, #27445, #2670, #39832, #30702, #2868, #12208, #33948, #9367, #6105 ),
 ( #3062, #15456, #28442, #16662, #22144, #814, #10361, #13602, #619, #16458, #22536, #7297, #28843, #19703, #25793, #19497, #34947, #3861, #1021, #28246, #32095, #7101, #9566, #13401, #18904 ),
 ( #423, #34544, #31892, #19103, #38190, #16053, #4055, #22740, #4261, #9764, #35144, #29044, #34745, #6695, #28644, #31297, #12802, #31496, #1224, #6499, #21948, #6895, #37391, #34350, #37787 ),
 ( #16259, #3463, #10163, #15858, #19295, #13195, #25589, #3660, #37990, #25199, #37598, #13000, #25388, #9959, #22339, #31694, #26600, #32710, #16869, #4466, #4862, #38992, #29249, #7908, #7504 ),
 ( #1420, #23149, #22946, #35952, #7711, #35547, #1829, #38590, #13803, #11166, #26195, #29647, #26396, #10764, #19907, #8107, #20113, #32301, #10563, #23557, #17276, #32512, #35348, #14209, #4666 ),
 ( #25990, #17068, #38792, #38389, #29446, #1625, #14007, #10971, #23358, #35753, #20313, #10494, #4193, #7232, #28777, #19632, #22080, #953, #22875, #19431, #7031, #12935, #37725, #22271, #28978 ),
 ( #3990, #34676, #9892, #19230, #38118, #22675, #35078, #16597, #25725, #35279, #6628, #6829, #13536, #1353, #31623, #10291, #7435, #38523, #13128, #1154, #32028, #32233, #25924, #4395, #19844 ),
 ( #16801, #28576, #38324, #26127, #29186, #13738, #551, #13332, #34481, #25326, #3790, #16192, #19036, #16391, #750, #25520, #37921, #31428, #3595, #15992, #28371, #10093, #22473, #34878, #31824 ),
 ( #35187, #34787, #32143, #26441, #19955, #19543, #19750, #13242, #34994, #32351, #31933, #29296, #28889, #4511, #10812, #17118, #22588, #23198, #7552, #7344, #7143, #1266, #31737, #862, #4102 ),
 ( #4306, #32555, #13650, #16506, #20156, #16299, #16913, #29092, #1466, #22990, #28686, #16708, #26037, #38436, #1064, #10609, #26242, #35597, #4714, #10002, #22381, #6939, #13851, #29493, #38637 ),
 ( #3902, #7753, #10204, #13445, #35394, #1669, #14049, #19345, #25838, #38238, #25632, #38031, #10408, #22785, #11808, #5113, #36000, #5706, #8156, #27244, #14658, #17520, #17319, #30504, #29891 ),
 ( #33557, #30300, #20560, #7951, #24194, #14449, #2472, #39033, #23797, #23400, #20764, #15051, #8558, #32957, #8364, #1877, #23602, #20953, #2073, #17916, #26845, #33360, #39632, #18117, #11211 ),
 ( #38840, #2664, #39235, #35795, #5310, #8761, #14253, #11415, #36198, #21150, #2270, #33158, #11016, #4911, #5503, #17720, #14859, #11614, #29693, #30096, #27049, #39433, #23997, #36394, #36591 ),
 ( #20363, #32756, #26644, #419, #33944, #31097, #6102, #15855, #8962, #3459, #27642, #18507, #3261, #19099, #31493, #12799, #24598, #30896, #21353, #3657, #27844, #3059, #25194, #15451, #36991 ),
 ( #28243, #15653, #17, #5905, #27441, #12400, #30699, #24395, #22141, #18900, #9160, #36788, #37594, #24793, #31294, #37190, #24995, #9363, #33760, #15253, #21741, #9761, #21544, #37388, #34147 ),
 ( #34541, #9562, #12604, #6297, #21943, #39829, #18706, #6692, #28040, #217, #18308, #2864, #40023, #34347, #6495, #12006, #12204, #4051, #10159, #16455, #811, #10358, #25385, #16049, #10760 ),
 ( #31689, #7501, #25789, #19292, #13192, #25987, #37987, #35343, #34943, #10559, #16865, #23145, #28640, #29246, #13599, #13398, #25586, #7293, #37784, #6892, #22533, #35543, #9956, #28438, #38186 ),
 ( #26192, #22336, #38385, #35141, #22942, #29041, #34741, #22735, #19698, #4258, #7095, #16659, #32298, #1417, #7707, #32507, #615, #12996, #19904, #38585, #4462, #16255, #3858, #13799, #20109 ) ),
 .UNSPECIFIED., .F., .F., .F.,
 ( 4, 3, 3, 3, 3, 3, 3, 3, 4 ),
 ( 4, 3, 3, 3, 3, 3, 3, 3, 4 ),
 ( 0.000000000000000000, 0.1250000000000000000, 0.2500000000000000000, 0.3750000000000000000, 0.5000000000000000000, 0.6250000000000000000, 0.7500000000000000000, 0.8750000000000000000, 1.000000000000000000 ),
 ( 0.2711095619351722164, 0.5960312531501053002, 0.9209529443650383840, 1.245874635579971468, 1.570796326794904552, 1.895718018009837635, 2.220639709224770719, 2.545561400439703803, 2.870483091654636887 ),
 .UNSPECIFIED. ) ;
#31417 = EDGE_LOOP ( 'NONE', ( #22821, #16483, #27438, #3056 ) ) ;
#31418 = CARTESIAN_POINT ( 'NONE',  ( 9.806975420853749625, 31.15003855377755571, 13.00000000000000178 ) ) ;
#31419 = CARTESIAN_POINT ( 'NONE',  ( -14.24588017709789156, -25.05103694589206142, -11.60217997011687530 ) ) ;
#31420 = CARTESIAN_POINT ( 'NONE',  ( -37.17935095643291987, -12.86265498539201957, 13.32518128616588626 ) ) ;
#31421 = CIRCLE ( 'NONE', #26224, 1.000000000000000000 ) ;
#31422 = CARTESIAN_POINT ( 'NONE',  ( -27.56419008223693368, -20.32132774350781546, -11.98953026114993214 ) ) ;
#31423 = CARTESIAN_POINT ( 'NONE',  ( -4.514867549693919457, -24.02565271312832351, -11.85143917347367370 ) ) ;
#31424 = CARTESIAN_POINT ( 'NONE',  ( 15.67016653301135243, 25.89419373281741343, -4.999999999999999112 ) ) ;
#31425 = ORIENTED_EDGE ( 'NONE', *, *, #20205, .F. ) ;
#31426 = CARTESIAN_POINT ( 'NONE',  ( 18.71476311508316925, 8.734133638284580670, -27.16947995569030283 ) ) ;
#31427 = CARTESIAN_POINT ( 'NONE',  ( 12.25538945203533459, -14.54837145661906384, 23.00000000000000355 ) ) ;
#31428 = CARTESIAN_POINT ( 'NONE',  ( -8.062736477019040393, 35.88854577675052582, 16.87380292611359422 ) ) ;
#31429 = ORIENTED_EDGE ( 'NONE', *, *, #11723, .T. ) ;
#31430 = CARTESIAN_POINT ( 'NONE',  ( -20.35866630304074221, -2.409458700188494618, -30.00000000000000000 ) ) ;
#31431 = CIRCLE ( 'NONE', #1597, 1.000000000000000000 ) ;
#31432 = CARTESIAN_POINT ( 'NONE',  ( -14.43694901005832243, 26.51279404185573796, 17.42190598798392998 ) ) ;
#31433 = EDGE_LOOP ( 'NONE', ( #302, #32782, #38707, #13118 ) ) ;
#31434 = CARTESIAN_POINT ( 'NONE',  ( 3.713592597587160871, 7.966960743906808418, 7.499999999999990230 ) ) ;
#31435 = DIRECTION ( 'NONE',  ( 1.000000000000000000, 0.000000000000000000, 0.000000000000000000 ) ) ;
#31436 = CARTESIAN_POINT ( 'NONE',  ( -29.53879188788242516, 0.8751376573578146800, -8.306695801703410709 ) ) ;
#31437 = ADVANCED_FACE ( 'NONE', ( #27155 ), #33665, .F. ) ;
#31438 = CARTESIAN_POINT ( 'NONE',  ( 34.91094743763966335, -15.30826278171658927, -5.859126002197243110 ) ) ;
#31439 = CARTESIAN_POINT ( 'NONE',  ( 31.02271782694946722, -24.34398845624577135, 13.92931973827809067 ) ) ;
#31440 = ORIENTED_EDGE ( 'NONE', *, *, #16309, .F. ) ;
#31441 = ADVANCED_FACE ( 'NONE', ( #33066 ), #30412, .F. ) ;
#31442 = ORIENTED_EDGE ( 'NONE', *, *, #11269, .T. ) ;
#31443 = B_SPLINE_CURVE_WITH_KNOTS ( 'NONE', 3,
 ( #26539, #2161, #35883, #33251 ),
 .UNSPECIFIED., .F., .F.,
 ( 4, 4 ),
 ( 0.000000000000000000, 1.000000000000000000 ),
 .UNSPECIFIED. ) ;
#31444 = CARTESIAN_POINT ( 'NONE',  ( 15.00099999999999767, 36.50000000000000711, 7.000000000000000000 ) ) ;
#31445 = CARTESIAN_POINT ( 'NONE',  ( 19.26948696230200397, 27.85601271560037162, 22.99999999999999645 ) ) ;
#31446 = AXIS2_PLACEMENT_3D ( 'NONE', #25956, #22504, #19666 ) ;
#31447 = CARTESIAN_POINT ( 'NONE',  ( 13.62380822250710999, 25.87518140495407692, 10.50000000000000000 ) ) ;
#31448 = ORIENTED_EDGE ( 'NONE', *, *, #33524, .T. ) ;
#31449 = CARTESIAN_POINT ( 'NONE',  ( -2.937369183556012509, 36.26184006374910496, -9.732975961863635561 ) ) ;
#31450 = CARTESIAN_POINT ( 'NONE',  ( 3.118671991557230516, 37.17221401100731981, 13.00000000000000178 ) ) ;
#31451 = LINE ( 'NONE', #33911, #9205 ) ;
#31452 = DIRECTION ( 'NONE',  ( 0.2079116908177534029, -0.9781476007338067991, 0.000000000000000000 ) ) ;
#31453 = DIRECTION ( 'NONE',  ( 0.07391278520358296467, 0.7032331762533997610, -0.7071067811865502373 ) ) ;
#31454 = DIRECTION ( 'NONE',  ( -0.9945218953682730678, 0.1045284632676569819, 0.000000000000000000 ) ) ;
#31455 = CARTESIAN_POINT ( 'NONE',  ( 13.49628937919752936, 30.16421895756228011, -8.163569957728929793 ) ) ;
#31456 = AXIS2_PLACEMENT_3D ( 'NONE', #31846, #6651, #19059 ) ;
#31457 = VERTEX_POINT ( 'NONE', #14561 ) ;
#31458 = CARTESIAN_POINT ( 'NONE',  ( -18.27861351387878486, 9.971955297741459390, -25.50930699828377257 ) ) ;
#31459 = CARTESIAN_POINT ( 'NONE',  ( -19.26948696230206437, 27.85601271560034320, 11.00000000000000000 ) ) ;
#31460 = CARTESIAN_POINT ( 'NONE',  ( 9.732651874096569955, -18.42127846640838484, -26.82682959031351189 ) ) ;
#31461 = CARTESIAN_POINT ( 'NONE',  ( -13.16028273094462975, 27.30176617939698147, 10.00000000000000000 ) ) ;
#31462 = CARTESIAN_POINT ( 'NONE',  ( 15.34082215761350731, 26.78240229728934807, -6.415436508019739748 ) ) ;
#31463 = EDGE_CURVE ( 'NONE', #15902, #14950, #39201, .T. ) ;
#31464 = CARTESIAN_POINT ( 'NONE',  ( -31.47283671532261806, -25.12609584734821766, -14.45070082761205477 ) ) ;
#31465 = DIRECTION ( 'NONE',  ( 0.8090169943749426773, -0.5877852522924797984, 0.000000000000000000 ) ) ;
#31466 = EDGE_CURVE ( 'NONE', #18645, #32074, #21060, .T. ) ;
#31467 = CARTESIAN_POINT ( 'NONE',  ( -22.06585941720839017, -22.05058654489405967, -13.92938651405431649 ) ) ;
#31468 = CARTESIAN_POINT ( 'NONE',  ( 10.76261159742561802, -25.66954346325781700, -5.474903014184794969 ) ) ;
#31469 = CARTESIAN_POINT ( 'NONE',  ( 15.18929233869975803, 25.85343093234575562, -8.770441219456733606 ) ) ;
#31470 = CARTESIAN_POINT ( 'NONE',  ( 29.20799977545595638, -19.79325530109120379, -11.07381889372395456 ) ) ;
#31471 = CARTESIAN_POINT ( 'NONE',  ( 8.229154955994852472, 10.32288908946079076, 10.96580508970283141 ) ) ;
#31472 = CARTESIAN_POINT ( 'NONE',  ( 5.465749975257575777, 36.45564430483320706, 10.49999999999999822 ) ) ;
#31473 = VERTEX_POINT ( 'NONE', #14960 ) ;
#31474 = CARTESIAN_POINT ( 'NONE',  ( -5.905911943458037605, 19.71813378021714769, -28.52406569151924742 ) ) ;
#31475 = DIRECTION ( 'NONE',  ( -0.4156269377774530760, 0.5720614028176880250, -0.7071067811865446862 ) ) ;
#31476 = AXIS2_PLACEMENT_3D ( 'NONE', #4230, #22311, #28409 ) ;
#31477 = CARTESIAN_POINT ( 'NONE',  ( -11.81630298851966288, 31.79381426990562787, 10.50000000000000000 ) ) ;
#31478 = EDGE_LOOP ( 'NONE', ( #31906, #33891 ) ) ;
#31479 = CARTESIAN_POINT ( 'NONE',  ( 30.94149296799522020, -0.08026563842153495998, -4.999999999999999112 ) ) ;
#31480 = CARTESIAN_POINT ( 'NONE',  ( 4.591666147298500533, 15.32946292166668556, 9.000000000000001776 ) ) ;
#31481 = CARTESIAN_POINT ( 'NONE',  ( -7.766013557953294288, 28.81973365084998306, 10.50000000000000000 ) ) ;
#31482 = ORIENTED_EDGE ( 'NONE', *, *, #3827, .T. ) ;
#31483 = VECTOR ( 'NONE', #30172, 1000.000000000000000 ) ;
#31484 = CARTESIAN_POINT ( 'NONE',  ( -28.84883529782520384, 0.1510037028947092130, -11.60082923936701782 ) ) ;
#31485 = CARTESIAN_POINT ( 'NONE',  ( -18.54826650170510760, -24.72227203249315863, -12.26027862771963228 ) ) ;
#31486 = EDGE_CURVE ( 'NONE', #12932, #22404, #2766, .T. ) ;
#31487 = VERTEX_POINT ( 'NONE', #8668 ) ;
#31488 = CARTESIAN_POINT ( 'NONE',  ( 20.61284349087890178, -4.224483801661988558, -26.46532051397237595 ) ) ;
#31489 = CONICAL_SURFACE ( 'NONE', #374, 1.000000000000014655, 0.7853981633974520538 ) ;
#31490 = CIRCLE ( 'NONE', #5528, 1.000000000000000888 ) ;
#31491 = EDGE_CURVE ( 'NONE', #30787, #24743, #36701, .T. ) ;
#31492 = EDGE_LOOP ( 'NONE', ( #11261, #19114 ) ) ;
#31493 = CARTESIAN_POINT ( 'NONE',  ( -3.827636526755954449, 39.84991882288245080, 13.32518128616621844 ) ) ;
#31494 = DIRECTION ( 'NONE',  ( -0.5254827454987639479, -0.4731467892558146593, -0.7071067811865439090 ) ) ;
#31495 = CARTESIAN_POINT ( 'NONE',  ( -6.471455985784314358, 17.88805487301255681, 23.00000000000000000 ) ) ;
#31496 = CARTESIAN_POINT ( 'NONE',  ( -6.372562348374944285, 33.08234073370745421, 19.27171037444085755 ) ) ;
#31497 = EDGE_CURVE ( 'NONE', #6388, #648, #26879, .T. ) ;
#31498 = CYLINDRICAL_SURFACE ( 'NONE', #1927, 1.000000000000000888 ) ;
#31499 = VERTEX_POINT ( 'NONE', #39340 ) ;
#31500 = DIRECTION ( 'NONE',  ( 0.9781476007338069101, 0.2079116908177532641, -0.000000000000000000 ) ) ;
#31501 = CARTESIAN_POINT ( 'NONE',  ( -18.94584503392242425, -7.857761768003762803, -30.00000000000000000 ) ) ;
#31502 = CARTESIAN_POINT ( 'NONE',  ( 5.440908595777814050, 35.94977745735560859, 7.000000000000000000 ) ) ;
#31503 = DIRECTION ( 'NONE',  ( -1.000000000000000000, 0.000000000000000000, 0.000000000000000000 ) ) ;
#31504 = CARTESIAN_POINT ( 'NONE',  ( 14.00978157989841932, 15.66612192722645780, -25.31855382825745693 ) ) ;
#31505 = CARTESIAN_POINT ( 'NONE',  ( 5.567050714568646974, 24.71546371777111517, -19.77525644353581669 ) ) ;
#31506 = ORIENTED_EDGE ( 'NONE', *, *, #24897, .T. ) ;
#31507 = CARTESIAN_POINT ( 'NONE',  ( 14.98429054056425791, -24.74230029465469372, -12.47804673543034681 ) ) ;
#31508 = CARTESIAN_POINT ( 'NONE',  ( 15.00437666251104396, -28.61930095463400292, 12.14047268033097637 ) ) ;
#31509 = ADVANCED_FACE ( 'NONE', ( #11518 ), #5417, .F. ) ;
#31510 = CARTESIAN_POINT ( 'NONE',  ( -14.02783499842349002, 22.03112340962126581, 10.50000000000000000 ) ) ;
#31511 = EDGE_CURVE ( 'NONE', #10646, #37532, #28538, .T. ) ;
#31512 = ORIENTED_EDGE ( 'NONE', *, *, #39373, .T. ) ;
#31513 = AXIS2_PLACEMENT_3D ( 'NONE', #14374, #7672, #38956 ) ;
#31514 = CARTESIAN_POINT ( 'NONE',  ( -11.32195743957676726, 18.02873052150704325, -25.01618100487094409 ) ) ;
#31515 = AXIS2_PLACEMENT_3D ( 'NONE', #31905, #38207, #35365 ) ;
#31516 = CARTESIAN_POINT ( 'NONE',  ( -30.17922767059458167, -0.7536324250905129807, 17.42190598798392998 ) ) ;
#31517 = CARTESIAN_POINT ( 'NONE',  ( 15.03800791059918396, -26.62802654356141119, -5.000000000000000888 ) ) ;
#31518 = DIRECTION ( 'NONE',  ( 0.000000000000000000, 0.000000000000000000, 1.000000000000000000 ) ) ;
#31519 = ORIENTED_EDGE ( 'NONE', *, *, #3846, .T. ) ;
#31520 = ORIENTED_EDGE ( 'NONE', *, *, #1677, .T. ) ;
#31521 = CARTESIAN_POINT ( 'NONE',  ( -9.991501677813444005, 23.11176406337531120, -19.09605641320739267 ) ) ;
#31522 = CARTESIAN_POINT ( 'NONE',  ( -7.659620408498105881, 26.92228390473685096, 9.000000000000001776 ) ) ;
#31523 = FACE_BOUND ( 'NONE', #10185, .T. ) ;
#31524 = CARTESIAN_POINT ( 'NONE',  ( -34.93438416866315066, -9.757236910605460167, -7.597984259234436877 ) ) ;
#31525 = CARTESIAN_POINT ( 'NONE',  ( -9.861416007139599316, -18.85607788447654443, -25.02649126457271223 ) ) ;
#31526 = CARTESIAN_POINT ( 'NONE',  ( -20.23249103036706842, 12.99895069675662640, 9.500000000000000000 ) ) ;
#31527 = ORIENTED_EDGE ( 'NONE', *, *, #15478, .F. ) ;
#31528 = CARTESIAN_POINT ( 'NONE',  ( 28.14739292305172924, 0.3821647062335758460, -12.56146095346657532 ) ) ;
#31529 = DIRECTION ( 'NONE',  ( 0.000000000000000000, 0.000000000000000000, 1.000000000000000000 ) ) ;
#31530 = LINE ( 'NONE', #33796, #24494 ) ;
#31531 = ORIENTED_EDGE ( 'NONE', *, *, #34357, .T. ) ;
#31532 = CARTESIAN_POINT ( 'NONE',  ( -23.95715816398616127, 0.4476729911382093530, -19.49109017648843789 ) ) ;
#31533 = ORIENTED_EDGE ( 'NONE', *, *, #38926, .T. ) ;
#31534 = CARTESIAN_POINT ( 'NONE',  ( 20.50115022911059270, -0.2752137519716085223, -29.32748844547824163 ) ) ;
#31535 = CARTESIAN_POINT ( 'NONE',  ( 24.22138565352629058, -9.557272464391640909, 21.00000000000001066 ) ) ;
#31536 = CARTESIAN_POINT ( 'NONE',  ( 33.67755813373108964, -6.176019118478268233, 17.42190598798353562 ) ) ;
#31537 = EDGE_CURVE ( 'NONE', #28022, #29830, #24102, .T. ) ;
#31538 = ORIENTED_EDGE ( 'NONE', *, *, #367, .T. ) ;
#31539 = CIRCLE ( 'NONE', #18583, 0.4999999999999997780 ) ;
#31540 = CARTESIAN_POINT ( 'NONE',  ( -17.34253826607186966, 27.32041144404028188, 23.00000000000000000 ) ) ;
#31541 = CARTESIAN_POINT ( 'NONE',  ( -4.791301586986582706, 25.75006569903015574, 20.99999999999999645 ) ) ;
#31542 = CARTESIAN_POINT ( 'NONE',  ( -7.929471891321299815, 25.60217271033470965, 9.000000000000001776 ) ) ;
#31543 = AXIS2_PLACEMENT_3D ( 'NONE', #19069, #16020, #12767 ) ;
#31544 = CARTESIAN_POINT ( 'NONE',  ( -2.916683454136887121, 12.38538396040838840, 10.75000000000001776 ) ) ;
#31545 = FACE_BOUND ( 'NONE', #14230, .T. ) ;
#31546 = CARTESIAN_POINT ( 'NONE',  ( 18.63686013480785775, 22.43247111562878615, 12.14047268031015214 ) ) ;
#31547 = CARTESIAN_POINT ( 'NONE',  ( -22.69387413952485488, 8.732923056282277940, -11.85621800793260405 ) ) ;
#31548 = CARTESIAN_POINT ( 'NONE',  ( 21.16136169972589443, -23.36689248179594713, -13.05645000173869441 ) ) ;
#31549 = LINE ( 'NONE', #18964, #154 ) ;
#31550 = CARTESIAN_POINT ( 'NONE',  ( 12.85423046086276777, 21.77606881879581024, -17.42081002309879167 ) ) ;
#31551 = ORIENTED_EDGE ( 'NONE', *, *, #688, .F. ) ;
#31552 = CARTESIAN_POINT ( 'NONE',  ( -15.50946703677032268, 25.48995504883554375, -7.833083979528388419 ) ) ;
#31553 = CARTESIAN_POINT ( 'NONE',  ( -21.27406655599722995, -21.06385835267891693, 20.25080042701542382 ) ) ;
#31554 = DIRECTION ( 'NONE',  ( 1.000000000000000000, 0.000000000000000000, 0.000000000000000000 ) ) ;
#31555 = CARTESIAN_POINT ( 'NONE',  ( 12.67586314470820419, 21.02061172028682989, -18.45614634320944702 ) ) ;
#31556 = ORIENTED_EDGE ( 'NONE', *, *, #36199, .T. ) ;
#31557 = ADVANCED_FACE ( 'NONE', ( #30606 ), #39933, .F. ) ;
#31558 = CARTESIAN_POINT ( 'NONE',  ( -13.97557076678966403, 21.53386246193713305, 7.500000000000004441 ) ) ;
#31559 = EDGE_LOOP ( 'NONE', ( #13946, #17687, #8944, #10446 ) ) ;
#31561 = CARTESIAN_POINT ( 'NONE',  ( 14.97283171447379146, 21.48159823030311344, 7.000000000000000000 ) ) ;
#31560 = CARTESIAN_POINT ( 'NONE',  ( -15.28843509798326750, 26.96128135507572310, -6.412575688757890191 ) ) ;
#31562 = CARTESIAN_POINT ( 'NONE',  ( -15.97359574264618409, -26.56429016778576369, -7.804459717415208608 ) ) ;
#31563 = DIRECTION ( 'NONE',  ( 0.000000000000000000, 0.000000000000000000, 1.000000000000000000 ) ) ;
#31564 = CIRCLE ( 'NONE', #17324, 0.5000000000000004441 ) ;
#31565 = ORIENTED_EDGE ( 'NONE', *, *, #17341, .F. ) ;
#31566 = CARTESIAN_POINT ( 'NONE',  ( -20.21266914523116043, -10.59870367858544071, -22.98988714542691625 ) ) ;
#31567 = CARTESIAN_POINT ( 'NONE',  ( -8.977629974610007224, -18.64362841147424632, -27.49153544992771359 ) ) ;
#31568 = CARTESIAN_POINT ( 'NONE',  ( -5.288651019503864958, 36.01756689786831345, 10.83333333333333215 ) ) ;
#31569 = CARTESIAN_POINT ( 'NONE',  ( 15.70302840757942953, 22.76320954772178240, -10.71404650329602326 ) ) ;
#31570 = ORIENTED_EDGE ( 'NONE', *, *, #26713, .F. ) ;
#31571 = CARTESIAN_POINT ( 'NONE',  ( 19.71254563347552846, 5.914222174241564822, -28.25527075934179067 ) ) ;
#31572 = CARTESIAN_POINT ( 'NONE',  ( -21.39877161664097827, 15.54711762656374141, 7.000000000000000000 ) ) ;
#31573 = FACE_OUTER_BOUND ( 'NONE', #26007, .T. ) ;
#31574 = CARTESIAN_POINT ( 'NONE',  ( -13.16997832219843545, -17.85564823411818836, -23.48525574308021646 ) ) ;
#31575 = ORIENTED_EDGE ( 'NONE', *, *, #1712, .F. ) ;
#31576 = CARTESIAN_POINT ( 'NONE',  ( -31.07115740369864199, -0.3229936248456179992, -6.410853627256240195 ) ) ;
#31577 = CARTESIAN_POINT ( 'NONE',  ( 27.38313135976468260, -0.1050505738281504176, -14.43771228336784063 ) ) ;
#31578 = CARTESIAN_POINT ( 'NONE',  ( 27.96047413129323189, -4.559793092418160221, 19.99202127657250116 ) ) ;
#31579 = EDGE_LOOP ( 'NONE', ( #2545, #11827, #1201, #26787, #30176, #28136, #34682, #13460 ) ) ;
#31580 = CARTESIAN_POINT ( 'NONE',  ( 13.28992586503610163, -18.25382200079949513, -20.55760979252977094 ) ) ;
#31581 = CARTESIAN_POINT ( 'NONE',  ( 1.247466774197339978, 28.36888560440311480, 12.00000000000000000 ) ) ;
#31582 = VERTEX_POINT ( 'NONE', #39737 ) ;
#31583 = EDGE_CURVE ( 'NONE', #32934, #4065, #24497, .T. ) ;
#31584 = CARTESIAN_POINT ( 'NONE',  ( -5.049784273262889478, -26.77689918168220018, -5.000000000000000888 ) ) ;
#31585 = CIRCLE ( 'NONE', #33590, 1.000000000000000000 ) ;
#31586 = PLANE ( 'NONE',  #7798 ) ;
#31587 = CARTESIAN_POINT ( 'NONE',  ( 8.935770203493859754, 22.34671014717335780, 12.00000000000000000 ) ) ;
#31588 = CARTESIAN_POINT ( 'NONE',  ( 2.668841116913945211, 20.33496311051875693, -30.00000000000001066 ) ) ;
#31589 = FACE_OUTER_BOUND ( 'NONE', #32372, .T. ) ;
#31590 = EDGE_LOOP ( 'NONE', ( #37074, #14479, #24182, #23304, #11015, #4483, #38859, #35472, #32922, #4953, #24486, #10481, #9102, #2055, #22140, #36065, #29712, #14331, #28721, #5779, #35154, #18806, #24160, #7649, #7774, #900 ) ) ;
#31591 = LINE ( 'NONE', #6407, #9148 ) ;
#31592 = CARTESIAN_POINT ( 'NONE',  ( -1.853172919594719970, 21.57294901687549427, 13.00000000000000178 ) ) ;
#31593 = AXIS2_PLACEMENT_3D ( 'NONE', #36938, #34289, #33895 ) ;
#31594 = FACE_OUTER_BOUND ( 'NONE', #22100, .T. ) ;
#31595 = DIRECTION ( 'NONE',  ( -1.000000000000000000, 0.000000000000000000, 0.000000000000000000 ) ) ;
#31596 = CARTESIAN_POINT ( 'NONE',  ( 15.03773630625828517, 27.03340586037365867, -7.807355954524350494 ) ) ;
#31597 = AXIS2_PLACEMENT_3D ( 'NONE', #30214, #14164, #11328 ) ;
#31598 = PLANE ( 'NONE',  #2262 ) ;
#31599 = VERTEX_POINT ( 'NONE', #39136 ) ;
#31601 = LINE ( 'NONE', #17135, #23948 ) ;
#31600 = CARTESIAN_POINT ( 'NONE',  ( -17.24705954285015963, 17.28840653234623659, -13.80911451859712358 ) ) ;
#31602 = CARTESIAN_POINT ( 'NONE',  ( 36.04785107591597892, -18.56329043283713887, 11.00000000000005684 ) ) ;
#31603 = EDGE_CURVE ( 'NONE', #33412, #26968, #30132, .T. ) ;
#31604 = CARTESIAN_POINT ( 'NONE',  ( 13.70278808041313034, -24.11633286913983909, -13.51357506480354154 ) ) ;
#31605 = DIRECTION ( 'NONE',  ( 1.000000000000000000, 0.000000000000000000, 0.000000000000000000 ) ) ;
#31606 = CARTESIAN_POINT ( 'NONE',  ( 14.53734341128950014, 24.95703585460324803, -11.59938498087787195 ) ) ;
#31607 = VERTEX_POINT ( 'NONE', #11321 ) ;
#31608 = CARTESIAN_POINT ( 'NONE',  ( 12.12399539440989393, 19.93227742869169816, -20.53953816727202408 ) ) ;
#31609 = EDGE_LOOP ( 'NONE', ( #3888, #2708, #38422 ) ) ;
#31610 = CARTESIAN_POINT ( 'NONE',  ( -14.86556419889029534, 20.43481210330121556, 11.00000000000000000 ) ) ;
#31611 = EDGE_CURVE ( 'NONE', #14430, #2539, #2869, .T. ) ;
#31612 = CARTESIAN_POINT ( 'NONE',  ( -9.739536567210267393, -18.58453973594571451, -26.22921015961444979 ) ) ;
#31613 = CARTESIAN_POINT ( 'NONE',  ( -28.15028875894780924, -26.91874057851014612, 12.73282698324841711 ) ) ;
#31614 = CARTESIAN_POINT ( 'NONE',  ( -30.65860538206566588, -22.55701637896913070, -6.281012731829498819 ) ) ;
#31615 = CARTESIAN_POINT ( 'NONE',  ( -3.609577435699458547, -21.27339400844680384, -22.19980166077412065 ) ) ;
#31616 = CARTESIAN_POINT ( 'NONE',  ( 11.46030064407786675, 17.14133356389085350, -28.10178865267953441 ) ) ;
#31617 = EDGE_CURVE ( 'NONE', #19220, #14160, #12068, .T. ) ;
#31618 = ORIENTED_EDGE ( 'NONE', *, *, #33612, .F. ) ;
#31619 = CARTESIAN_POINT ( 'NONE',  ( 22.50594045486629469, 10.05894777106499838, -8.895335536218450301 ) ) ;
#31620 = CARTESIAN_POINT ( 'NONE',  ( -9.062230821157587712, 11.16111041642498591, 10.83333333333333215 ) ) ;
#31621 = EDGE_CURVE ( 'NONE', #21433, #172, #24898, .T. ) ;
#31622 = B_SPLINE_CURVE_WITH_KNOTS ( 'NONE', 3,
 ( #7309, #20921, #30065, #17887, #8333, #33124 ),
 .UNSPECIFIED., .F., .F.,
 ( 4, 2, 4 ),
 ( 0.000000000000000000, 0.5000000000000000000, 1.000000000000000000 ),
 .UNSPECIFIED. ) ;
#31623 = CARTESIAN_POINT ( 'NONE',  ( -3.246717519899657400, 37.21789761807042396, 17.42190598798395484 ) ) ;
#31624 = ORIENTED_EDGE ( 'NONE', *, *, #19332, .F. ) ;
#31625 = CARTESIAN_POINT ( 'NONE',  ( -27.32938361780223957, -2.673874545957628079, -16.12352731284545726 ) ) ;
#31626 = CIRCLE ( 'NONE', #7604, 1.000000000000000000 ) ;
#31627 = CIRCLE ( 'NONE', #13462, 0.5000000000000004441 ) ;
#31628 = CARTESIAN_POINT ( 'NONE',  ( -15.47112132963103726, 15.31948306975548491, 19.27171037444150770 ) ) ;
#31629 = EDGE_LOOP ( 'NONE', ( #28273, #25624, #12674, #37223, #35851 ) ) ;
#31630 = DIRECTION ( 'NONE',  ( -0.000000000000000000, -0.000000000000000000, -1.000000000000000000 ) ) ;
#31631 = FACE_OUTER_BOUND ( 'NONE', #35211, .T. ) ;
#31632 = AXIS2_PLACEMENT_3D ( 'NONE', #34837, #16555, #3748 ) ;
#31633 = CARTESIAN_POINT ( 'NONE',  ( -28.60302894850194022, 1.758667520871832757, -8.791322179575384865 ) ) ;
#31634 = CARTESIAN_POINT ( 'NONE',  ( 20.37979243436083010, -8.235259509822993707, -24.27245371426751674 ) ) ;
#31636 = VECTOR ( 'NONE', #16036, 999.9999999999998863 ) ;
#31635 = CARTESIAN_POINT ( 'NONE',  ( 15.00437666251104218, -28.61930095463399581, 12.14047268033097460 ) ) ;
#31637 = ORIENTED_EDGE ( 'NONE', *, *, #25378, .F. ) ;
#31638 = EDGE_CURVE ( 'NONE', #26640, #21617, #22235, .T. ) ;
#31639 = ORIENTED_EDGE ( 'NONE', *, *, #892, .T. ) ;
#31640 = EDGE_CURVE ( 'NONE', #39512, #1450, #37882, .T. ) ;
#31641 = DIRECTION ( 'NONE',  ( 0.000000000000000000, 0.000000000000000000, 1.000000000000000000 ) ) ;
#31642 = CARTESIAN_POINT ( 'NONE',  ( -15.42150907995254983, 26.76352410258160930, -5.000000000000001776 ) ) ;
#31643 = PLANE ( 'NONE',  #33103 ) ;
#31644 = ORIENTED_EDGE ( 'NONE', *, *, #23863, .T. ) ;
#31645 = CARTESIAN_POINT ( 'NONE',  ( -1.130164101217176365, 22.80556646834144630, -22.98960577978414577 ) ) ;
#31646 = CARTESIAN_POINT ( 'NONE',  ( -19.34689456777905292, 35.00980436007201746, 10.00000000000000000 ) ) ;
#31647 = DIRECTION ( 'NONE',  ( -0.5720614028176770338, 0.4156269377774552409, 0.7071067811865524577 ) ) ;
#31648 = B_SPLINE_CURVE_WITH_KNOTS ( 'NONE', 3,
 ( #14863, #24002, #32963, #30509 ),
 .UNSPECIFIED., .F., .F.,
 ( 4, 4 ),
 ( 0.000000000000000000, 0.1333333595060078314 ),
 .UNSPECIFIED. ) ;
#31649 = AXIS2_PLACEMENT_3D ( 'NONE', #25404, #21962, #9974 ) ;
#31650 = LINE ( 'NONE', #10118, #30570 ) ;
#31651 = DIRECTION ( 'NONE',  ( -0.000000000000000000, -0.000000000000000000, -1.000000000000000000 ) ) ;
#31652 = CARTESIAN_POINT ( 'NONE',  ( 2.552861293176707402, 8.084864722426264194, 11.00000000000000355 ) ) ;
#31653 = CIRCLE ( 'NONE', #30995, 1.000000000000000888 ) ;
#31654 = CARTESIAN_POINT ( 'NONE',  ( 8.928096088923819451, 19.18392227192688182, -25.99240570989386256 ) ) ;
#31655 = LINE ( 'NONE', #38147, #20509 ) ;
#31656 = AXIS2_PLACEMENT_3D ( 'NONE', #18986, #24483, #12488 ) ;
#31657 = ORIENTED_EDGE ( 'NONE', *, *, #37797, .F. ) ;
#31659 = CARTESIAN_POINT ( 'NONE',  ( -12.22403502154109667, 14.67264973081049284, 10.83333333333333037 ) ) ;
#31658 = CARTESIAN_POINT ( 'NONE',  ( -19.04214505569463967, 11.35732863687608152, -19.06679702495384277 ) ) ;
#31660 = CARTESIAN_POINT ( 'NONE',  ( -18.68934290553424304, 29.94321432092579727, 11.00000000000000000 ) ) ;
#31661 = CARTESIAN_POINT ( 'NONE',  ( 15.49155713431803960, -26.66867858187293550, -6.415952216431528576 ) ) ;
#31662 = LINE ( 'NONE', #28210, #2913 ) ;
#31663 = CARTESIAN_POINT ( 'NONE',  ( 11.13181036404293067, 17.79423202622817968, -26.21918479596937601 ) ) ;
#31664 = CARTESIAN_POINT ( 'NONE',  ( 13.28992586503610163, -18.25382200079949513, -20.55760979252977094 ) ) ;
#31665 = ADVANCED_FACE ( 'NONE', ( #30804 ), #8056, .T. ) ;
#31666 = DIRECTION ( 'NONE',  ( 0.7431448254773953543, 0.6691306063588570163, 0.000000000000000000 ) ) ;
#31667 = CARTESIAN_POINT ( 'NONE',  ( -21.80867257259097514, -23.11172725429855390, -13.03247554641362349 ) ) ;
#31668 = CARTESIAN_POINT ( 'NONE',  ( 8.497644768481743327, -25.32189558139016228, -5.000000000000002665 ) ) ;
#31669 = CARTESIAN_POINT ( 'NONE',  ( 11.07485645340150171, 17.25102576792224340, -29.99999999999999289 ) ) ;
#31670 = CARTESIAN_POINT ( 'NONE',  ( 25.87580467091643399, -17.52732614752431672, -14.74065523776432052 ) ) ;
#31671 = CARTESIAN_POINT ( 'NONE',  ( 8.336672018935502138, 10.01592710129210850, 10.49999999999999822 ) ) ;
#31672 = CARTESIAN_POINT ( 'NONE',  ( 5.517564457587568860, 36.12194934191559526, 10.96580508970282608 ) ) ;
#31673 = ORIENTED_EDGE ( 'NONE', *, *, #19587, .T. ) ;
#31674 = CARTESIAN_POINT ( 'NONE',  ( -6.253143773029494312, 26.59490657384560208, -17.73706128625773459 ) ) ;
#31675 = CARTESIAN_POINT ( 'NONE',  ( -13.87104230352202094, 20.53934056656885687, 7.500000000000004441 ) ) ;
#31676 = ORIENTED_EDGE ( 'NONE', *, *, #33999, .F. ) ;
#31677 = CARTESIAN_POINT ( 'NONE',  ( 30.92038317698504457, -0.05869178374276579069, -5.000000000000000000 ) ) ;
#31678 = CARTESIAN_POINT ( 'NONE',  ( 8.927394655428274817, 11.06314620770945290, 7.500000000000000888 ) ) ;
#31679 = CARTESIAN_POINT ( 'NONE',  ( -27.71565130972192392, -3.171757977838550513, 19.66345542862528717 ) ) ;
#31680 = ORIENTED_EDGE ( 'NONE', *, *, #5943, .F. ) ;
#31681 = CARTESIAN_POINT ( 'NONE',  ( -20.68821937854897541, 0.9221346313300146091, -27.45318776198465471 ) ) ;
#31682 = CARTESIAN_POINT ( 'NONE',  ( -7.530592408761007661, 11.28437794979203090, 10.00000000000000000 ) ) ;
#31683 = ORIENTED_EDGE ( 'NONE', *, *, #25025, .T. ) ;
#31684 = CARTESIAN_POINT ( 'NONE',  ( 33.80886038580988640, -8.069990905591543751, -9.383811014428410147 ) ) ;
#31685 = VECTOR ( 'NONE', #28380, 1000.000000000000000 ) ;
#31686 = AXIS2_PLACEMENT_3D ( 'NONE', #1304, #38475, #27089 ) ;
#31687 = ORIENTED_EDGE ( 'NONE', *, *, #30110, .F. ) ;
#31688 = APPLICATION_PROTOCOL_DEFINITION ( 'draft international standard', 'automotive_design', 1998, #6209 ) ;
#31689 = CARTESIAN_POINT ( 'NONE',  ( 17.34253826607195847, 27.32041144403996213, 11.55979286843935050 ) ) ;
#31690 = AXIS2_PLACEMENT_3D ( 'NONE', #1931, #22839, #14307 ) ;
#31691 = DIRECTION ( 'NONE',  ( -0.5877852522924690293, 0.8090169943749503378, 0.000000000000000000 ) ) ;
#31692 = CARTESIAN_POINT ( 'NONE',  ( -0.7619526660190145684, 37.48079653017162371, 7.455686640544901600 ) ) ;
#31693 = EDGE_CURVE ( 'NONE', #5336, #24444, #16155, .T. ) ;
#31694 = CARTESIAN_POINT ( 'NONE',  ( -4.159699369156335536, 34.84843100105939584, 18.87996532025786323 ) ) ;
#31695 = VECTOR ( 'NONE', #1771, 1000.000000000000000 ) ;
#31696 = CYLINDRICAL_SURFACE ( 'NONE', #18797, 0.5000000000000004441 ) ;
#31697 = VERTEX_POINT ( 'NONE', #12308 ) ;
#31698 = CARTESIAN_POINT ( 'NONE',  ( 6.245935934162172742, 19.56982954529273400, -30.00000000000000711 ) ) ;
#31699 = FACE_OUTER_BOUND ( 'NONE', #30598, .T. ) ;
#31700 = CARTESIAN_POINT ( 'NONE',  ( 12.67493120981675325, 14.45362483784307983, 10.49999999999999645 ) ) ;
#31701 = CARTESIAN_POINT ( 'NONE',  ( 13.75357712579410574, 15.21937127477098350, -30.00000000000000711 ) ) ;
#31702 = CARTESIAN_POINT ( 'NONE',  ( 10.02000509642858361, 34.97447782610390732, -4.999999999999999112 ) ) ;
#31703 = ORIENTED_EDGE ( 'NONE', *, *, #17845, .F. ) ;
#31704 = CARTESIAN_POINT ( 'NONE',  ( 15.84394465367380178, -26.31127309132897452, -8.735524027787771928 ) ) ;
#31705 = CARTESIAN_POINT ( 'NONE',  ( 4.672335726383267662, 24.36080358023194137, 21.00000000000000000 ) ) ;
#31706 = LINE ( 'NONE', #37209, #21277 ) ;
#31707 = ADVANCED_FACE ( 'NONE', ( #31000 ), #28143, .F. ) ;
#31708 = CIRCLE ( 'NONE', #568, 1.000000000000002665 ) ;
#31709 = ORIENTED_EDGE ( 'NONE', *, *, #3564, .F. ) ;
#31711 = AXIS2_PLACEMENT_3D ( 'NONE', #29482, #36186, #4902 ) ;
#31710 = CARTESIAN_POINT ( 'NONE',  ( -13.21411722169975711, 22.22692963839663705, -16.44518550108498189 ) ) ;
#31712 = CARTESIAN_POINT ( 'NONE',  ( -34.38615473478483153, -15.96524117250080010, 16.87380292611443622 ) ) ;
#31713 = CARTESIAN_POINT ( 'NONE',  ( 10.26885880249883165, -19.65294855164837884, -22.76732940879269051 ) ) ;
#31714 = EDGE_CURVE ( 'NONE', #27240, #18790, #20395, .T. ) ;
#31715 = DIRECTION ( 'NONE',  ( 1.000000000000000000, 0.000000000000000000, 0.000000000000000000 ) ) ;
#31716 = ORIENTED_EDGE ( 'NONE', *, *, #5810, .T. ) ;
#31717 = VERTEX_POINT ( 'NONE', #320 ) ;
#31718 = AXIS2_PLACEMENT_3D ( 'NONE', #13654, #38036, #11023 ) ;
#31719 = CARTESIAN_POINT ( 'NONE',  ( -12.40929423282409694, 26.94941001123947544, -13.25802102404320060 ) ) ;
#31720 = CARTESIAN_POINT ( 'NONE',  ( -75.15099915297791711, 43.38844959084113384, 0.000000000000000000 ) ) ;
#31721 = FACE_BOUND ( 'NONE', #4351, .T. ) ;
#31722 = EDGE_CURVE ( 'NONE', #39789, #13016, #6792, .T. ) ;
#31723 = CARTESIAN_POINT ( 'NONE',  ( -33.27180366187747751, -8.208870852378092664, -10.27506301637745167 ) ) ;
#31724 = CYLINDRICAL_SURFACE ( 'NONE', #25474, 0.5000000000000011102 ) ;
#31725 = ORIENTED_EDGE ( 'NONE', *, *, #35131, .F. ) ;
#31726 = CARTESIAN_POINT ( 'NONE',  ( 30.75747790117273794, 0.1077116562829361218, -4.999999999999999112 ) ) ;
#31727 = CARTESIAN_POINT ( 'NONE',  ( 14.19304739008519256, 26.58586953448655521, 10.94611345180491035 ) ) ;
#31728 = CARTESIAN_POINT ( 'NONE',  ( 14.97277451176449325, 21.48159783397873923, 10.49999999999999822 ) ) ;
#31729 = ORIENTED_EDGE ( 'NONE', *, *, #3997, .F. ) ;
#31730 = CARTESIAN_POINT ( 'NONE',  ( -30.20906327819625048, -0.01427245983082933191, -8.766269380263043587 ) ) ;
#31731 = CARTESIAN_POINT ( 'NONE',  ( 75.15099915297797395, 43.38844959084117647, -5.000000000000000000 ) ) ;
#31732 = ORIENTED_EDGE ( 'NONE', *, *, #18761, .F. ) ;
#31733 = CARTESIAN_POINT ( 'NONE',  ( 32.71662871600790368, -3.117337333226495755, -8.171977234651780719 ) ) ;
#31734 = CARTESIAN_POINT ( 'NONE',  ( -13.42604558747169285, 21.08886574588681384, 7.000000000000000000 ) ) ;
#31735 = CARTESIAN_POINT ( 'NONE',  ( 29.75773323547294424, -22.90830468393526687, 16.87380292611442556 ) ) ;
#31736 = ORIENTED_EDGE ( 'NONE', *, *, #11770, .T. ) ;
#31737 = CARTESIAN_POINT ( 'NONE',  ( -14.21869892593723428, 30.05184351263790532, 16.30093088680186497 ) ) ;
#31738 = EDGE_CURVE ( 'NONE', #25686, #23343, #12504, .T. ) ;
#31739 = EDGE_CURVE ( 'NONE', #11008, #23024, #33365, .T. ) ;
#31740 = DIRECTION ( 'NONE',  ( 0.000000000000000000, 0.000000000000000000, 1.000000000000000000 ) ) ;
#31741 = ADVANCED_FACE ( 'NONE', ( #13091 ), #25480, .F. ) ;
#31742 = CARTESIAN_POINT ( 'NONE',  ( -1.254079983865611370, 28.18681535329822196, 20.99999999999999645 ) ) ;
#31743 = AXIS2_PLACEMENT_3D ( 'NONE', #26459, #35613, #11033 ) ;
#31744 = VECTOR ( 'NONE', #36718, 1000.000000000000114 ) ;
#31745 = FACE_OUTER_BOUND ( 'NONE', #7853, .T. ) ;
#31746 = CARTESIAN_POINT ( 'NONE',  ( 10.14060191828659541, 25.26915018278934610, 11.00000000000000000 ) ) ;
#31747 = AXIS2_PLACEMENT_3D ( 'NONE', #10765, #20114, #14008 ) ;
#31748 = PRODUCT_DEFINITION_SHAPE ( 'NONE', 'NONE',  #40201 ) ;
#31749 = FACE_BOUND ( 'NONE', #31492, .T. ) ;
#31750 = CARTESIAN_POINT ( 'NONE',  ( 16.24129362379723673, 27.01431713451477279, 15.13084544680213739 ) ) ;
#31751 = CARTESIAN_POINT ( 'NONE',  ( -21.91354840350972211, 9.539350162456797122, -12.87506386756524179 ) ) ;
#31752 = CARTESIAN_POINT ( 'NONE',  ( 15.40455633798288204, -19.17866944239923299, -20.04336763641729036 ) ) ;
#31753 = FACE_OUTER_BOUND ( 'NONE', #18607, .T. ) ;
#31754 = EDGE_CURVE ( 'NONE', #4170, #24423, #3359, .T. ) ;
#31755 = CARTESIAN_POINT ( 'NONE',  ( 14.45110082695830833, 25.20033142108280089, -11.58180078429156090 ) ) ;
#31756 = ORIENTED_EDGE ( 'NONE', *, *, #22897, .F. ) ;
#31757 = CARTESIAN_POINT ( 'NONE',  ( -15.85862229823199776, 25.25472105652747246, -5.000000000000000000 ) ) ;
#31758 = CARTESIAN_POINT ( 'NONE',  ( -25.62037635619380893, -16.85925998830651906, 20.69868183039781684 ) ) ;
#31759 = EDGE_CURVE ( 'NONE', #39078, #2539, #37881, .T. ) ;
#31760 = DIRECTION ( 'NONE',  ( 0.000000000000000000, 0.000000000000000000, 1.000000000000000000 ) ) ;
#31761 = CARTESIAN_POINT ( 'NONE',  ( 12.68336450221132417, 21.00970290476725211, -18.45743704410757857 ) ) ;
#31762 = ORIENTED_EDGE ( 'NONE', *, *, #3462, .F. ) ;
#31763 = CARTESIAN_POINT ( 'NONE',  ( 22.90052353346136371, -11.74428243424502760, -19.63336109330355228 ) ) ;
#31764 = FACE_OUTER_BOUND ( 'NONE', #4804, .T. ) ;
#31765 = ORIENTED_EDGE ( 'NONE', *, *, #31738, .F. ) ;
#31767 = CARTESIAN_POINT ( 'NONE',  ( 7.748046928843868031, 9.655464433119462342, 7.102474990965862212 ) ) ;
#31766 = CARTESIAN_POINT ( 'NONE',  ( -14.75109696978639029, 26.35784808731213857, -9.678683898009220243 ) ) ;
#31768 = CARTESIAN_POINT ( 'NONE',  ( -15.44690521824878537, -25.79975055938752604, -10.14031905184057791 ) ) ;
#31769 = DIRECTION ( 'NONE',  ( -0.3090169943749560000, -0.9510565162951507556, -3.469446951953612611E-15 ) ) ;
#31770 = VECTOR ( 'NONE', #3567, 1000.000000000000000 ) ;
#31771 = ORIENTED_EDGE ( 'NONE', *, *, #14135, .F. ) ;
#31772 = CARTESIAN_POINT ( 'NONE',  ( -34.54285066864272835, -16.78341526201209533, -5.435878295993979314 ) ) ;
#31773 = CARTESIAN_POINT ( 'NONE',  ( -10.69804542477608855, -21.08478606119448884, -19.58466021002672974 ) ) ;
#31774 = DIRECTION ( 'NONE',  ( 0.000000000000000000, 0.000000000000000000, 1.000000000000000000 ) ) ;
#31775 = CARTESIAN_POINT ( 'NONE',  ( 15.90807616341559338, 22.25326793540537906, -10.72615760417953013 ) ) ;
#31776 = VERTEX_POINT ( 'NONE', #37492 ) ;
#31777 = CARTESIAN_POINT ( 'NONE',  ( 26.66934055787902835, 2.909074036114203121, -11.70011843583559497 ) ) ;
#31778 = CARTESIAN_POINT ( 'NONE',  ( -7.713869163866014844, 10.18146832927085299, 9.500000000000000000 ) ) ;
#31779 = LINE ( 'NONE', #22420, #6302 ) ;
#31780 = DIRECTION ( 'NONE',  ( 1.000000000000000000, 0.000000000000000000, 0.000000000000000000 ) ) ;
#31781 = ORIENTED_EDGE ( 'NONE', *, *, #23412, .T. ) ;
#31782 = CARTESIAN_POINT ( 'NONE',  ( -20.50193171233730993, 0.1922071591807814339, -29.33613531814199149 ) ) ;
#31783 = CARTESIAN_POINT ( 'NONE',  ( 20.99165470567395175, 0.5836903346832758022, -26.20505728122213895 ) ) ;
#31784 = CARTESIAN_POINT ( 'NONE',  ( 20.32014898129569147, -22.75198622026958617, 19.66345542862527651 ) ) ;
#31785 = VERTEX_POINT ( 'NONE', #21451 ) ;
#31786 = CARTESIAN_POINT ( 'NONE',  ( -12.33616729053609795, -27.99489201236593061, -4.999999999999999112 ) ) ;
#31787 = DIRECTION ( 'NONE',  ( 0.000000000000000000, -0.000000000000000000, -1.000000000000000000 ) ) ;
#31788 = VERTEX_POINT ( 'NONE', #6005 ) ;
#31789 = ADVANCED_FACE ( 'NONE', ( #9670 ), #28335, .F. ) ;
#31790 = LINE ( 'NONE', #29899, #21057 ) ;
#31791 = DIRECTION ( 'NONE',  ( -0.7431448254773862505, 0.6691306063588670083, 0.000000000000000000 ) ) ;
#31792 = CARTESIAN_POINT ( 'NONE',  ( -6.811226782241547539, 35.33967249274200384, 9.500000000000000000 ) ) ;
#31793 = CARTESIAN_POINT ( 'NONE',  ( 12.77090408390491305, 15.39748370681878775, 12.00000000000000000 ) ) ;
#31794 = ORIENTED_EDGE ( 'NONE', *, *, #28630, .F. ) ;
#31795 = FACE_OUTER_BOUND ( 'NONE', #20745, .T. ) ;
#31796 = DIRECTION ( 'NONE',  ( 0.000000000000000000, 0.000000000000000000, 1.000000000000000000 ) ) ;
#31797 = CARTESIAN_POINT ( 'NONE',  ( 26.92080679176510571, -24.85520046368381131, -7.585400692263990940 ) ) ;
#31798 = CIRCLE ( 'NONE', #18189, 15.00000000000000000 ) ;
#31799 = CARTESIAN_POINT ( 'NONE',  ( -3.229437847141423124, 24.50739181907689712, 12.00000000000000000 ) ) ;
#31800 = LINE ( 'NONE', #29158, #17741 ) ;
#31801 = CARTESIAN_POINT ( 'NONE',  ( 10.55968626961773360, 17.57118088696260827, -29.33920240098544951 ) ) ;
#31802 = CARTESIAN_POINT ( 'NONE',  ( -4.678013043399448456, 44.50832101651065642, 7.000000000000000000 ) ) ;
#31803 = ORIENTED_EDGE ( 'NONE', *, *, #11386, .F. ) ;
#31805 = CARTESIAN_POINT ( 'NONE',  ( -3.503793317224518145, 8.420815634768723967, 7.499999999999997335 ) ) ;
#31804 = CARTESIAN_POINT ( 'NONE',  ( -17.73668911492254807, 19.59045636488301767, -7.397010546184955793 ) ) ;
#31806 = CARTESIAN_POINT ( 'NONE',  ( 13.01373512357458928, 15.56386679243127347, 10.94387467463492847 ) ) ;
#31807 = CARTESIAN_POINT ( 'NONE',  ( 15.41329945644580413, -26.72332452139117720, -5.000000000000000000 ) ) ;
#31808 = CARTESIAN_POINT ( 'NONE',  ( 13.47830981910550641, 21.58612669357077607, 7.000000000000000000 ) ) ;
#31809 = CARTESIAN_POINT ( 'NONE',  ( 11.07256710390407051, 17.50279746095970523, -27.44776494551608792 ) ) ;
#31810 = ORIENTED_EDGE ( 'NONE', *, *, #29002, .T. ) ;
#31811 = CARTESIAN_POINT ( 'NONE',  ( 14.73787879266534873, 25.39503920881744392, -10.65324680268567725 ) ) ;
#31812 = VERTEX_POINT ( 'NONE', #24698 ) ;
#31814 = CARTESIAN_POINT ( 'NONE',  ( 12.99377146717206344, 26.19620116591418224, 9.500000000000000000 ) ) ;
#31813 = CARTESIAN_POINT ( 'NONE',  ( -11.43760958252774884, 18.47761077602904223, -23.84654567625729626 ) ) ;
#31815 = CARTESIAN_POINT ( 'NONE',  ( -12.97980758920870592, -23.09007905854067744, -15.45264339162509515 ) ) ;
#31816 = CARTESIAN_POINT ( 'NONE',  ( -29.72906145568333258, -25.76693493179011085, 13.32518128616621667 ) ) ;
#31817 = CIRCLE ( 'NONE', #37011, 0.5000000000000004441 ) ;
#31818 = CARTESIAN_POINT ( 'NONE',  ( -18.79189612092352135, -12.94303005244327132, -23.00170733529830258 ) ) ;
#31819 = CARTESIAN_POINT ( 'NONE',  ( -1.766708854211077595, -20.47917438257665879, -30.00000000000000355 ) ) ;
#31820 = CARTESIAN_POINT ( 'NONE',  ( 13.81705425458364722, 22.18564081078588046, -15.49648774365130244 ) ) ;
#31821 = ORIENTED_EDGE ( 'NONE', *, *, #8830, .F. ) ;
#31822 = CARTESIAN_POINT ( 'NONE',  ( 18.53824370654135478, 9.487311751210160793, -25.50586965412942320 ) ) ;
#31823 = DIRECTION ( 'NONE',  ( 1.000000000000000000, 0.000000000000000000, 0.000000000000000000 ) ) ;
#31824 = CARTESIAN_POINT ( 'NONE',  ( -14.97058623676950262, 26.66112013780927015, 16.87380292611441490 ) ) ;
#31825 = ORIENTED_EDGE ( 'NONE', *, *, #23489, .T. ) ;
#31826 = CARTESIAN_POINT ( 'NONE',  ( -20.28315073442723460, -3.046437751679770933, -30.00000000000000000 ) ) ;
#31827 = CARTESIAN_POINT ( 'NONE',  ( -24.37528612864471711, 1.300641855047817153, 19.27171037444580648 ) ) ;
#31828 = ORIENTED_EDGE ( 'NONE', *, *, #2599, .T. ) ;
#31829 = B_SPLINE_CURVE_WITH_KNOTS ( 'NONE', 3,
 ( #24795, #21546, #24997, #13194, #19294, #31692, #27846, #36993 ),
 .UNSPECIFIED., .F., .F.,
 ( 4, 2, 2, 4 ),
 ( 2.168404344971008868E-19, 0.0004726692273637090745, 0.0007090038410455647231, 0.0009453384547274204259 ),
 .UNSPECIFIED. ) ;
#31830 = CARTESIAN_POINT ( 'NONE',  ( 20.38753357181594694, -16.19769905861743098, 20.99999999999999645 ) ) ;
#31831 = DIRECTION ( 'NONE',  ( -0.1045284632676569819, -0.9945218953682730678, 0.000000000000000000 ) ) ;
#31832 = AXIS2_PLACEMENT_3D ( 'NONE', #18517, #9170, #34358 ) ;
#31833 = CARTESIAN_POINT ( 'NONE',  ( 34.73373506214407769, -15.22407143656519679, -6.703790208019304586 ) ) ;
#31834 = CARTESIAN_POINT ( 'NONE',  ( 26.42723928173402470, -27.79046472072450413, 12.14047268033097104 ) ) ;
#31835 = EDGE_CURVE ( 'NONE', #11673, #17087, #6106, .T. ) ;
#31836 = ORIENTED_EDGE ( 'NONE', *, *, #15348, .T. ) ;
#31837 = ORIENTED_EDGE ( 'NONE', *, *, #3147, .T. ) ;
#31838 = PLANE ( 'NONE',  #4131 ) ;
#31839 = CARTESIAN_POINT ( 'NONE',  ( -15.41558956984166251, 26.78481017248024898, -5.000000000000000000 ) ) ;
#31840 = AXIS2_PLACEMENT_3D ( 'NONE', #33768, #15060, #3070 ) ;
#31841 = DIRECTION ( 'NONE',  ( 0.000000000000000000, 0.000000000000000000, 1.000000000000000000 ) ) ;
#31842 = ORIENTED_EDGE ( 'NONE', *, *, #7631, .F. ) ;
#31843 = EDGE_CURVE ( 'NONE', #25686, #15880, #34680, .T. ) ;
#31844 = CARTESIAN_POINT ( 'NONE',  ( -1.517615944522816118, 30.16442793585677862, -15.68169713778068441 ) ) ;
#31845 = AXIS2_PLACEMENT_3D ( 'NONE', #28343, #3366, #15362 ) ;
#31846 = CARTESIAN_POINT ( 'NONE',  ( -1.829593030691901284E-15, 22.50000000000001066, -5.000000000000000000 ) ) ;
#31847 = CARTESIAN_POINT ( 'NONE',  ( 6.330070799514983193, 27.28854476845134513, 12.00000000000000000 ) ) ;
#31848 = EDGE_CURVE ( 'NONE', #33983, #31959, #39041, .T. ) ;
#31849 = DIRECTION ( 'NONE',  ( -0.3090169943749450643, 0.9510565162951543083, 0.000000000000000000 ) ) ;
#31850 = CARTESIAN_POINT ( 'NONE',  ( -14.49025312501840723, 21.64735187953135309, 10.83333333333333215 ) ) ;
#31851 = CARTESIAN_POINT ( 'NONE',  ( -4.211402178667006169, 32.38366924255629442, 12.00000000000000000 ) ) ;
#31852 = CARTESIAN_POINT ( 'NONE',  ( 9.367770739272080149, 18.53333684161963646, -27.31848943577234934 ) ) ;
#31853 = FACE_OUTER_BOUND ( 'NONE', #23298, .T. ) ;
#31854 = VERTEX_POINT ( 'NONE', #31989 ) ;
#31856 = CARTESIAN_POINT ( 'NONE',  ( 13.14827996435953494, 25.72067290776660897, 10.50000000000000000 ) ) ;
#31855 = CARTESIAN_POINT ( 'NONE',  ( -18.38058839721481874, 11.97145855736538245, -20.11878731179081825 ) ) ;
#31857 = CARTESIAN_POINT ( 'NONE',  ( -4.331888854854360815, 42.14502281367542480, 11.00000000000000000 ) ) ;
#31858 = CARTESIAN_POINT ( 'NONE',  ( 13.42465078840814918, -23.62789290738457382, -14.47165382363914787 ) ) ;
#31859 = DIRECTION ( 'NONE',  ( 0.4156269377774525209, 0.5720614028176911336, -0.7071067811865425767 ) ) ;
#31860 = CARTESIAN_POINT ( 'NONE',  ( 10.94214493613176664, 17.33550160327741096, -29.99999999999999289 ) ) ;
#31861 = CARTESIAN_POINT ( 'NONE',  ( -13.47223693944937040, 18.09844039693852125, -29.99999999999999645 ) ) ;
#31862 = CARTESIAN_POINT ( 'NONE',  ( -24.51458563001630964, -11.16205237993636956, 23.00000000000000711 ) ) ;
#31863 = CARTESIAN_POINT ( 'NONE',  ( -22.97994382251033585, -24.34209009305979166, -11.18594617276381697 ) ) ;
#31864 = CARTESIAN_POINT ( 'NONE',  ( 8.487318810465147578, -25.30172221365172192, -5.955506841159929010 ) ) ;
#31865 = CARTESIAN_POINT ( 'NONE',  ( 11.26119111163083630, 17.51761337186505685, -26.84302999491309194 ) ) ;
#31866 = CARTESIAN_POINT ( 'NONE',  ( 30.53998965538356103, -22.06133822602150474, -7.552213228032163883 ) ) ;
#31867 = EDGE_CURVE ( 'NONE', #6401, #13649, #34839, .T. ) ;
#31868 = DIRECTION ( 'NONE',  ( 0.000000000000000000, 0.000000000000000000, 1.000000000000000000 ) ) ;
#31869 = LINE ( 'NONE', #28823, #30658 ) ;
#31870 = ADVANCED_FACE ( 'NONE', ( #39242 ), #16355, .F. ) ;
#31871 = VERTEX_POINT ( 'NONE', #10253 ) ;
#31872 = B_SPLINE_CURVE_WITH_KNOTS ( 'NONE', 3,
 ( #21584, #2704, #21192, #33985 ),
 .UNSPECIFIED., .F., .F.,
 ( 4, 4 ),
 ( 0.000000000000000000, 1.000000000000000000 ),
 .UNSPECIFIED. ) ;
#31873 = CARTESIAN_POINT ( 'NONE',  ( -5.884614315209530488, 19.64670892508010169, -29.99999999999997868 ) ) ;
#31874 = AXIS2_PLACEMENT_3D ( 'NONE', #38996, #7302, #7508 ) ;
#31875 = DIRECTION ( 'NONE',  ( 0.000000000000000000, 0.000000000000000000, 1.000000000000000000 ) ) ;
#31876 = ORIENTED_EDGE ( 'NONE', *, *, #37381, .T. ) ;
#31877 = CARTESIAN_POINT ( 'NONE',  ( 22.74115952922136330, 0.5763562226926195464, -21.61272164397127682 ) ) ;
#31878 = AXIS2_PLACEMENT_3D ( 'NONE', #35600, #35396, #17321 ) ;
#31879 = CARTESIAN_POINT ( 'NONE',  ( 0.5000000000000001110, 37.00000000000000711, 9.000000000000001776 ) ) ;
#31880 = LINE ( 'NONE', #4041, #23253 ) ;
#31881 = EDGE_LOOP ( 'NONE', ( #7844, #24696 ) ) ;
#31882 = CARTESIAN_POINT ( 'NONE',  ( -29.50026895737458688, 0.1576476882857581474, -10.18295560989503734 ) ) ;
#31883 = CYLINDRICAL_SURFACE ( 'NONE', #9247, 1.000000000000000888 ) ;
#31884 = VERTEX_POINT ( 'NONE', #20772 ) ;
#31885 = CARTESIAN_POINT ( 'NONE',  ( 35.30405009085131240, -9.553221813830631959, -6.305931249553304418 ) ) ;
#31886 = ORIENTED_EDGE ( 'NONE', *, *, #22508, .F. ) ;
#31887 = AXIS2_PLACEMENT_3D ( 'NONE', #9551, #13178, #407 ) ;
#31888 = DIRECTION ( 'NONE',  ( 0.9781476007338072431, 0.2079116908177517375, 0.000000000000000000 ) ) ;
#31889 = DIRECTION ( 'NONE',  ( -0.000000000000000000, -0.000000000000000000, -1.000000000000000000 ) ) ;
#31890 = PLANE ( 'NONE',  #3345 ) ;
#31891 = EDGE_CURVE ( 'NONE', #33301, #7705, #11973, .T. ) ;
#31892 = CARTESIAN_POINT ( 'NONE',  ( 10.90977822005762832, 28.29415442298315142, 19.27171037444158586 ) ) ;
#31893 = DIRECTION ( 'NONE',  ( -0.000000000000000000, -0.000000000000000000, -1.000000000000000000 ) ) ;
#31894 = ORIENTED_EDGE ( 'NONE', *, *, #1592, .T. ) ;
#31895 = CARTESIAN_POINT ( 'NONE',  ( -4.448583892168122667, 20.01379199642233075, -29.99999999999998579 ) ) ;
#31896 = DIRECTION ( 'NONE',  ( 1.000000000000000000, 0.000000000000000000, 0.000000000000000000 ) ) ;
#31897 = CARTESIAN_POINT ( 'NONE',  ( -6.354454053420248272, 35.54304081427989814, 9.000000000000001776 ) ) ;
#31898 = CARTESIAN_POINT ( 'NONE',  ( 18.12927444247487685, 18.97622154095044777, -5.957654057152589999 ) ) ;
#31899 = CARTESIAN_POINT ( 'NONE',  ( 5.857883788898597288, 20.22416296293512872, -26.42044690542252638 ) ) ;
#31900 = AXIS2_PLACEMENT_3D ( 'NONE', #28001, #37149, #175 ) ;
#31901 = ORIENTED_EDGE ( 'NONE', *, *, #14006, .T. ) ;
#31902 = CARTESIAN_POINT ( 'NONE',  ( -0.7344975573282397363, 36.24516302788250499, 13.00000000000000178 ) ) ;
#31903 = CARTESIAN_POINT ( 'NONE',  ( 16.28181498793477999, -26.61367711139261161, -7.795649509280883294 ) ) ;
#31904 = LINE ( 'NONE', #19720, #22353 ) ;
#31905 = CARTESIAN_POINT ( 'NONE',  ( 14.26584437371809777, 27.13525491562438319, 13.00000000000000178 ) ) ;
#31906 = ORIENTED_EDGE ( 'NONE', *, *, #14466, .F. ) ;
#31907 = CARTESIAN_POINT ( 'NONE',  ( -15.29470497349542235, 26.51477255901613361, -7.358185202849431228 ) ) ;
#31908 = CARTESIAN_POINT ( 'NONE',  ( -25.49851591039071863, -25.57752154475369366, 16.87380292611442201 ) ) ;
#31909 = CARTESIAN_POINT ( 'NONE',  ( 9.392528018862558170, -18.45111944239248913, -27.46388755805442372 ) ) ;
#31910 = CIRCLE ( 'NONE', #33874, 1.000000000000000000 ) ;
#31911 = DIRECTION ( 'NONE',  ( 0.000000000000000000, 0.000000000000000000, 1.000000000000000000 ) ) ;
#31912 = EDGE_CURVE ( 'NONE', #8749, #14728, #4154, .T. ) ;
#31913 = ORIENTED_EDGE ( 'NONE', *, *, #7352, .T. ) ;
#31914 = ORIENTED_EDGE ( 'NONE', *, *, #164, .F. ) ;
#31915 = CARTESIAN_POINT ( 'NONE',  ( -12.65601555930210509, 32.35306062433939900, -5.452413821557709817 ) ) ;
#31916 = CARTESIAN_POINT ( 'NONE',  ( -6.557822374958137246, 35.99981354310120452, 10.63089969389957012 ) ) ;
#31917 = FACE_BOUND ( 'NONE', #31051, .T. ) ;
#31918 = CARTESIAN_POINT ( 'NONE',  ( -30.08318636280791125, -7.404603725954973292, -13.95201704139118526 ) ) ;
#31919 = DIRECTION ( 'NONE',  ( 0.000000000000000000, 0.000000000000000000, 1.000000000000000000 ) ) ;
#31920 = EDGE_LOOP ( 'NONE', ( #29649, #18526, #21269, #39222, #4760 ) ) ;
#31921 = CARTESIAN_POINT ( 'NONE',  ( 30.04993021256226626, 0.1566486852560641796, -8.769524174311651876 ) ) ;
#31922 = DIRECTION ( 'NONE',  ( 1.000000000000000000, 0.000000000000000000, 0.000000000000000000 ) ) ;
#31923 = CARTESIAN_POINT ( 'NONE',  ( 13.05736835487433467, 16.11602540378438420, 10.49999999999999822 ) ) ;
#31924 = ORIENTED_EDGE ( 'NONE', *, *, #22163, .F. ) ;
#31925 = CARTESIAN_POINT ( 'NONE',  ( -21.71042592863056342, 0.7213194707694018382, -23.85327911821731206 ) ) ;
#31926 = CARTESIAN_POINT ( 'NONE',  ( -5.465749975257388371, 36.45564430483327811, 10.49999999999999822 ) ) ;
#31927 = ORIENTED_EDGE ( 'NONE', *, *, #7482, .T. ) ;
#31928 = CARTESIAN_POINT ( 'NONE',  ( 33.32260079917540452, -3.210191908071163169, -5.911986766794023573 ) ) ;
#31929 = DIRECTION ( 'NONE',  ( -0.000000000000000000, -0.000000000000000000, -1.000000000000000000 ) ) ;
#31930 = VECTOR ( 'NONE', #3915, 1000.000000000000114 ) ;
#31931 = CARTESIAN_POINT ( 'NONE',  ( 34.14640338304414513, -7.754617911606312752, 17.42190598798393353 ) ) ;
#31932 = VERTEX_POINT ( 'NONE', #16764 ) ;
#31933 = CARTESIAN_POINT ( 'NONE',  ( 3.468257360957521573, 38.22173125672342309, 16.30093088680195024 ) ) ;
#31934 = CARTESIAN_POINT ( 'NONE',  ( -10.81260707898136708, 32.90853150812170469, 7.000000000000000000 ) ) ;
#31935 = EDGE_CURVE ( 'NONE', #19575, #855, #2081, .T. ) ;
#31936 = CARTESIAN_POINT ( 'NONE',  ( 6.367390439426121596, 24.26983560722165834, 20.94377226548378346 ) ) ;
#31937 = CARTESIAN_POINT ( 'NONE',  ( -23.14043693410022229, 26.33379778550221673, 10.00000000000000000 ) ) ;
#31938 = EDGE_CURVE ( 'NONE', #34128, #30574, #22637, .T. ) ;
#31939 = AXIS2_PLACEMENT_3D ( 'NONE', #22526, #22331, #28634 ) ;
#31940 = DIRECTION ( 'NONE',  ( 0.000000000000000000, 0.000000000000000000, -1.000000000000000000 ) ) ;
#31941 = ADVANCED_FACE ( 'NONE', ( #28737 ), #1117, .F. ) ;
#31942 = VECTOR ( 'NONE', #595, 1000.000000000000000 ) ;
#31943 = DIRECTION ( 'NONE',  ( 0.000000000000000000, 0.000000000000000000, 1.000000000000000000 ) ) ;
#31944 = CARTESIAN_POINT ( 'NONE',  ( 24.77298340259215692, 8.359746025956967586, 15.13084544680224575 ) ) ;
#31945 = CARTESIAN_POINT ( 'NONE',  ( -19.39911238771444246, 7.131629512367122281, -27.14147998049999444 ) ) ;
#31946 = CARTESIAN_POINT ( 'NONE',  ( 21.24144353091755733, -26.22539287217877657, -9.006437966444934773 ) ) ;
#31947 = DIRECTION ( 'NONE',  ( 0.9781476007338042455, -0.2079116908177663370, -0.000000000000000000 ) ) ;
#31948 = VERTEX_POINT ( 'NONE', #14665 ) ;
#31949 = CARTESIAN_POINT ( 'NONE',  ( 11.17207643027059305, 18.14497318590918695, -24.99559416334685835 ) ) ;
#31950 = VERTEX_POINT ( 'NONE', #1317 ) ;
#31951 = CARTESIAN_POINT ( 'NONE',  ( -14.10408248735370407, 22.68866825637624274, -14.51867820061998060 ) ) ;
#31952 = CARTESIAN_POINT ( 'NONE',  ( -31.83642866623216605, -11.02236948596316424, 19.27171037444223956 ) ) ;
#31953 = DIRECTION ( 'NONE',  ( 0.000000000000000000, 0.000000000000000000, 1.000000000000000000 ) ) ;
#31954 = CARTESIAN_POINT ( 'NONE',  ( 11.22661243547084453, 17.72572647685119307, -26.22939125915132053 ) ) ;
#31955 = ORIENTED_EDGE ( 'NONE', *, *, #12343, .F. ) ;
#31956 = CARTESIAN_POINT ( 'NONE',  ( 29.30039860399171303, -16.15247984952398141, -12.89021756677838226 ) ) ;
#31957 = CARTESIAN_POINT ( 'NONE',  ( -0.6237384431625470071, 19.56555719779890978, 12.00000000000000000 ) ) ;
#31958 = EDGE_CURVE ( 'NONE', #34372, #4972, #31790, .T. ) ;
#31959 = VERTEX_POINT ( 'NONE', #36209 ) ;
#31961 = CARTESIAN_POINT ( 'NONE',  ( 8.014845354181460380, 9.820632123551975567, 7.338691926023214407 ) ) ;
#31960 = CARTESIAN_POINT ( 'NONE',  ( -10.79835490039502410, 17.42544872524608479, -29.99999999999999289 ) ) ;
#31962 = EDGE_CURVE ( 'NONE', #21971, #5904, #10020, .T. ) ;
#31963 = CARTESIAN_POINT ( 'NONE',  ( -12.44748226125696711, -21.44593556856202810, -18.38580773262598456 ) ) ;
#31964 = CARTESIAN_POINT ( 'NONE',  ( 12.74038105676654631, 14.56698729810771731, 10.49999999999999822 ) ) ;
#31965 = EDGE_CURVE ( 'NONE', #2211, #3294, #27547, .T. ) ;
#31966 = VECTOR ( 'NONE', #18961, 1000.000000000000000 ) ;
#31967 = ORIENTED_EDGE ( 'NONE', *, *, #575, .F. ) ;
#31968 = CARTESIAN_POINT ( 'NONE',  ( -26.66261548401102743, -11.00715225274686482, -16.66819200665372946 ) ) ;
#31969 = CARTESIAN_POINT ( 'NONE',  ( -14.06843317319044928, -25.79384935331063744, -9.249739353774602435 ) ) ;
#31970 = DIRECTION ( 'NONE',  ( 0.000000000000000000, 0.000000000000000000, 1.000000000000000000 ) ) ;
#31971 = CARTESIAN_POINT ( 'NONE',  ( 14.59202647793683738, 19.84686743550333432, -16.64054136931479633 ) ) ;
#31972 = ORIENTED_EDGE ( 'NONE', *, *, #797, .F. ) ;
#31973 = CARTESIAN_POINT ( 'NONE',  ( 25.22259539243878024, 3.759474034095959372, -13.70306588605936327 ) ) ;
#31974 = DIRECTION ( 'NONE',  ( -1.000000000000000000, 0.000000000000000000, 0.000000000000000000 ) ) ;
#31975 = AXIS2_PLACEMENT_3D ( 'NONE', #10225, #35018, #6764 ) ;
#31976 = CARTESIAN_POINT ( 'NONE',  ( -4.727507481117092070, 31.88885898370948269, 10.50000000000000000 ) ) ;
#31977 = ORIENTED_EDGE ( 'NONE', *, *, #31714, .T. ) ;
#31978 = CARTESIAN_POINT ( 'NONE',  ( -21.31112166252114903, 0.5185946039941641272, -24.98634476583432829 ) ) ;
#31979 = CARTESIAN_POINT ( 'NONE',  ( 21.33889498998111378, 0.2955338563558915776, -24.96187165485871162 ) ) ;
#31980 = CARTESIAN_POINT ( 'NONE',  ( 28.04602290581444635, -19.07745245555366864, 19.66345542862561047 ) ) ;
#31981 = ORIENTED_EDGE ( 'NONE', *, *, #23042, .F. ) ;
#31982 = CARTESIAN_POINT ( 'NONE',  ( -26.31271763591399804, -28.25584584496044727, -14.26382729546507555 ) ) ;
#31983 = EDGE_CURVE ( 'NONE', #21143, #17826, #38287, .T. ) ;
#31984 = AXIS2_PLACEMENT_3D ( 'NONE', #16365, #725, #35253 ) ;
#31985 = DIRECTION ( 'NONE',  ( -0.000000000000000000, -0.000000000000000000, -1.000000000000000000 ) ) ;
#31986 = ADVANCED_FACE ( 'NONE', ( #22840 ), #8727, .T. ) ;
#31987 = FACE_OUTER_BOUND ( 'NONE', #35541, .T. ) ;
#31988 = EDGE_CURVE ( 'NONE', #37754, #2697, #35240, .T. ) ;
#31989 = CARTESIAN_POINT ( 'NONE',  ( -15.48853125999098701, -26.74269726803709446, 0.000000000000000000 ) ) ;
#31990 = CIRCLE ( 'NONE', #27446, 6.000000000000013323 ) ;
#31991 = EDGE_CURVE ( 'NONE', #7799, #1139, #15956, .T. ) ;
#31992 = FACE_OUTER_BOUND ( 'NONE', #15887, .T. ) ;
#31993 = DIRECTION ( 'NONE',  ( 1.000000000000000000, 0.000000000000000000, 0.000000000000000000 ) ) ;
#31994 = DIRECTION ( 'NONE',  ( 0.000000000000000000, 0.000000000000000000, 1.000000000000000000 ) ) ;
#31995 = ORIENTED_EDGE ( 'NONE', *, *, #6439, .T. ) ;
#31996 = FACE_OUTER_BOUND ( 'NONE', #14909, .T. ) ;
#31997 =( GEOMETRIC_REPRESENTATION_CONTEXT ( 3 ) GLOBAL_UNCERTAINTY_ASSIGNED_CONTEXT ( ( #32340 ) ) GLOBAL_UNIT_ASSIGNED_CONTEXT ( ( #8111, #30260, #8720 ) ) REPRESENTATION_CONTEXT ( 'NONE', 'WORKASPACE' ) );
#31998 = CARTESIAN_POINT ( 'NONE',  ( 5.440829913680675034, 10.60893893836775348, 6.000000000000000000 ) ) ;
#31999 = CARTESIAN_POINT ( 'NONE',  ( 15.55596413789349342, -13.49028823909393893, -28.47924180414970863 ) ) ;
#32000 = DIRECTION ( 'NONE',  ( 0.000000000000000000, 0.000000000000000000, 1.000000000000000000 ) ) ;
#32001 = LINE ( 'NONE', #19206, #35909 ) ;
#32002 = CARTESIAN_POINT ( 'NONE',  ( 15.14367636855533483, 27.25780052973253476, -6.874303053600053559 ) ) ;
#32003 = CARTESIAN_POINT ( 'NONE',  ( -10.73859285986284640, 31.49625607628545154, 7.500000000000005329 ) ) ;
#32004 = VERTEX_POINT ( 'NONE', #24606 ) ;
#32005 = AXIS2_PLACEMENT_3D ( 'NONE', #5374, #36061, #4775 ) ;
#32006 = CARTESIAN_POINT ( 'NONE',  ( -17.83076603928403969, 19.73132804355285685, -4.999999999999999112 ) ) ;
#32007 = CARTESIAN_POINT ( 'NONE',  ( 36.74707368630883053, -16.71203845619566053, 10.99999999999983125 ) ) ;
#32008 = CARTESIAN_POINT ( 'NONE',  ( 14.02069553749537789, -24.60808805636505880, -12.55129267140057081 ) ) ;
#32009 = DIRECTION ( 'NONE',  ( 1.000000000000000000, 5.204170427930407084E-15, 0.000000000000000000 ) ) ;
#32010 = CARTESIAN_POINT ( 'NONE',  ( 14.03024999042850496, 23.93342408826297074, -13.51346792333798241 ) ) ;
#32011 = ORIENTED_EDGE ( 'NONE', *, *, #39347, .F. ) ;
#32012 = CARTESIAN_POINT ( 'NONE',  ( 10.99616811907620395, 17.35450030463652737, -28.70654324492396725 ) ) ;
#32013 = ORIENTED_EDGE ( 'NONE', *, *, #10369, .F. ) ;
#32015 = CARTESIAN_POINT ( 'NONE',  ( 3.503793317224320969, 8.420815634768672453, 11.00000000000000000 ) ) ;
#32014 = CARTESIAN_POINT ( 'NONE',  ( -12.60536492748955517, 21.12509647135009772, -18.44162819889032789 ) ) ;
#32016 = CARTESIAN_POINT ( 'NONE',  ( -14.34991748541630230, -25.06893485500494378, -11.59976961054102240 ) ) ;
#32017 = CIRCLE ( 'NONE', #2818, 1.000000000000000888 ) ;
#32018 = CARTESIAN_POINT ( 'NONE',  ( -35.86478881511108341, -18.48242683698273225, 12.73282698324857698 ) ) ;
#32019 = EDGE_CURVE ( 'NONE', #11801, #30503, #5912, .T. ) ;
#32020 = CARTESIAN_POINT ( 'NONE',  ( -19.17385361915705033, -12.37337734071081563, -22.99238475705470819 ) ) ;
#32021 = CIRCLE ( 'NONE', #30754, 0.4999999999999999445 ) ;
#32022 = CARTESIAN_POINT ( 'NONE',  ( -7.043788095933357418, -25.16102598387571376, -5.958356067281301627 ) ) ;
#32023 = CARTESIAN_POINT ( 'NONE',  ( 15.68203584040330334, 25.45105541600625187, -6.890715696209627872 ) ) ;
#32024 = VERTEX_POINT ( 'NONE', #37198 ) ;
#32025 = CARTESIAN_POINT ( 'NONE',  ( 23.69351461785554136, 8.239566554881321281, -8.880179489987360952 ) ) ;
#32026 = CARTESIAN_POINT ( 'NONE',  ( 27.27781358227127129, -25.27706179178272450, -4.999999999999999112 ) ) ;
#32027 = DIRECTION ( 'NONE',  ( 1.000000000000000000, 0.000000000000000000, 0.000000000000000000 ) ) ;
#32028 = CARTESIAN_POINT ( 'NONE',  ( -11.49018961600678779, 32.25363044047580985, 17.42190598798392287 ) ) ;
#32029 = ORIENTED_EDGE ( 'NONE', *, *, #32599, .T. ) ;
#32030 = CARTESIAN_POINT ( 'NONE',  ( -33.19333159104881048, -3.445792630615724050, -7.261352220591662743 ) ) ;
#32031 = CARTESIAN_POINT ( 'NONE',  ( -8.755436920523948174, 18.76929632780095858, 20.82122704794065982 ) ) ;
#32032 = ORIENTED_EDGE ( 'NONE', *, *, #30493, .T. ) ;
#32033 = CARTESIAN_POINT ( 'NONE',  ( 19.48557158514982746, -11.25000000000009415, 23.00000000000000000 ) ) ;
#32034 = CARTESIAN_POINT ( 'NONE',  ( -14.35088184066156280, 20.32132268570699196, 10.83333333333333393 ) ) ;
#32035 = CARTESIAN_POINT ( 'NONE',  ( 33.73785410275350216, -15.99653540799024931, -8.410072970351906818 ) ) ;
#32036 = CARTESIAN_POINT ( 'NONE',  ( 29.92393930195800067, -26.04303208588349250, 11.55979286843930964 ) ) ;
#32037 = CIRCLE ( 'NONE', #30747, 0.5000000000000001110 ) ;
#32038 = ADVANCED_FACE ( 'NONE', ( #36796 ), #36599, .F. ) ;
#32039 = ORIENTED_EDGE ( 'NONE', *, *, #16721, .T. ) ;
#32040 = VERTEX_POINT ( 'NONE', #39639 ) ;
#32041 = DIRECTION ( 'NONE',  ( -0.8660254037844454800, -0.4999999999999881206, 0.000000000000000000 ) ) ;
#32042 = CARTESIAN_POINT ( 'NONE',  ( -24.10033869720827227, 8.113510326755614344, -5.000000000000002665 ) ) ;
#32043 = CARTESIAN_POINT ( 'NONE',  ( 19.48557158514988075, -11.24999999999998224, 0.000000000000000000 ) ) ;
#32044 = ORIENTED_EDGE ( 'NONE', *, *, #25566, .F. ) ;
#32045 = AXIS2_PLACEMENT_3D ( 'NONE', #27061, #36405, #14872 ) ;
#32046 = CARTESIAN_POINT ( 'NONE',  ( -0.3989805618741724125, 20.59240739012455990, -28.44384999149225379 ) ) ;
#32047 = CARTESIAN_POINT ( 'NONE',  ( 0.9999966292907466192, 22.50000000000031264, 13.00000000000000178 ) ) ;
#32048 = DIRECTION ( 'NONE',  ( 1.000000000000000000, 0.000000000000000000, 0.000000000000000000 ) ) ;
#32049 = CARTESIAN_POINT ( 'NONE',  ( 17.00000000000000000, 22.50000000000000711, 10.00000000000000000 ) ) ;
#32050 = CARTESIAN_POINT ( 'NONE',  ( 5.537946624086096392, 36.44027069998188750, 7.500000000000000888 ) ) ;
#32051 = CARTESIAN_POINT ( 'NONE',  ( -22.32447841415231338, 25.34915137120643180, 11.00000000000000000 ) ) ;
#32052 = CARTESIAN_POINT ( 'NONE',  ( 9.263407132367138530, 18.28842304576874156, -29.31195371305176067 ) ) ;
#32053 = CARTESIAN_POINT ( 'NONE',  ( -8.118377661053488126, 10.47536095541708967, 7.000000000000000000 ) ) ;
#32054 = ORIENTED_EDGE ( 'NONE', *, *, #38076, .F. ) ;
#32056 = DIRECTION ( 'NONE',  ( 0.000000000000000000, 0.000000000000000000, 1.000000000000000000 ) ) ;
#32055 = CARTESIAN_POINT ( 'NONE',  ( -19.69150485828470920, 15.64879689043717192, -4.999999999999998224 ) ) ;
#32057 = DIRECTION ( 'NONE',  ( -1.000000000000000000, 0.000000000000000000, 0.000000000000000000 ) ) ;
#32058 = CARTESIAN_POINT ( 'NONE',  ( -3.833852081710640292, 25.75497152300896175, 23.00000000000000000 ) ) ;
#32059 = CARTESIAN_POINT ( 'NONE',  ( 15.45120705166009678, -26.60939779128311500, -6.886503721798920452 ) ) ;
#32060 = DIRECTION ( 'NONE',  ( 1.000000000000000000, 0.000000000000000000, 0.000000000000000000 ) ) ;
#32061 = CARTESIAN_POINT ( 'NONE',  ( 11.28132746819896504, 18.06042462519475933, -25.01062990606723346 ) ) ;
#32062 = CARTESIAN_POINT ( 'NONE',  ( -22.45323650136969462, -2.382502413133420038, -20.55760979252980647 ) ) ;
#32063 = DIRECTION ( 'NONE',  ( 0.000000000000000000, 0.000000000000000000, 1.000000000000000000 ) ) ;
#32064 = VECTOR ( 'NONE', #18019, 1000.000000000000000 ) ;
#32065 = CARTESIAN_POINT ( 'NONE',  ( -14.31376830907703557, -15.17370222568340488, -27.11184809475398438 ) ) ;
#32066 = CARTESIAN_POINT ( 'NONE',  ( 5.958427663799773732, -24.34613153426185761, -10.83339736943976028 ) ) ;
#32067 = CARTESIAN_POINT ( 'NONE',  ( 13.29387873628312633, 22.08577950255929778, -16.45709539392367660 ) ) ;
#32068 = CARTESIAN_POINT ( 'NONE',  ( 20.55850455995617310, 13.96709772207984557, -5.966656640325017413 ) ) ;
#32069 = EDGE_CURVE ( 'NONE', #4829, #33109, #26903, .T. ) ;
#32070 = DIRECTION ( 'NONE',  ( 0.000000000000000000, 0.000000000000000000, 1.000000000000000000 ) ) ;
#32071 = FACE_OUTER_BOUND ( 'NONE', #31920, .T. ) ;
#32072 = ORIENTED_EDGE ( 'NONE', *, *, #2203, .F. ) ;
#32073 = CARTESIAN_POINT ( 'NONE',  ( -9.173595147271331740, 34.50490541566588121, -8.476194683046836431 ) ) ;
#32074 = VERTEX_POINT ( 'NONE', #9168 ) ;
#32075 = AXIS2_PLACEMENT_3D ( 'NONE', #39352, #33476, #23912 ) ;
#32076 = CARTESIAN_POINT ( 'NONE',  ( -9.183247089818959097, 16.78440424842446532, 13.00000000000000178 ) ) ;
#32077 = EDGE_LOOP ( 'NONE', ( #39102, #15115, #9651, #24990, #408 ) ) ;
#32078 = CARTESIAN_POINT ( 'NONE',  ( 30.38638613626090645, -0.03985804923669677979, -8.295769245405898218 ) ) ;
#32079 = FACE_OUTER_BOUND ( 'NONE', #6658, .T. ) ;
#32080 = CARTESIAN_POINT ( 'NONE',  ( -25.98021325959403427, -4.875178728618521973, 20.50957957746029692 ) ) ;
#32081 = EDGE_CURVE ( 'NONE', #25787, #8554, #9392, .T. ) ;
#32082 = B_SPLINE_SURFACE_WITH_KNOTS ( 'NONE', 1, 3, ( 
 ( #22343, #21952, #37601, #25391, #9371, #6899, #31104, #3468, #12409, #25002 ),
 ( #15260, #12212, #15661, #9767, #24801, #2872, #15460, #6502, #34548, #37394 ) ),
 .UNSPECIFIED., .F., .F., .F.,
 ( 2, 2 ),
 ( 4, 2, 2, 2, 4 ),
 ( 0.000000000000000000, 1.000000000000000000 ),
 ( -1.421612811542168231, -1.028913729843446090, -0.6362146481447240598, -0.2435155664460019742, 0.1491835152527200836 ),
 .UNSPECIFIED. ) ;
#32083 = EDGE_LOOP ( 'NONE', ( #32390, #7950, #27409 ) ) ;
#32084 = CARTESIAN_POINT ( 'NONE',  ( -20.60809083734462277, 0.8890292739548594225, -28.07942971103104313 ) ) ;
#32085 = CARTESIAN_POINT ( 'NONE',  ( -20.54949622337250403, -27.17849093743868849, -5.904791858790468417 ) ) ;
#32086 = ORIENTED_EDGE ( 'NONE', *, *, #9158, .F. ) ;
#32087 = CARTESIAN_POINT ( 'NONE',  ( 25.26093265137713573, -6.803277765801289512, -18.80458527437446747 ) ) ;
#32088 = CIRCLE ( 'NONE', #21072, 1.000000000000000000 ) ;
#32089 = VERTEX_POINT ( 'NONE', #24201 ) ;
#32090 = DIRECTION ( 'NONE',  ( 0.000000000000000000, 0.000000000000000000, 1.000000000000000000 ) ) ;
#32091 = FACE_OUTER_BOUND ( 'NONE', #4857, .T. ) ;
#32092 = CARTESIAN_POINT ( 'NONE',  ( 4.817371740575539185, 23.83900317890011422, 20.99999999999999645 ) ) ;
#32093 = VECTOR ( 'NONE', #18822, 1000.000000000000000 ) ;
#32094 = CARTESIAN_POINT ( 'NONE',  ( 4.524139159579307012, 31.43208625488810171, 10.00000000000000000 ) ) ;
#32095 = CARTESIAN_POINT ( 'NONE',  ( -8.842993596485667851, 30.00678625355870111, 19.66345542862525519 ) ) ;
#32096 = AXIS2_PLACEMENT_3D ( 'NONE', #24, #11815, #5510 ) ;
#32097 = CARTESIAN_POINT ( 'NONE',  ( 3.863783140547853712E-14, -86.77689918168233874, 3.000000000000000000 ) ) ;
#32098 = ORIENTED_EDGE ( 'NONE', *, *, #9085, .T. ) ;
#32099 = CARTESIAN_POINT ( 'NONE',  ( -15.31690239355500971, 13.64047066522845242, -30.00000000000001776 ) ) ;
#32100 = DIRECTION ( 'NONE',  ( -0.000000000000000000, -0.000000000000000000, 1.000000000000000000 ) ) ;
#32101 = EDGE_CURVE ( 'NONE', #23066, #37754, #6730, .T. ) ;
#32102 = LINE ( 'NONE', #38395, #24697 ) ;
#32103 = CARTESIAN_POINT ( 'NONE',  ( 15.80069108502425301, 17.14170230956324303, -17.82616030926931927 ) ) ;
#32104 = CARTESIAN_POINT ( 'NONE',  ( 5.706445963761893836, 19.68930810918331531, -29.25141939363317078 ) ) ;
#32105 = ORIENTED_EDGE ( 'NONE', *, *, #35133, .T. ) ;
#32106 = DIRECTION ( 'NONE',  ( 0.000000000000000000, 0.000000000000000000, 1.000000000000000000 ) ) ;
#32107 = LINE ( 'NONE', #4067, #7786 ) ;
#32108 = CARTESIAN_POINT ( 'NONE',  ( 9.965926242692308534, -17.97018614680934689, -28.68921181318054892 ) ) ;
#32109 = CARTESIAN_POINT ( 'NONE',  ( 15.27443809245942141, -27.57253143578274290, 15.13084544680213561 ) ) ;
#32110 = LINE ( 'NONE', #19721, #32190 ) ;
#32111 = B_SPLINE_CURVE_WITH_KNOTS ( 'NONE', 3,
 ( #17876, #21111, #39788, #8109, #5659, #20911 ),
 .UNSPECIFIED., .F., .F.,
 ( 4, 2, 4 ),
 ( 0.000000000000000000, 0.4333333202469910606, 0.8666666404939821211 ),
 .UNSPECIFIED. ) ;
#32112 = AXIS2_PLACEMENT_3D ( 'NONE', #15377, #18633, #40156 ) ;
#32113 = EDGE_LOOP ( 'NONE', ( #11246, #12825 ) ) ;
#32114 = CARTESIAN_POINT ( 'NONE',  ( -14.94540916678409559, 25.76695089328861599, -9.709480485754761858 ) ) ;
#32115 = CARTESIAN_POINT ( 'NONE',  ( -33.53427059938940857, -2.462512058961074946, 15.72805884748892957 ) ) ;
#32116 = CARTESIAN_POINT ( 'NONE',  ( 9.271440805881887570, -18.28379014461920349, -30.00000000000000000 ) ) ;
#32117 = EDGE_CURVE ( 'NONE', #3600, #9898, #40033, .T. ) ;
#32118 = CARTESIAN_POINT ( 'NONE',  ( -1.494943660522439099, 10.76222879119470832, 12.00000000000000000 ) ) ;
#32119 = ORIENTED_EDGE ( 'NONE', *, *, #21941, .T. ) ;
#32120 = ORIENTED_EDGE ( 'NONE', *, *, #20795, .T. ) ;
#32121 = CARTESIAN_POINT ( 'NONE',  ( -10.24063254661171918, 21.86334665591954618, -20.21485189711300379 ) ) ;
#32122 = AXIS2_PLACEMENT_3D ( 'NONE', #4169, #11284, #1330 ) ;
#32123 = DIRECTION ( 'NONE',  ( -0.000000000000000000, -0.000000000000000000, -1.000000000000000000 ) ) ;
#32124 = CARTESIAN_POINT ( 'NONE',  ( -12.38757880222266650, 14.77067777473956767, 10.99387789255785464 ) ) ;
#32125 = AXIS2_PLACEMENT_3D ( 'NONE', #15613, #3616, #6458 ) ;
#32127 = VECTOR ( 'NONE', #11695, 1000.000000000000000 ) ;
#32126 = CARTESIAN_POINT ( 'NONE',  ( -31.82304104356865793, -7.834543439184518121, -12.09424007204980711 ) ) ;
#32128 = CARTESIAN_POINT ( 'NONE',  ( 13.64210930126480115, 24.20081211342298744, 12.00000000000000000 ) ) ;
#32129 = ORIENTED_EDGE ( 'NONE', *, *, #31739, .T. ) ;
#32130 = CARTESIAN_POINT ( 'NONE',  ( 30.52903303563438797, 0.07247293852937149172, -7.358272049610939725 ) ) ;
#32131 = EDGE_CURVE ( 'NONE', #7162, #11320, #2788, .T. ) ;
#32132 = CARTESIAN_POINT ( 'NONE',  ( 11.05997879105324877, 17.47350834465349578, -27.43542404371585164 ) ) ;
#32133 = CYLINDRICAL_SURFACE ( 'NONE', #40085, 1.000000000000000000 ) ;
#32134 = ADVANCED_FACE ( 'NONE', ( #11622 ), #14589, .T. ) ;
#32135 = ORIENTED_EDGE ( 'NONE', *, *, #30958, .T. ) ;
#32136 = CARTESIAN_POINT ( 'NONE',  ( -28.34239771388248030, 0.1355473793836993457, -12.55008231272072194 ) ) ;
#32137 = CARTESIAN_POINT ( 'NONE',  ( -38.11240863262091949, -18.68972660803411046, 11.00000000000000355 ) ) ;
#32138 = ORIENTED_EDGE ( 'NONE', *, *, #21753, .T. ) ;
#32139 = CARTESIAN_POINT ( 'NONE',  ( 28.83559650784853545, -2.623511950590506014, -14.20132271218602149 ) ) ;
#32140 = LINE ( 'NONE', #22987, #16145 ) ;
#32141 = CARTESIAN_POINT ( 'NONE',  ( 17.23228185427324277, -26.71557896777858332, 16.87380292611382515 ) ) ;
#32142 = ORIENTED_EDGE ( 'NONE', *, *, #21458, .F. ) ;
#32143 = CARTESIAN_POINT ( 'NONE',  ( 14.21868324749889645, 30.05186662605645864, 16.30093088680188274 ) ) ;
#32144 = CARTESIAN_POINT ( 'NONE',  ( -5.468510220371378239, -21.80712738496724157, 18.87996532025784902 ) ) ;
#32145 = FACE_OUTER_BOUND ( 'NONE', #35434, .T. ) ;
#32146 = CIRCLE ( 'NONE', #28892, 0.5000000000000001110 ) ;
#32147 = CARTESIAN_POINT ( 'NONE',  ( 1.082972213713589094, 27.41125570341916173, 21.00000000000000355 ) ) ;
#32148 = FACE_OUTER_BOUND ( 'NONE', #26992, .T. ) ;
#32149 = EDGE_CURVE ( 'NONE', #6084, #2291, #15222, .T. ) ;
#32150 = PLANE ( 'NONE',  #13044 ) ;
#32151 = EDGE_CURVE ( 'NONE', #38676, #39628, #317, .T. ) ;
#32152 = CIRCLE ( 'NONE', #9453, 1.000000000000000000 ) ;
#32153 = AXIS2_PLACEMENT_3D ( 'NONE', #21455, #15164, #18418 ) ;
#32154 = TOROIDAL_SURFACE ( 'NONE', #33461, 1.000000000000000000, 0.5000000000000000000 ) ;
#32155 = FACE_BOUND ( 'NONE', #26984, .T. ) ;
#32156 = CARTESIAN_POINT ( 'NONE',  ( 19.62624412895855741, 17.27415994119410669, 15.13084544680202548 ) ) ;
#32157 = CARTESIAN_POINT ( 'NONE',  ( -23.57137302209975260, 8.956611734839530214, -5.963979942565353909 ) ) ;
#32158 = CARTESIAN_POINT ( 'NONE',  ( 20.69337408919974663, -25.59025939823920481, -10.36400023151281324 ) ) ;
#32159 = CARTESIAN_POINT ( 'NONE',  ( -24.54956740501959800, -26.55910502559106590, -5.000000000000000000 ) ) ;
#32160 = ORIENTED_EDGE ( 'NONE', *, *, #32743, .F. ) ;
#32161 = CARTESIAN_POINT ( 'NONE',  ( 12.31018467675442096, 20.59829060042622828, -19.47928546867396093 ) ) ;
#32162 = ORIENTED_EDGE ( 'NONE', *, *, #28988, .T. ) ;
#32163 = CARTESIAN_POINT ( 'NONE',  ( -15.63234325287015558, 24.80996185906289853, -8.309407532411428932 ) ) ;
#32164 = CARTESIAN_POINT ( 'NONE',  ( -30.76885290917900662, -8.559665202950077045, 19.66345542862464768 ) ) ;
#32165 = DIRECTION ( 'NONE',  ( 0.000000000000000000, 0.000000000000000000, 1.000000000000000000 ) ) ;
#32166 = CARTESIAN_POINT ( 'NONE',  ( 15.39960304625618726, 26.57504432316893883, -6.417109345100691975 ) ) ;
#32167 = ORIENTED_EDGE ( 'NONE', *, *, #19192, .F. ) ;
#32168 = CARTESIAN_POINT ( 'NONE',  ( 32.80197066822268681, -18.08580508125842101, -8.405041325730369550 ) ) ;
#32169 = CYLINDRICAL_SURFACE ( 'NONE', #31975, 1.000000000000000888 ) ;
#32170 = ORIENTED_EDGE ( 'NONE', *, *, #9617, .F. ) ;
#32172 = PLANE ( 'NONE',  #10174 ) ;
#32171 = CARTESIAN_POINT ( 'NONE',  ( -10.85232944982509373, 17.54704845259137969, -28.06621872721026278 ) ) ;
#32173 = CARTESIAN_POINT ( 'NONE',  ( -14.44323513478368426, -23.70972000048200812, -14.37742332914230659 ) ) ;
#32174 = ADVANCED_FACE ( 'NONE', ( #2480 ), #18315, .T. ) ;
#32175 = DIRECTION ( 'NONE',  ( 1.000000000000000000, 0.000000000000000000, -0.000000000000000000 ) ) ;
#32176 = VERTEX_POINT ( 'NONE', #15059 ) ;
#32177 = CARTESIAN_POINT ( 'NONE',  ( -21.63092173904548332, -9.727850427649963549, -21.86719485504245952 ) ) ;
#32178 = CARTESIAN_POINT ( 'NONE',  ( -9.124714416476436440, -18.84963008713028287, -26.28455564130669941 ) ) ;
#32179 = CARTESIAN_POINT ( 'NONE',  ( 12.05736835487432579, 14.38397459621550567, 10.49999999999999822 ) ) ;
#32180 = CARTESIAN_POINT ( 'NONE',  ( 13.28607726706187364, 15.81902776886276385, -27.59724186177722416 ) ) ;
#32181 = ORIENTED_EDGE ( 'NONE', *, *, #38260, .T. ) ;
#32182 = CARTESIAN_POINT ( 'NONE',  ( 27.65851975983521527, 2.896154268494189665, -8.808624792320287611 ) ) ;
#32183 = CARTESIAN_POINT ( 'NONE',  ( -11.74460609746112461, 31.83082137946488643, 7.365559175140416137 ) ) ;
#32184 = CARTESIAN_POINT ( 'NONE',  ( -20.92112759555551094, -16.07000418475121961, 23.00000000000000000 ) ) ;
#32185 = VECTOR ( 'NONE', #32165, 1000.000000000000000 ) ;
#32186 = EDGE_LOOP ( 'NONE', ( #12237, #10184 ) ) ;
#32187 = CARTESIAN_POINT ( 'NONE',  ( -30.81597363132232914, -0.1242289339610933435, -6.885118092463035744 ) ) ;
#32188 = CARTESIAN_POINT ( 'NONE',  ( 20.49250884496040115, 0.5553618484168656444, -29.34280755129132245 ) ) ;
#32189 = CONICAL_SURFACE ( 'NONE', #31513, 1.000000000000004441, 0.7853981633974591592 ) ;
#32190 = VECTOR ( 'NONE', #4275, 1000.000000000000000 ) ;
#32191 = CARTESIAN_POINT ( 'NONE',  ( 26.04200899061357077, -18.69117426458517528, 20.25080042701566541 ) ) ;
#32192 = VECTOR ( 'NONE', #2784, 1000.000000000000114 ) ;
#32193 = ORIENTED_EDGE ( 'NONE', *, *, #18111, .F. ) ;
#32194 = CARTESIAN_POINT ( 'NONE',  ( 6.023418944065110914, 39.81932404830325112, -14.45070082761206365 ) ) ;
#32195 = CARTESIAN_POINT ( 'NONE',  ( -14.09933648065464062, 26.02968990214173317, 10.50000000000000533 ) ) ;
#32196 = DIRECTION ( 'NONE',  ( 0.4999999999999919509, -0.8660254037844432595, 0.000000000000000000 ) ) ;
#32197 = DIRECTION ( 'NONE',  ( -0.5877852522924690293, 0.8090169943749503378, -0.000000000000000000 ) ) ;
#32198 = EDGE_CURVE ( 'NONE', #8093, #3398, #38562, .T. ) ;
#32199 = CARTESIAN_POINT ( 'NONE',  ( -11.11016527260153630, 31.83082137946488643, 11.00000000000000000 ) ) ;
#32200 = CARTESIAN_POINT ( 'NONE',  ( 22.71238962388145310, 10.21442836349894456, -4.999999999999998224 ) ) ;
#32201 = DIRECTION ( 'NONE',  ( 1.000000000000000000, 0.000000000000000000, 0.000000000000000000 ) ) ;
#32202 = EDGE_LOOP ( 'NONE', ( #18574, #35166, #15552, #18771 ) ) ;
#32203 = CYLINDRICAL_SURFACE ( 'NONE', #31332, 1.000000000000000000 ) ;
#32204 = DIRECTION ( 'NONE',  ( -0.6691306063588671194, -0.7431448254773862505, 0.000000000000000000 ) ) ;
#32205 = CARTESIAN_POINT ( 'NONE',  ( 26.77741691842820870, -24.73292702398819642, -8.017675451830744038 ) ) ;
#32206 = DIRECTION ( 'NONE',  ( 0.7032331762534084207, 0.07391278520354237214, -0.7071067811865459074 ) ) ;
#32207 = DIRECTION ( 'NONE',  ( 0.000000000000000000, -0.000000000000000000, -1.000000000000000000 ) ) ;
#32208 = CARTESIAN_POINT ( 'NONE',  ( 15.05466390046562886, 27.28512766916796295, -7.337438985496051558 ) ) ;
#32209 = ORIENTED_EDGE ( 'NONE', *, *, #26253, .T. ) ;
#32211 = VECTOR ( 'NONE', #8641, 1000.000000000000000 ) ;
#32210 = CARTESIAN_POINT ( 'NONE',  ( -14.00996106472373270, 15.24814236169682147, -27.05129743250489938 ) ) ;
#32212 = CARTESIAN_POINT ( 'NONE',  ( 14.42035624161478857, 26.65972665747660031, 10.50000000000000000 ) ) ;
#32213 = VECTOR ( 'NONE', #16741, 1000.000000000000000 ) ;
#32214 = CARTESIAN_POINT ( 'NONE',  ( 14.68419454952205072, -25.64123961583407763, -10.18168563382398162 ) ) ;
#32215 = DIRECTION ( 'NONE',  ( 0.000000000000000000, 0.000000000000000000, 1.000000000000000000 ) ) ;
#32216 = CARTESIAN_POINT ( 'NONE',  ( 15.37856327759776320, 26.64927617434213047, -6.417027871434891395 ) ) ;
#32217 = VERTEX_POINT ( 'NONE', #19301 ) ;
#32218 = CARTESIAN_POINT ( 'NONE',  ( 13.76661467574962394, 23.40248112065825836, -14.47560752045292709 ) ) ;
#32219 = ORIENTED_EDGE ( 'NONE', *, *, #35193, .F. ) ;
#32221 = DIRECTION ( 'NONE',  ( 0.000000000000000000, 0.000000000000000000, 1.000000000000000000 ) ) ;
#32220 = CARTESIAN_POINT ( 'NONE',  ( -14.99409613481703651, 26.04743989974285867, -9.234380414057861586 ) ) ;
#32222 = CARTESIAN_POINT ( 'NONE',  ( -15.37461277948404614, -26.63904247529195146, -6.417043597033281088 ) ) ;
#32223 = EDGE_CURVE ( 'NONE', #8314, #22563, #12635, .T. ) ;
#32224 = CARTESIAN_POINT ( 'NONE',  ( -22.73078996736922264, -29.06185046644117165, 11.55979286843901122 ) ) ;
#32225 = CARTESIAN_POINT ( 'NONE',  ( -21.60462512834099869, -13.94959705066216493, -19.63613014917582689 ) ) ;
#32226 = CARTESIAN_POINT ( 'NONE',  ( -4.583136480692052039, -24.23512553185321750, -10.85810497518859030 ) ) ;
#32227 = CARTESIAN_POINT ( 'NONE',  ( 13.66344759430295674, 21.43633434956417716, -16.51270124952114671 ) ) ;
#32229 = EDGE_CURVE ( 'NONE', #39481, #24143, #37994, .T. ) ;
#32228 = EDGE_LOOP ( 'NONE', ( #4401, #8384, #25852, #9728 ) ) ;
#32230 = CARTESIAN_POINT ( 'NONE',  ( 24.02933105728603991, 8.309275822838595005, -5.480673643475639345 ) ) ;
#32231 = CARTESIAN_POINT ( 'NONE',  ( -8.437494178870162287, 40.76200630940459746, 11.00000000000000178 ) ) ;
#32232 = CARTESIAN_POINT ( 'NONE',  ( -9.697889840765283154, 31.90483559858340357, 10.00000000000000000 ) ) ;
#32233 = CARTESIAN_POINT ( 'NONE',  ( -12.40052356344504680, 30.91160080447363256, 17.42190598798392642 ) ) ;
#32234 = VERTEX_POINT ( 'NONE', #22543 ) ;
#32235 = CARTESIAN_POINT ( 'NONE',  ( -28.11566308881036846, -1.264383335452437418, -14.31890013009667939 ) ) ;
#32236 =( BOUNDED_SURFACE ( )  B_SPLINE_SURFACE ( 2, 3, ( 
 ( #2387, #36509, #33278, #39944, #6018, #5827 ),
 ( #14777, #30012, #17837, #27164, #21462, #8877 ),
 ( #2188, #36713, #2979, #11529, #18423, #23914 ) ),
 .UNSPECIFIED., .F., .F., .T. ) 
 B_SPLINE_SURFACE_WITH_KNOTS ( ( 3, 3 ),
 ( 4, 2, 4 ),
 ( 0.000000000000000000, 1.000000000000000000 ),
 ( 1.318307113131750086, 1.570796326794896336, 1.823285540458042586 ),
 .UNSPECIFIED. ) 
 GEOMETRIC_REPRESENTATION_ITEM ( )  RATIONAL_B_SPLINE_SURFACE ( (
 ( 1.000000000000000000, 1.000000000000000000, 1.000000000000000000, 1.000000000000000000, 1.000000000000000000, 1.000000000000000000),
 ( 0.7071067811865474617, 0.7071067811865474617, 0.7071067811865474617, 0.7071067811865474617, 0.7071067811865474617, 0.7071067811865474617),
 ( 1.000000000000000000, 1.000000000000000000, 1.000000000000000000, 1.000000000000000000, 1.000000000000000000, 1.000000000000000000) ) ) 
 REPRESENTATION_ITEM ( '' )  SURFACE ( )  );
#32237 = EDGE_CURVE ( 'NONE', #23669, #1290, #23146, .T. ) ;
#32238 = CARTESIAN_POINT ( 'NONE',  ( -19.50480011250488843, 16.42246729932494276, 10.00000000000000000 ) ) ;
#32239 = VERTEX_POINT ( 'NONE', #10566 ) ;
#32240 = CARTESIAN_POINT ( 'NONE',  ( -13.13581098909220302, 27.45627467658446008, 7.499999999999993783 ) ) ;
#32241 = CARTESIAN_POINT ( 'NONE',  ( -10.03245514394471627, 31.53326318584470656, 7.000000000000000000 ) ) ;
#32242 = CARTESIAN_POINT ( 'NONE',  ( -12.99377146717200660, 26.19620116591435277, 7.000000000000000000 ) ) ;
#32243 = CARTESIAN_POINT ( 'NONE',  ( 24.46249166291341126, -10.72823817068293728, -18.64685341546218211 ) ) ;
#32244 = CARTESIAN_POINT ( 'NONE',  ( 37.13148535761801838, -14.80270701502657538, 11.55979286843934872 ) ) ;
#32245 = AXIS2_PLACEMENT_3D ( 'NONE', #5888, #34131, #4 ) ;
#32246 = CIRCLE ( 'NONE', #14730, 1.000000000000004441 ) ;
#32247 = ORIENTED_EDGE ( 'NONE', *, *, #21207, .F. ) ;
#32248 = LINE ( 'NONE', #4412, #11950 ) ;
#32249 = CARTESIAN_POINT ( 'NONE',  ( -16.10728771989144903, 24.44770348874625299, -4.999999999999999112 ) ) ;
#32250 = EDGE_CURVE ( 'NONE', #36138, #5201, #10974, .T. ) ;
#32251 = EDGE_CURVE ( 'NONE', #30326, #12836, #33422, .T. ) ;
#32252 = LINE ( 'NONE', #25940, #22689 ) ;
#32253 = ORIENTED_EDGE ( 'NONE', *, *, #33979, .T. ) ;
#32254 = CARTESIAN_POINT ( 'NONE',  ( -1.915298613502000036, 38.17830312701165241, -6.697546018672553281 ) ) ;
#32255 = PLANE ( 'NONE',  #21086 ) ;
#32256 = DIRECTION ( 'NONE',  ( -0.5254827454987532898, 0.4731467892558212651, -0.7071067811865475727 ) ) ;
#32257 = CARTESIAN_POINT ( 'NONE',  ( -8.505700342264141511, 22.10876900990917804, 9.000000000000001776 ) ) ;
#32258 = DIRECTION ( 'NONE',  ( -0.1045284632676570929, -0.9945218953682729568, 0.000000000000000000 ) ) ;
#32259 = CARTESIAN_POINT ( 'NONE',  ( 4.724371395536106633, 32.23037938972932892, 12.00000000000000000 ) ) ;
#32260 = CARTESIAN_POINT ( 'NONE',  ( 11.22822495210109395, 22.89591416269367841, -18.18872776029335014 ) ) ;
#32261 = DIRECTION ( 'NONE',  ( -1.000000000000000000, 0.000000000000000000, 0.000000000000000000 ) ) ;
#32262 = EDGE_LOOP ( 'NONE', ( #15881, #18305, #3924 ) ) ;
#32264 = DIRECTION ( 'NONE',  ( 0.5877852522924690293, -0.8090169943749503378, 0.000000000000000000 ) ) ;
#32263 = CARTESIAN_POINT ( 'NONE',  ( -17.49499888782854384, 11.31808902454676335, -25.50841800900462886 ) ) ;
#32265 = CARTESIAN_POINT ( 'NONE',  ( -14.11133924723977451, 27.61078317377193869, 10.49999999999999112 ) ) ;
#32266 = CARTESIAN_POINT ( 'NONE',  ( 15.24043722059125017, -26.29847216020535683, -8.295283855862736644 ) ) ;
#32267 = FACE_OUTER_BOUND ( 'NONE', #27990, .T. ) ;
#32268 = CARTESIAN_POINT ( 'NONE',  ( 12.62672847796949505, 21.09324721752569332, -18.44634832236629407 ) ) ;
#32269 = CARTESIAN_POINT ( 'NONE',  ( -23.06249103411543544, 13.31513540672989926, -4.999999999999996447 ) ) ;
#32270 = DIRECTION ( 'NONE',  ( 1.000000000000000000, 0.000000000000000000, 0.000000000000000000 ) ) ;
#32271 = EDGE_CURVE ( 'NONE', #19280, #30187, #28844, .T. ) ;
#32272 = AXIS2_PLACEMENT_3D ( 'NONE', #24833, #9198, #9798 ) ;
#32273 = VECTOR ( 'NONE', #4600, 1000.000000000000114 ) ;
#32274 = CARTESIAN_POINT ( 'NONE',  ( -27.94687998398240225, -24.71358538153085149, -6.293495900045230407 ) ) ;
#32275 = CARTESIAN_POINT ( 'NONE',  ( 5.399542109131928669, -22.95868181222395066, -15.85264200238205312 ) ) ;
#32276 = CARTESIAN_POINT ( 'NONE',  ( 11.09252425524408459, 17.23965631597926418, -29.35067692373401016 ) ) ;
#32277 = EDGE_CURVE ( 'NONE', #18096, #13411, #23361, .T. ) ;
#32278 = CARTESIAN_POINT ( 'NONE',  ( 16.75470528484330046, 11.98919836256815330, -27.72802603258947229 ) ) ;
#32279 = DIRECTION ( 'NONE',  ( 1.000000000000000000, 0.000000000000000000, 0.000000000000000000 ) ) ;
#32280 = CARTESIAN_POINT ( 'NONE',  ( 11.77090408390491305, 15.39748370681878775, 6.000000000000000000 ) ) ;
#32281 = VERTEX_POINT ( 'NONE', #39196 ) ;
#32282 = CARTESIAN_POINT ( 'NONE',  ( -8.724803901531640093, 32.67470959390297480, -11.16207224700029776 ) ) ;
#32283 = AXIS2_PLACEMENT_3D ( 'NONE', #30801, #2762, #6399 ) ;
#32284 = EDGE_LOOP ( 'NONE', ( #1909, #28308, #11210 ) ) ;
#32285 = CARTESIAN_POINT ( 'NONE',  ( -15.32303194119059420, -26.70022385808693954, -5.474162114618875030 ) ) ;
#32286 = CIRCLE ( 'NONE', #25108, 1.000000000000000888 ) ;
#32287 = DIRECTION ( 'NONE',  ( -0.9781476007338069101, -0.2079116908177533751, 0.000000000000000000 ) ) ;
#32288 = EDGE_LOOP ( 'NONE', ( #35035, #3285 ) ) ;
#32289 = CARTESIAN_POINT ( 'NONE',  ( 23.32290838231767438, 0.5357531857212454174, -20.54009308810276124 ) ) ;
#32290 = PLANE ( 'NONE',  #5077 ) ;
#32291 = DIRECTION ( 'NONE',  ( 0.000000000000000000, 0.000000000000000000, -1.000000000000000000 ) ) ;
#32292 = EDGE_LOOP ( 'NONE', ( #14886, #30034, #7123, #10054, #26320, #7929, #19435, #17672 ) ) ;
#32293 = CARTESIAN_POINT ( 'NONE',  ( -30.74131631141073129, 0.1242922002067066989, -4.999999999999999112 ) ) ;
#32294 = ORIENTED_EDGE ( 'NONE', *, *, #12942, .F. ) ;
#32295 = CARTESIAN_POINT ( 'NONE',  ( 35.21367278186023952, -9.523108846389430227, -6.737064075858604006 ) ) ;
#32296 = VERTEX_POINT ( 'NONE', #26399 ) ;
#32297 = CARTESIAN_POINT ( 'NONE',  ( 0.000000000000000000, 0.000000000000000000, 0.000000000000000000 ) ) ;
#32298 = CARTESIAN_POINT ( 'NONE',  ( -1.477035006930975258E-13, 40.50000000000004974, 11.00000000000000000 ) ) ;
#32299 = DIRECTION ( 'NONE',  ( 0.000000000000000000, 0.000000000000000000, 1.000000000000000000 ) ) ;
#32300 = DIRECTION ( 'NONE',  ( 0.2876062384759424106, -0.6459741880212539478, -0.7071067811865482389 ) ) ;
#32301 = CARTESIAN_POINT ( 'NONE',  ( -7.124477683922587623, 34.33078274760865867, 18.42518152272030463 ) ) ;
#32302 = VECTOR ( 'NONE', #8952, 1000.000000000000000 ) ;
#32303 = AXIS2_PLACEMENT_3D ( 'NONE', #25082, #304, #15940 ) ;
#32304 = CARTESIAN_POINT ( 'NONE',  ( 13.94482798346721353, 26.50521816028912525, 9.000000000000001776 ) ) ;
#32305 = ORIENTED_EDGE ( 'NONE', *, *, #36311, .T. ) ;
#32306 = FILL_AREA_STYLE_COLOUR ( '', #20997 ) ;
#32307 = CARTESIAN_POINT ( 'NONE',  ( 9.331903152615748098, 11.35703883385568780, 7.500000000000000888 ) ) ;
#32308 = CARTESIAN_POINT ( 'NONE',  ( 3.835130509701798918, 15.55077355964573904, 13.00000000000000178 ) ) ;
#32309 = EDGE_CURVE ( 'NONE', #36348, #12651, #32914, .T. ) ;
#32310 = CONICAL_SURFACE ( 'NONE', #37493, 1.000000000000014655, 0.7853981633974526089 ) ;
#32311 = CARTESIAN_POINT ( 'NONE',  ( 10.44103466624280507, 32.57396620494213124, 7.000000000000000000 ) ) ;
#32312 = CARTESIAN_POINT ( 'NONE',  ( 17.18224089502211882, 16.15582687960090524, -15.85542385682627753 ) ) ;
#32313 = CIRCLE ( 'NONE', #20631, 6.000000000000000888 ) ;
#32314 = CARTESIAN_POINT ( 'NONE',  ( 11.71220820147315500, 33.45731985618542836, -5.448922514974672282 ) ) ;
#32315 = ORIENTED_EDGE ( 'NONE', *, *, #15111, .T. ) ;
#32316 = CARTESIAN_POINT ( 'NONE',  ( 4.984135866956517447, 36.15314577889351000, 7.500000000000000888 ) ) ;
#32317 = DIRECTION ( 'NONE',  ( 0.000000000000000000, 0.000000000000000000, 1.000000000000000000 ) ) ;
#32318 = CARTESIAN_POINT ( 'NONE',  ( 13.47515517589329903, -22.56152428954667144, -16.35616346769606722 ) ) ;
#32319 = LINE ( 'NONE', #6708, #10047 ) ;
#32320 = DIRECTION ( 'NONE',  ( 0.000000000000000000, 0.000000000000000000, 1.000000000000000000 ) ) ;
#32321 = VERTEX_POINT ( 'NONE', #11375 ) ;
#32322 = CARTESIAN_POINT ( 'NONE',  ( -13.77105083670779173, 23.39240968089663397, -14.47666898018377779 ) ) ;
#32323 = CARTESIAN_POINT ( 'NONE',  ( -34.64424588158978935, -17.94331620955210127, 15.72805884748971650 ) ) ;
#32324 = CARTESIAN_POINT ( 'NONE',  ( 12.54367332990374173, -23.06920662023509294, -15.48107427365479261 ) ) ;
#32325 = CARTESIAN_POINT ( 'NONE',  ( 8.118377661053324701, 10.47536095541698486, 11.00000000000000000 ) ) ;
#32326 = VERTEX_POINT ( 'NONE', #35552 ) ;
#32327 = ORIENTED_EDGE ( 'NONE', *, *, #7543, .T. ) ;
#32328 = CARTESIAN_POINT ( 'NONE',  ( -13.31194575400795443, 31.44560903785412265, -5.455421079577211785 ) ) ;
#32329 = CARTESIAN_POINT ( 'NONE',  ( -12.11431924477676425, -16.53859993892360336, -29.29246340206837473 ) ) ;
#32330 = CARTESIAN_POINT ( 'NONE',  ( 4.082600654608392610, 21.41965916404854298, 6.000000000000000000 ) ) ;
#32331 = CIRCLE ( 'NONE', #14812, 0.9999999999999974465 ) ;
#32332 = CIRCLE ( 'NONE', #32982, 21.00000000000002842 ) ;
#32333 = CARTESIAN_POINT ( 'NONE',  ( -34.62559140834917315, -8.582204632672675970, -8.048554430461706488 ) ) ;
#32334 = DIRECTION ( 'NONE',  ( 1.000000000000000000, 0.000000000000000000, 0.000000000000000000 ) ) ;
#32335 = EDGE_LOOP ( 'NONE', ( #25202, #18513, #1399, #23261 ) ) ;
#32336 = CARTESIAN_POINT ( 'NONE',  ( 30.34379296090365941, 0.1366719566521715779, -7.828841148755459223 ) ) ;
#32337 = CARTESIAN_POINT ( 'NONE',  ( -5.400683141673551901, 15.91724817395922997, 7.000000000000000000 ) ) ;
#32338 = DIRECTION ( 'NONE',  ( 0.000000000000000000, 0.000000000000000000, 1.000000000000000000 ) ) ;
#32339 = EDGE_CURVE ( 'NONE', #31037, #32234, #30157, .T. ) ;
#32340 = UNCERTAINTY_MEASURE_WITH_UNIT (LENGTH_MEASURE( 1.000000000000000082E-05 ), #8111, 'distance_accuracy_value', 'NONE');
#32341 = CONICAL_SURFACE ( 'NONE', #23256, 1.000000000000004441, 0.7853981633974522758 ) ;
#32342 = EDGE_LOOP ( 'NONE', ( #17507, #25066, #6968 ) ) ;
#32343 = CARTESIAN_POINT ( 'NONE',  ( -20.69487421836006291, 0.8272276961458596700, -27.44708463700338541 ) ) ;
#32344 = CARTESIAN_POINT ( 'NONE',  ( -5.558911028763774631, 36.44455752850708308, 10.49999999999999822 ) ) ;
#32345 = VERTEX_POINT ( 'NONE', #4866 ) ;
#32346 = CARTESIAN_POINT ( 'NONE',  ( 21.97238824968331627, -1.114103264437971808, -23.63409279004794072 ) ) ;
#32347 = AXIS2_PLACEMENT_3D ( 'NONE', #36339, #8094, #11152 ) ;
#32348 = LINE ( 'NONE', #35391, #23915 ) ;
#32349 = CARTESIAN_POINT ( 'NONE',  ( 20.70549897995575961, -28.06280627726307486, 15.13084544680213384 ) ) ;
#32350 = ORIENTED_EDGE ( 'NONE', *, *, #5168, .T. ) ;
#32351 = CARTESIAN_POINT ( 'NONE',  ( 5.109761443618928922, 37.66877327392104036, 16.30093088680190760 ) ) ;
#32352 = CARTESIAN_POINT ( 'NONE',  ( 10.71169154830999659, -23.81371503812557222, 17.92354375535058253 ) ) ;
#32353 = CYLINDRICAL_SURFACE ( 'NONE', #6550, 0.5000000000000004441 ) ;
#32354 = CARTESIAN_POINT ( 'NONE',  ( -3.858525888478689936, 28.90799431746169290, 20.82122704794051415 ) ) ;
#32355 = CARTESIAN_POINT ( 'NONE',  ( -2.494943660522439099, 10.76222879119470832, 6.000000000000000000 ) ) ;
#32356 = ADVANCED_FACE ( 'NONE', ( #5071 ), #20117, .T. ) ;
#32357 = CARTESIAN_POINT ( 'NONE',  ( 8.339609403135806787, 11.87216320208440479, 9.500000000000000000 ) ) ;
#32358 = CIRCLE ( 'NONE', #38182, 0.5000000000000007772 ) ;
#32360 = VECTOR ( 'NONE', #29214, 1000.000000000000000 ) ;
#32359 = CARTESIAN_POINT ( 'NONE',  ( 3.957996558887789451, 29.70837811692673469, -15.71455925150293176 ) ) ;
#32361 = CARTESIAN_POINT ( 'NONE',  ( 17.34253826607186255, 27.32041144404028543, -5.000000000000000000 ) ) ;
#32363 = EDGE_CURVE ( 'NONE', #17409, #6680, #2034, .T. ) ;
#32362 = CIRCLE ( 'NONE', #10964, 16.99999999999999645 ) ;
#32364 = CARTESIAN_POINT ( 'NONE',  ( 16.15127118876671020, 15.63943246416513588, 18.87996532025803376 ) ) ;
#32365 = CARTESIAN_POINT ( 'NONE',  ( -19.26428189677079317, 7.107870580791990633, -28.84674469903880123 ) ) ;
#32366 = EDGE_CURVE ( 'NONE', #2590, #15085, #1423, .T. ) ;
#32367 = CARTESIAN_POINT ( 'NONE',  ( 18.47528072167350643, -21.61393943133635531, -15.95044983778787895 ) ) ;
#32368 = CIRCLE ( 'NONE', #14850, 1.000000000000000888 ) ;
#32369 = CARTESIAN_POINT ( 'NONE',  ( -12.39464589777671044, 26.66807349098043289, 13.00000000000000178 ) ) ;
#32370 = ORIENTED_EDGE ( 'NONE', *, *, #23048, .F. ) ;
#32371 = CARTESIAN_POINT ( 'NONE',  ( 10.89890768951664946, 17.41657833809615141, -28.70249223529265947 ) ) ;
#32372 = EDGE_LOOP ( 'NONE', ( #640, #22477, #38861, #23312 ) ) ;
#32373 = CARTESIAN_POINT ( 'NONE',  ( -15.78519146989449951, 25.10981109001613731, -6.891642859120278963 ) ) ;
#32374 = CARTESIAN_POINT ( 'NONE',  ( -31.66906069137318624, -9.703676519219762042, 19.27171037444156099 ) ) ;
#32375 = CARTESIAN_POINT ( 'NONE',  ( -14.26729173199937684, 26.60999298350843389, 10.87262190629277647 ) ) ;
#32376 = CARTESIAN_POINT ( 'NONE',  ( 14.05944288250579888, 23.86579217215976101, -13.51649411389087696 ) ) ;
#32377 = ORIENTED_EDGE ( 'NONE', *, *, #39823, .F. ) ;
#32378 = CARTESIAN_POINT ( 'NONE',  ( 33.04045786196795120, -19.54937996555464963, -6.275779577593939784 ) ) ;
#32379 = EDGE_LOOP ( 'NONE', ( #33502, #13942 ) ) ;
#32381 = DIRECTION ( 'NONE',  ( 0.000000000000000000, 0.000000000000000000, -1.000000000000000000 ) ) ;
#32380 = CARTESIAN_POINT ( 'NONE',  ( -14.99270781980373179, 26.86396254207275547, -8.275605574745005910 ) ) ;
#32382 = B_SPLINE_CURVE_WITH_KNOTS ( 'NONE', 3,
 ( #27877, #8998, #15089, #25028, #21580, #12435 ),
 .UNSPECIFIED., .F., .F.,
 ( 4, 2, 4 ),
 ( 0.000000000000000000, 0.5000000000000000000, 1.000000000000000000 ),
 .UNSPECIFIED. ) ;
#32383 = CARTESIAN_POINT ( 'NONE',  ( -16.22334360803714404, -26.92298677526160233, -5.470646933448687577 ) ) ;
#32384 = DIRECTION ( 'NONE',  ( 1.000000000000000000, 0.000000000000000000, 0.000000000000000000 ) ) ;
#32385 = VERTEX_POINT ( 'NONE', #29651 ) ;
#32386 = CARTESIAN_POINT ( 'NONE',  ( -33.38192493758457857, -13.76034026150677647, -9.745630752933474028 ) ) ;
#32387 = CARTESIAN_POINT ( 'NONE',  ( -14.54159974610060502, -26.13620151684259341, -8.302464661525958078 ) ) ;
#32388 = CARTESIAN_POINT ( 'NONE',  ( -5.440908595777639079, 35.94977745735568675, 11.00000000000000000 ) ) ;
#32389 = CARTESIAN_POINT ( 'NONE',  ( 14.48425105757694276, 16.48989445216367500, -21.99809950758036337 ) ) ;
#32390 = ORIENTED_EDGE ( 'NONE', *, *, #38942, .T. ) ;
#32391 = CARTESIAN_POINT ( 'NONE',  ( 25.79239026209233288, 2.921625702708928962, -13.66086306012633500 ) ) ;
#32392 = CARTESIAN_POINT ( 'NONE',  ( -9.806982162272253944, 13.84996144622306247, 13.00000000000000178 ) ) ;
#32393 = ADVANCED_FACE ( 'NONE', ( #33117 ), #1834, .T. ) ;
#32394 = CARTESIAN_POINT ( 'NONE',  ( -38.42882785865835160, -4.479089857567120525, 23.00000000000094147 ) ) ;
#32395 = EDGE_CURVE ( 'NONE', #6243, #29659, #11170, .T. ) ;
#32396 = VERTEX_POINT ( 'NONE', #35353 ) ;
#32397 = CARTESIAN_POINT ( 'NONE',  ( -20.98656222130776072, 0.6382380030884662325, -26.20988820701830946 ) ) ;
#32399 = CARTESIAN_POINT ( 'NONE',  ( 21.31785039509857782, 0.4639204330908863749, -24.98034756807314238 ) ) ;
#32398 = AXIS2_PLACEMENT_3D ( 'NONE', #8979, #17537, #5924 ) ;
#32400 = CIRCLE ( 'NONE', #18758, 0.4999999999999998335 ) ;
#32401 = CARTESIAN_POINT ( 'NONE',  ( 24.52800942765090753, -23.26501842005243148, 18.87996532025785967 ) ) ;
#32402 = ORIENTED_EDGE ( 'NONE', *, *, #28126, .F. ) ;
#32403 = CARTESIAN_POINT ( 'NONE',  ( -25.99398016003019762, 1.074985532622513063, -15.51177067371635587 ) ) ;
#32404 = CIRCLE ( 'NONE', #14876, 1.000000000000000000 ) ;
#32405 = CARTESIAN_POINT ( 'NONE',  ( -13.47223693944937040, 18.09844039693852125, -29.99999999999999645 ) ) ;
#32406 = CARTESIAN_POINT ( 'NONE',  ( -6.607858460703655901, 34.88289976392069747, 9.500000000000000000 ) ) ;
#32407 = CARTESIAN_POINT ( 'NONE',  ( 14.02783499842348647, 22.03112340962107751, 9.500000000000000000 ) ) ;
#32408 = EDGE_CURVE ( 'NONE', #4328, #37515, #31431, .T. ) ;
#32409 = DIRECTION ( 'NONE',  ( 1.000000000000000000, 0.000000000000000000, 0.000000000000000000 ) ) ;
#32410 = CYLINDRICAL_SURFACE ( 'NONE', #13213, 0.4999999999999997224 ) ;
#32411 = CARTESIAN_POINT ( 'NONE',  ( -0.5000000000000008882, 36.00000000000000711, 10.50000000000000000 ) ) ;
#32412 = EDGE_LOOP ( 'NONE', ( #30206, #39032, #25534, #40133 ) ) ;
#32413 = CARTESIAN_POINT ( 'NONE',  ( -12.41268156625113406, 18.79179606750104981, 13.00000000000000178 ) ) ;
#32414 = DIRECTION ( 'NONE',  ( 0.6691306063588662312, 0.7431448254773869166, 0.000000000000000000 ) ) ;
#32415 = CARTESIAN_POINT ( 'NONE',  ( 21.63954851288776382, -20.01129605949122592, -15.78715110015275691 ) ) ;
#32416 = CARTESIAN_POINT ( 'NONE',  ( 3.153820973115410098, 32.04219121950180238, 10.49999999999999822 ) ) ;
#32417 = CARTESIAN_POINT ( 'NONE',  ( 1.000000000000000666, 32.50000000000000000, 10.50000000000000178 ) ) ;
#32418 = CARTESIAN_POINT ( 'NONE',  ( 13.19794165967893740, 23.39120655137475779, -15.38553023868800196 ) ) ;
#32419 = DIRECTION ( 'NONE',  ( 0.000000000000000000, -0.000000000000000000, 1.000000000000000000 ) ) ;
#32420 = AXIS2_PLACEMENT_3D ( 'NONE', #23264, #14722, #30163 ) ;
#32421 = ORIENTED_EDGE ( 'NONE', *, *, #37180, .F. ) ;
#32422 = CARTESIAN_POINT ( 'NONE',  ( -16.78065708880074425, 18.17327365419953011, -13.77701268753624753 ) ) ;
#32423 = CYLINDRICAL_SURFACE ( 'NONE', #35466, 0.4999999999999986122 ) ;
#32424 = CARTESIAN_POINT ( 'NONE',  ( 14.97653007950890469, -26.12221433204903320, -8.768684533753454247 ) ) ;
#32425 = CARTESIAN_POINT ( 'NONE',  ( 14.31603901957230462, 19.98981538725069740, 10.50000000000000533 ) ) ;
#32426 = CARTESIAN_POINT ( 'NONE',  ( 11.13469544420071067, 17.60622615329656071, -26.83131557681828383 ) ) ;
#32427 = VERTEX_POINT ( 'NONE', #13607 ) ;
#32428 = CARTESIAN_POINT ( 'NONE',  ( 14.83827637938750321, 25.61447254529330664, -10.18026005582235527 ) ) ;
#32429 = VECTOR ( 'NONE', #33718, 1000.000000000000000 ) ;
#32430 = ORIENTED_EDGE ( 'NONE', *, *, #28271, .F. ) ;
#32432 = DIRECTION ( 'NONE',  ( 1.000000000000000000, 0.000000000000000000, 0.000000000000000000 ) ) ;
#32431 = CARTESIAN_POINT ( 'NONE',  ( -12.34392958471658730, 20.55351014499400364, -19.48636728564961373 ) ) ;
#32433 = CARTESIAN_POINT ( 'NONE',  ( -9.686854926055254111, -18.44287383492480714, -26.83074955385285421 ) ) ;
#32434 = CARTESIAN_POINT ( 'NONE',  ( -32.33143948541789570, 1.358872982501977633, 11.55979286843934872 ) ) ;
#32435 = CARTESIAN_POINT ( 'NONE',  ( -17.65620682731983848, -12.15726045169065550, -25.58993171772528541 ) ) ;
#32436 = CARTESIAN_POINT ( 'NONE',  ( -6.928215406011057453, -24.90100025669732631, -8.373177299821190189 ) ) ;
#32437 = CARTESIAN_POINT ( 'NONE',  ( 15.72808583165933172, 25.07803225150221493, -7.363722881524870090 ) ) ;
#32438 = ORIENTED_EDGE ( 'NONE', *, *, #19953, .T. ) ;
#32439 = CARTESIAN_POINT ( 'NONE',  ( 22.02868513814706830, 8.851876989647921690, -13.87910646370428580 ) ) ;
#32440 = CARTESIAN_POINT ( 'NONE',  ( 20.30751140574952629, -27.27504018040222533, -4.999999999999999112 ) ) ;
#32441 = CARTESIAN_POINT ( 'NONE',  ( 0.5000000000000000000, 37.00000000000000711, 10.99999999999999645 ) ) ;
#32442 = EDGE_CURVE ( 'NONE', #614, #16736, #23562, .T. ) ;
#32443 = DIRECTION ( 'NONE',  ( -0.000000000000000000, -0.000000000000000000, -1.000000000000000000 ) ) ;
#32444 = ORIENTED_EDGE ( 'NONE', *, *, #39892, .F. ) ;
#32445 = CARTESIAN_POINT ( 'NONE',  ( -20.64083728193717349, -1.144092991643025359, -27.97724812587252785 ) ) ;
#32446 = CARTESIAN_POINT ( 'NONE',  ( -5.578133564216631868, 24.05045924978127303, 20.99999999999999645 ) ) ;
#32447 = EDGE_LOOP ( 'NONE', ( #23763, #27243, #28437, #9631 ) ) ;
#32448 = CARTESIAN_POINT ( 'NONE',  ( 24.37759566069541250, -10.08322588119073693, 20.99999999999999645 ) ) ;
#32449 = CARTESIAN_POINT ( 'NONE',  ( 6.151085731882510288, 35.08626808545850650, 10.00000000000000000 ) ) ;
#32450 = CARTESIAN_POINT ( 'NONE',  ( -13.97557076678966403, 21.53386246193713305, 7.500000000000004441 ) ) ;
#32451 = CARTESIAN_POINT ( 'NONE',  ( 18.74042788058114795, -8.920399457985654479, -27.71296284416046518 ) ) ;
#32452 = CARTESIAN_POINT ( 'NONE',  ( 31.25372621196095935, -24.60616950719559526, 12.73282698324852724 ) ) ;
#32453 = CIRCLE ( 'NONE', #656, 6.000000000000005329 ) ;
#32454 = ORIENTED_EDGE ( 'NONE', *, *, #17127, .F. ) ;
#32455 = AXIS2_PLACEMENT_3D ( 'NONE', #11521, #20869, #5422 ) ;
#32456 = CARTESIAN_POINT ( 'NONE',  ( -2.871208588069141143, 13.69667159339610762, 6.000000000000000000 ) ) ;
#32457 = DIRECTION ( 'NONE',  ( 1.000000000000000000, 0.000000000000000000, 0.000000000000000000 ) ) ;
#32458 = B_SPLINE_CURVE_WITH_KNOTS ( 'NONE', 3,
 ( #5732, #14884, #21570, #5530, #27467, #9185 ),
 .UNSPECIFIED., .F., .F.,
 ( 4, 2, 4 ),
 ( 0.000000000000000000, 0.5000000000000000000, 1.000000000000000000 ),
 .UNSPECIFIED. ) ;
#32459 = EDGE_CURVE ( 'NONE', #2015, #24787, #19911, .T. ) ;
#32460 = DIRECTION ( 'NONE',  ( 0.000000000000000000, 0.000000000000000000, 1.000000000000000000 ) ) ;
#32461 = EDGE_LOOP ( 'NONE', ( #35174, #30549, #38391, #6371 ) ) ;
#32462 = EDGE_CURVE ( 'NONE', #39039, #888, #24301, .T. ) ;
#32463 = CARTESIAN_POINT ( 'NONE',  ( -1.397011542984961219, 27.89542180380697189, -17.59998838210181660 ) ) ;
#32464 = FACE_OUTER_BOUND ( 'NONE', #7892, .T. ) ;
#32465 = DIRECTION ( 'NONE',  ( -0.000000000000000000, -0.000000000000000000, -1.000000000000000000 ) ) ;
#32466 = EDGE_CURVE ( 'NONE', #35419, #2211, #27206, .T. ) ;
#32467 = LINE ( 'NONE', #26357, #13033 ) ;
#32468 = CARTESIAN_POINT ( 'NONE',  ( 0.6237317017440463518, 25.43444280220171194, 13.00000000000000178 ) ) ;
#32469 = DIRECTION ( 'NONE',  ( 0.000000000000000000, 0.000000000000000000, 1.000000000000000000 ) ) ;
#32470 = CARTESIAN_POINT ( 'NONE',  ( 9.263407132367138530, 18.28842304576874156, -29.99999999999999645 ) ) ;
#32471 = PLANE ( 'NONE',  #25046 ) ;
#32472 = VERTEX_POINT ( 'NONE', #8922 ) ;
#32473 = CIRCLE ( 'NONE', #15667, 1.000000000000000888 ) ;
#32474 = EDGE_CURVE ( 'NONE', #27705, #27849, #15216, .T. ) ;
#32476 = LINE ( 'NONE', #13366, #20684 ) ;
#32475 = CARTESIAN_POINT ( 'NONE',  ( -19.66039451765587387, 12.90996750491107115, -13.90270306263754030 ) ) ;
#32477 = DIRECTION ( 'NONE',  ( 0.000000000000000000, 0.000000000000000000, 1.000000000000000000 ) ) ;
#32478 = CARTESIAN_POINT ( 'NONE',  ( 13.41104112211880128, -23.62643484690040907, -14.47296996873020092 ) ) ;
#32479 = CARTESIAN_POINT ( 'NONE',  ( 11.81630298851978722, 31.79381426990546089, 11.00000000000000000 ) ) ;
#32480 = CARTESIAN_POINT ( 'NONE',  ( 10.95101281418289219, 17.32990059288363582, -30.00000000000000355 ) ) ;
#32481 = CARTESIAN_POINT ( 'NONE',  ( -20.90924525106831666, -8.502318254486386451, -19.80438750953543803 ) ) ;
#32482 = CARTESIAN_POINT ( 'NONE',  ( 0.2655024426717602637, 36.24516302788250499, 6.000000000000000000 ) ) ;
#32483 = CARTESIAN_POINT ( 'NONE',  ( -18.43289261102269450, -17.30365355162674135, -19.79000791179135632 ) ) ;
#32484 = CARTESIAN_POINT ( 'NONE',  ( 3.713915702903541227, -23.75747772264873348, -12.86660365504189407 ) ) ;
#32485 = CARTESIAN_POINT ( 'NONE',  ( 13.89868614485595621, 23.12070620105854601, -14.49265882329358313 ) ) ;
#32486 = CARTESIAN_POINT ( 'NONE',  ( 21.08270858168392792, 12.99488455910146278, -5.967554639584160547 ) ) ;
#32487 = CARTESIAN_POINT ( 'NONE',  ( 5.440908595777817602, 35.94977745735560859, 7.000000000000000000 ) ) ;
#32489 = ORIENTED_EDGE ( 'NONE', *, *, #18379, .T. ) ;
#32488 = EDGE_CURVE ( 'NONE', #6492, #39980, #2283, .T. ) ;
#32490 = VECTOR ( 'NONE', #26201, 1000.000000000000000 ) ;
#32491 = CARTESIAN_POINT ( 'NONE',  ( -6.053964587434877309, 34.92638846911022910, -10.20850310494260782 ) ) ;
#32492 = ADVANCED_FACE ( 'NONE', ( #27402 ), #33721, .T. ) ;
#32493 = VERTEX_POINT ( 'NONE', #30662 ) ;
#32494 = EDGE_CURVE ( 'NONE', #6257, #30063, #4863, .T. ) ;
#32495 = DIRECTION ( 'NONE',  ( 0.9945218953682740670, 0.1045284632676460046, 0.000000000000000000 ) ) ;
#32496 = ORIENTED_EDGE ( 'NONE', *, *, #4512, .F. ) ;
#32497 = DIRECTION ( 'NONE',  ( 0.000000000000000000, 0.000000000000000000, 1.000000000000000000 ) ) ;
#32498 = CARTESIAN_POINT ( 'NONE',  ( 9.997483185316561105, 21.95197631500756685, 10.50000000000000000 ) ) ;
#32499 = ORIENTED_EDGE ( 'NONE', *, *, #33684, .T. ) ;
#32500 = CARTESIAN_POINT ( 'NONE',  ( -30.61700640880846791, 0.08162764009042081104, -6.888198014876335762 ) ) ;
#32501 = EDGE_LOOP ( 'NONE', ( #32893, #9552, #10790, #18157 ) ) ;
#32502 = CARTESIAN_POINT ( 'NONE',  ( 20.02039722198771088, -4.740659622082477931, -28.52478632098719658 ) ) ;
#32503 = VECTOR ( 'NONE', #18169, 1000.000000000000114 ) ;
#32504 = CIRCLE ( 'NONE', #29879, 1.000000000000013101 ) ;
#32505 = VERTEX_POINT ( 'NONE', #11572 ) ;
#32506 = DIRECTION ( 'NONE',  ( 0.000000000000000000, 0.000000000000000000, 1.000000000000000000 ) ) ;
#32507 = CARTESIAN_POINT ( 'NONE',  ( -5.746222359017808756, 39.55816310746045872, 11.00000000000000355 ) ) ;
#32508 = VERTEX_POINT ( 'NONE', #24559 ) ;
#32509 = DIRECTION ( 'NONE',  ( 1.000000000000000000, 0.000000000000000000, 0.000000000000000000 ) ) ;
#32510 = DIRECTION ( 'NONE',  ( -0.8660254037844431485, -0.4999999999999921174, 0.000000000000000000 ) ) ;
#32511 = ADVANCED_FACE ( 'NONE', ( #12165 ), #14817, .T. ) ;
#32512 = CARTESIAN_POINT ( 'NONE',  ( -11.36267260525735168, 30.20759924275325758, 18.42518152272108622 ) ) ;
#32513 = CARTESIAN_POINT ( 'NONE',  ( -11.60262927932668298, 31.67393310092496961, 10.49999999999999822 ) ) ;
#32514 = VERTEX_POINT ( 'NONE', #36955 ) ;
#32515 = EDGE_CURVE ( 'NONE', #27237, #25471, #12363, .T. ) ;
#32516 =( NAMED_UNIT ( * ) SI_UNIT ( $, .STERADIAN. ) SOLID_ANGLE_UNIT ( ) );
#32517 = DIRECTION ( 'NONE',  ( 0.3090169943749573878, 0.9510565162951503115, 0.000000000000000000 ) ) ;
#32518 = CARTESIAN_POINT ( 'NONE',  ( -14.47283171447380035, 21.48159823030330884, 9.000000000000001776 ) ) ;
#32519 = AXIS2_PLACEMENT_3D ( 'NONE', #37996, #4061, #35149 ) ;
#32520 = CARTESIAN_POINT ( 'NONE',  ( -14.84160187385924523, 20.32586711126994672, 7.000000000000000000 ) ) ;
#32521 = CARTESIAN_POINT ( 'NONE',  ( 15.35486525779784728, 13.76085684245165552, -27.69159219027432783 ) ) ;
#32522 = CARTESIAN_POINT ( 'NONE',  ( 7.493380996195920574, 25.92983308932212339, -17.81133628007513892 ) ) ;
#32523 = VERTEX_POINT ( 'NONE', #36755 ) ;
#32524 = DIRECTION ( 'NONE',  ( 1.000000000000000000, 0.000000000000000000, 0.000000000000000000 ) ) ;
#32525 = DIRECTION ( 'NONE',  ( 1.000000000000000000, 0.000000000000000000, 0.000000000000000000 ) ) ;
#32526 = CARTESIAN_POINT ( 'NONE',  ( 10.39272730050880789, -19.10536722629138140, -23.83256194882331869 ) ) ;
#32527 = DIRECTION ( 'NONE',  ( 0.000000000000000000, 0.000000000000000000, 1.000000000000000000 ) ) ;
#32528 = DIRECTION ( 'NONE',  ( 0.1045284632676569680, 0.9945218953682730678, -0.000000000000000000 ) ) ;
#32529 = ORIENTED_EDGE ( 'NONE', *, *, #25537, .T. ) ;
#32530 = CARTESIAN_POINT ( 'NONE',  ( -14.28250818835134872, 24.49381330739200990, -12.54868123938283375 ) ) ;
#32531 = AXIS2_PLACEMENT_3D ( 'NONE', #26854, #20963, #14866 ) ;
#32532 = CARTESIAN_POINT ( 'NONE',  ( -36.05338440271489731, -10.94427667939905824, 15.72805884749021033 ) ) ;
#32533 = CARTESIAN_POINT ( 'NONE',  ( 11.58908824346749178, -21.50996719514929723, -18.48308237374000029 ) ) ;
#32534 = VECTOR ( 'NONE', #15857, 1000.000000000000000 ) ;
#32535 = DIRECTION ( 'NONE',  ( 0.000000000000000000, 0.000000000000000000, 1.000000000000000000 ) ) ;
#32536 = ORIENTED_EDGE ( 'NONE', *, *, #2965, .T. ) ;
#32537 = ORIENTED_EDGE ( 'NONE', *, *, #9642, .T. ) ;
#32538 = CARTESIAN_POINT ( 'NONE',  ( -7.847358392957297646, 19.47655254888744736, -26.54680820890942883 ) ) ;
#32539 = PLANE ( 'NONE',  #4243 ) ;
#32540 = FACE_BOUND ( 'NONE', #9975, .T. ) ;
#32541 = CARTESIAN_POINT ( 'NONE',  ( -34.16618095875499250, -7.443595052282137914, -8.509874465049289682 ) ) ;
#32542 = CARTESIAN_POINT ( 'NONE',  ( 8.160254037844358876, 16.63397459621553054, 10.49999999999999822 ) ) ;
#32543 = ORIENTED_EDGE ( 'NONE', *, *, #30990, .T. ) ;
#32544 = CARTESIAN_POINT ( 'NONE',  ( 25.75329700475152706, 0.5046424211543979466, -16.46013763815398789 ) ) ;
#32545 = CARTESIAN_POINT ( 'NONE',  ( -10.50986403156571036, 32.63594044384558401, 10.99387789255783510 ) ) ;
#32546 = DIRECTION ( 'NONE',  ( -1.000000000000000000, 0.000000000000000000, 0.000000000000000000 ) ) ;
#32547 = LINE ( 'NONE', #9992, #1157 ) ;
#32548 = ORIENTED_EDGE ( 'NONE', *, *, #26435, .T. ) ;
#32549 = CARTESIAN_POINT ( 'NONE',  ( -29.99827651847404297, 0.02216799781674966274, -9.238322543644144957 ) ) ;
#32550 = FACE_OUTER_BOUND ( 'NONE', #6317, .T. ) ;
#32551 = VERTEX_POINT ( 'NONE', #11768 ) ;
#32552 = CARTESIAN_POINT ( 'NONE',  ( 26.14237992437378466, -1.587135967906720291, -17.20498952483474042 ) ) ;
#32553 = CARTESIAN_POINT ( 'NONE',  ( 25.86085639998011132, -26.44089909996149501, 15.72805884748939853 ) ) ;
#32554 = VERTEX_POINT ( 'NONE', #24154 ) ;
#32555 = CARTESIAN_POINT ( 'NONE',  ( 15.39524332970993470, 28.62968336403817204, 15.72805884749054250 ) ) ;
#32556 = CARTESIAN_POINT ( 'NONE',  ( -15.37000524123853218, -27.20210912714291496, 15.72805884748939498 ) ) ;
#32557 = LINE ( 'NONE', #38639, #15644 ) ;
#32558 = CARTESIAN_POINT ( 'NONE',  ( 2.638259136957625817, 30.33190274691521182, 20.69868183039781329 ) ) ;
#32559 = DIRECTION ( 'NONE',  ( 0.5778781230733963659, 0.000000000000000000, 0.8161230758122015594 ) ) ;
#32560 = ORIENTED_EDGE ( 'NONE', *, *, #442, .F. ) ;
#32561 = AXIS2_PLACEMENT_3D ( 'NONE', #33114, #8716, #27203 ) ;
#32562 = CARTESIAN_POINT ( 'NONE',  ( 13.24038105676655164, 15.43301270189216368, 10.49999999999999822 ) ) ;
#32563 = CARTESIAN_POINT ( 'NONE',  ( 2.292311336812923095, 22.67302623323931243, -23.01638908516527238 ) ) ;
#32564 = CARTESIAN_POINT ( 'NONE',  ( -14.23945615837876311, -31.58416516429889853, 0.000000000000000000 ) ) ;
#32565 = CARTESIAN_POINT ( 'NONE',  ( 24.07200259733946979, 7.872448391868417161, 16.30093088680184366 ) ) ;
#32566 = CONICAL_SURFACE ( 'NONE', #9852, 0.5000000000000023315, 0.7853981633974492782 ) ;
#32567 = CARTESIAN_POINT ( 'NONE',  ( 16.07137580887406969, -18.82834282195213405, -19.98174329064899979 ) ) ;
#32568 = DIRECTION ( 'NONE',  ( -1.000000000000000000, 0.000000000000000000, 0.000000000000000000 ) ) ;
#32569 = FACE_OUTER_BOUND ( 'NONE', #33065, .T. ) ;
#32570 = DIRECTION ( 'NONE',  ( 1.000000000000000000, 0.000000000000000000, 0.000000000000000000 ) ) ;
#32571 = ORIENTED_EDGE ( 'NONE', *, *, #19718, .T. ) ;
#32572 = CARTESIAN_POINT ( 'NONE',  ( 11.23935683279430364, 18.09303880744939619, -25.00484586747397842 ) ) ;
#32573 = ORIENTED_EDGE ( 'NONE', *, *, #9889, .T. ) ;
#32574 = CARTESIAN_POINT ( 'NONE',  ( -11.42515256197113693, 17.40157771485680627, -26.85803077672003525 ) ) ;
#32575 = CARTESIAN_POINT ( 'NONE',  ( -29.77970073067859147, -14.50783476829564300, 19.99202127657101613 ) ) ;
#32576 = CARTESIAN_POINT ( 'NONE',  ( -14.42035624161472995, 26.65972665747678505, 10.49999999999999112 ) ) ;
#32577 = CARTESIAN_POINT ( 'NONE',  ( 12.96728218553863954, 21.59012440819528322, -17.44419411314543567 ) ) ;
#32578 = ORIENTED_EDGE ( 'NONE', *, *, #26869, .F. ) ;
#32579 = CARTESIAN_POINT ( 'NONE',  ( 32.16900669001064728, -16.47211036377505167, -10.17477865279244043 ) ) ;
#32580 = ORIENTED_EDGE ( 'NONE', *, *, #25892, .T. ) ;
#32582 = DIRECTION ( 'NONE',  ( 0.000000000000000000, 0.000000000000000000, 1.000000000000000000 ) ) ;
#32581 = CARTESIAN_POINT ( 'NONE',  ( -11.12826152366268850, 18.17846884760333381, -24.98958924420576722 ) ) ;
#32583 = CARTESIAN_POINT ( 'NONE',  ( -17.02243939560907648, -26.72822735494350965, -7.774529914931894936 ) ) ;
#32584 = B_SPLINE_CURVE_WITH_KNOTS ( 'NONE', 3,
 ( #22064, #28758, #21862, #933 ),
 .UNSPECIFIED., .F., .F.,
 ( 4, 4 ),
 ( 0.000000000000000000, 0.0001748523089235895619 ),
 .UNSPECIFIED. ) ;
#32585 = DIRECTION ( 'NONE',  ( 0.8090169943749423442, -0.5877852522924800205, 0.000000000000000000 ) ) ;
#32586 = ORIENTED_EDGE ( 'NONE', *, *, #35900, .F. ) ;
#32587 = CARTESIAN_POINT ( 'NONE',  ( -19.77651789229256352, -8.197028377600723559, -25.61779185879715115 ) ) ;
#32588 = CARTESIAN_POINT ( 'NONE',  ( -11.55200745323391764, -21.51294090668309167, -18.48664492717743713 ) ) ;
#32589 = CARTESIAN_POINT ( 'NONE',  ( 37.88915195766877275, -19.37406375362064992, 22.99999999999999289 ) ) ;
#32590 = CARTESIAN_POINT ( 'NONE',  ( 16.82875782630935291, 20.37066115841360059, -10.28574066425471933 ) ) ;
#32591 = ORIENTED_EDGE ( 'NONE', *, *, #821, .F. ) ;
#32592 = CARTESIAN_POINT ( 'NONE',  ( 25.33665828877437320, 2.928795514553437673, -14.64692555173594357 ) ) ;
#32593 = ADVANCED_FACE ( 'NONE', ( #21504 ), #39791, .T. ) ;
#32594 = FACE_OUTER_BOUND ( 'NONE', #23444, .T. ) ;
#32595 = CARTESIAN_POINT ( 'NONE',  ( 7.935770203493858865, 22.34671014717335780, 13.00000000000000178 ) ) ;
#32596 = ORIENTED_EDGE ( 'NONE', *, *, #11946, .T. ) ;
#32597 = CARTESIAN_POINT ( 'NONE',  ( -30.95948536022075359, -0.1350361458710127027, -5.944726679833734373 ) ) ;
#32598 = CARTESIAN_POINT ( 'NONE',  ( 20.85121071602917553, 0.3501234034299393616, -26.79320176925520514 ) ) ;
#32599 = EDGE_CURVE ( 'NONE', #38623, #19050, #10560, .T. ) ;
#32600 = CARTESIAN_POINT ( 'NONE',  ( 30.79094061804850568, -13.52614530981714225, 19.66345542862527651 ) ) ;
#32601 = EDGE_LOOP ( 'NONE', ( #1456, #31762, #30818, #20060 ) ) ;
#32602 = AXIS2_PLACEMENT_3D ( 'NONE', #18209, #14954, #11510 ) ;
#32603 = CARTESIAN_POINT ( 'NONE',  ( -28.85560228327580390, 1.748727845287112448, -7.841872307111799500 ) ) ;
#32604 = EDGE_CURVE ( 'NONE', #35381, #21382, #36355, .T. ) ;
#32605 = CARTESIAN_POINT ( 'NONE',  ( -18.07620401364299667, 24.68088026512193167, -13.58461195433497082 ) ) ;
#32606 = DIRECTION ( 'NONE',  ( 0.000000000000000000, 0.000000000000000000, 1.000000000000000000 ) ) ;
#32607 = AXIS2_PLACEMENT_3D ( 'NONE', #34230, #37272, #18594 ) ;
#32608 = DIRECTION ( 'NONE',  ( 1.000000000000000000, 0.000000000000000000, 0.000000000000000000 ) ) ;
#32609 = CARTESIAN_POINT ( 'NONE',  ( 0.5000000000000000000, 37.00000000000000711, 11.00000000000000000 ) ) ;
#32610 = CARTESIAN_POINT ( 'NONE',  ( 6.460609604078280555, 35.78147008481143132, 10.94611345180490680 ) ) ;
#32611 = AXIS2_PLACEMENT_3D ( 'NONE', #12665, #81, #9027 ) ;
#32612 = LINE ( 'NONE', #28943, #33481 ) ;
#32613 = ORIENTED_EDGE ( 'NONE', *, *, #164, .T. ) ;
#32614 = CARTESIAN_POINT ( 'NONE',  ( -25.53096875586516390, 6.216240356532259703, -5.000000000000001776 ) ) ;
#32615 = EDGE_CURVE ( 'NONE', #21181, #12596, #8518, .T. ) ;
#32616 = CARTESIAN_POINT ( 'NONE',  ( -6.557822374958091949, 35.99981354310121873, 10.59344459855558540 ) ) ;
#32617 = ADVANCED_FACE ( 'NONE', ( #9323 ), #26263, .T. ) ;
#32618 = DIRECTION ( 'NONE',  ( 0.9781476007338069101, 0.2079116908177532641, 0.000000000000000000 ) ) ;
#32619 = CARTESIAN_POINT ( 'NONE',  ( 27.75063338421220749, -24.13809418093133274, -8.005686737521594765 ) ) ;
#32620 = DIRECTION ( 'NONE',  ( 0.9781476007338072431, 0.2079116908177519041, 0.000000000000000000 ) ) ;
#32621 = DIRECTION ( 'NONE',  ( 0.9659258262890655367, -0.2588190451025308980, -9.462988938997540172E-16 ) ) ;
#32622 = CARTESIAN_POINT ( 'NONE',  ( 14.77821352920928177, 26.27987808421032057, -9.682826709401501475 ) ) ;
#32623 = VECTOR ( 'NONE', #11871, 1000.000000000000114 ) ;
#32624 = CARTESIAN_POINT ( 'NONE',  ( -3.665809487923753274, 43.57847826359346755, 10.00000000000000000 ) ) ;
#32625 = VERTEX_POINT ( 'NONE', #5268 ) ;
#32626 = CARTESIAN_POINT ( 'NONE',  ( -15.52764069369276889, 16.28833658513694260, -19.93923883857963375 ) ) ;
#32627 = CARTESIAN_POINT ( 'NONE',  ( -19.84741737732755951, -16.23688957394095311, 20.99999999999999645 ) ) ;
#32628 = VECTOR ( 'NONE', #13, 1000.000000000000114 ) ;
#32629 = CARTESIAN_POINT ( 'NONE',  ( 9.636746047937265303, -18.46635915234381997, -26.83497180128339110 ) ) ;
#32630 = CARTESIAN_POINT ( 'NONE',  ( 22.42900687741999732, 24.35462947583785720, 11.00000000000000000 ) ) ;
#32631 = CARTESIAN_POINT ( 'NONE',  ( 14.84964465211067441, 25.58025656879111054, -10.18089330217375910 ) ) ;
#32632 = VERTEX_POINT ( 'NONE', #18073 ) ;
#32633 = CARTESIAN_POINT ( 'NONE',  ( 15.41298789278284964, 26.79417030376202291, -5.474208755804808035 ) ) ;
#32634 = ORIENTED_EDGE ( 'NONE', *, *, #4660, .T. ) ;
#32636 = DIRECTION ( 'NONE',  ( 0.000000000000000000, 0.000000000000000000, 1.000000000000000000 ) ) ;
#32635 = CARTESIAN_POINT ( 'NONE',  ( -11.63031588870816257, 18.96513858619488602, -22.72542786189888986 ) ) ;
#32637 = CARTESIAN_POINT ( 'NONE',  ( -14.61166790280883099, -25.45836085479211164, -10.65401685762440387 ) ) ;
#32638 = CARTESIAN_POINT ( 'NONE',  ( -35.68447701591262700, -3.401722300707700430, 11.00000000000000000 ) ) ;
#32639 = VECTOR ( 'NONE', #37816, 1000.000000000000000 ) ;
#32640 = CARTESIAN_POINT ( 'NONE',  ( -31.61852543657527903, -20.43336672873744675, -7.973887691128377142 ) ) ;
#32641 = CARTESIAN_POINT ( 'NONE',  ( -6.215971932975158154, -23.28253663301664389, -14.81238128996371195 ) ) ;
#32642 = CARTESIAN_POINT ( 'NONE',  ( 12.34902707657751186, 18.26588438466833608, -22.83901375834292224 ) ) ;
#32643 = ORIENTED_EDGE ( 'NONE', *, *, #28531, .T. ) ;
#32644 = CARTESIAN_POINT ( 'NONE',  ( 20.46894310308663734, 7.564869913809710411, -21.11451722641894690 ) ) ;
#32645 = CARTESIAN_POINT ( 'NONE',  ( -3.118675362266497775, 7.827785988992935096, 7.000000000000000000 ) ) ;
#32646 = CARTESIAN_POINT ( 'NONE',  ( 14.48927117870123027, -30.61587158504688233, 3.000000000000000000 ) ) ;
#32647 = CARTESIAN_POINT ( 'NONE',  ( 2.525645716490524606, 8.212903943950921715, 11.00000000000000000 ) ) ;
#32648 = ORIENTED_EDGE ( 'NONE', *, *, #21909, .F. ) ;
#32649 = CARTESIAN_POINT ( 'NONE',  ( -24.71030582546459442, -1.630746468800712279, -19.22827620953929184 ) ) ;
#32650 = ADVANCED_FACE ( 'NONE', ( #36550 ), #21113, .F. ) ;
#32651 = CARTESIAN_POINT ( 'NONE',  ( -21.27192666516830499, -1.272056932884052971, 20.69868183039990228 ) ) ;
#32652 = CARTESIAN_POINT ( 'NONE',  ( 25.15015781186010457, -9.899056496887492784, 20.99999999999999645 ) ) ;
#32653 = FACE_OUTER_BOUND ( 'NONE', #39855, .T. ) ;
#32654 = CIRCLE ( 'NONE', #13138, 1.000000000000013101 ) ;
#32655 = CARTESIAN_POINT ( 'NONE',  ( -9.665073660138984835, 25.11464168560199184, 10.50000000000000000 ) ) ;
#32656 = CARTESIAN_POINT ( 'NONE',  ( 18.51815053109030629, -8.815588134695456546, -29.21493728961338476 ) ) ;
#32657 = CARTESIAN_POINT ( 'NONE',  ( 31.38526299860050628, -24.75545609243360090, 11.00000000000000000 ) ) ;
#32658 = ORIENTED_EDGE ( 'NONE', *, *, #11589, .T. ) ;
#32659 = CARTESIAN_POINT ( 'NONE',  ( -10.29511041547401895, 24.79362192464190073, 10.50000000000000533 ) ) ;
#32660 = FACE_OUTER_BOUND ( 'NONE', #27460, .T. ) ;
#32661 = VECTOR ( 'NONE', #6497, 1000.000000000000000 ) ;
#32662 = CARTESIAN_POINT ( 'NONE',  ( 5.490944681523308724, 34.83286367817510154, 7.000000000000000000 ) ) ;
#32663 = CARTESIAN_POINT ( 'NONE',  ( -13.01838097023000707, 23.73363068877903359, 13.00000000000000178 ) ) ;
#32664 = CARTESIAN_POINT ( 'NONE',  ( 0.2270303117876434351, 21.43481588860569076, -25.57708852813776801 ) ) ;
#32665 = LINE ( 'NONE', #4214, #347 ) ;
#32666 = ADVANCED_FACE ( 'NONE', ( #25745 ), #28395, .F. ) ;
#32667 = DIRECTION ( 'NONE',  ( 1.000000000000000000, 0.000000000000000000, 0.000000000000000000 ) ) ;
#32668 = ADVANCED_FACE ( 'NONE', ( #38139 ), #10115, .F. ) ;
#32669 = FACE_OUTER_BOUND ( 'NONE', #29869, .T. ) ;
#32670 = CARTESIAN_POINT ( 'NONE',  ( 12.30736835487432934, 14.81698729810772797, 11.00000000000000000 ) ) ;
#32671 = AXIS2_PLACEMENT_3D ( 'NONE', #5025, #26757, #8476 ) ;
#32672 = FACE_OUTER_BOUND ( 'NONE', #4396, .T. ) ;
#32673 = CARTESIAN_POINT ( 'NONE',  ( 14.35878712486879039, 29.02377999103498496, -7.294375021701867468 ) ) ;
#32674 = CARTESIAN_POINT ( 'NONE',  ( 0.000000000000000000, 22.50000000000000355, 7.000000000000000000 ) ) ;
#32675 = ORIENTED_EDGE ( 'NONE', *, *, #22058, .F. ) ;
#32677 = CARTESIAN_POINT ( 'NONE',  ( 1.000000000000000222, 36.00000000000000711, 10.50000000000000000 ) ) ;
#32676 = CARTESIAN_POINT ( 'NONE',  ( -17.19661888337742184, 12.08206334730271791, -24.39846010520068731 ) ) ;
#32678 = CARTESIAN_POINT ( 'NONE',  ( 8.312035131040566682, 19.41226734497195849, 6.000000000000000000 ) ) ;
#32679 = CARTESIAN_POINT ( 'NONE',  ( 9.990270308899361851, -18.80412660014683013, -25.01178681032867956 ) ) ;
#32680 = DIRECTION ( 'NONE',  ( -0.5773502691896259531, -0.5773502691896217343, 0.5773502691896298389 ) ) ;
#32681 = CARTESIAN_POINT ( 'NONE',  ( 14.92120918266745733, 25.84352239596041301, -9.706504909383646407 ) ) ;
#32682 = CARTESIAN_POINT ( 'NONE',  ( -19.54664213359414404, -11.28525909758381829, -30.00000000000000711 ) ) ;
#32683 = DIRECTION ( 'NONE',  ( 1.000000000000000000, 0.000000000000000000, 0.000000000000000000 ) ) ;
#32684 = CARTESIAN_POINT ( 'NONE',  ( -23.72267846501879518, -21.04549334238744507, -13.87629623305566007 ) ) ;
#32685 = CARTESIAN_POINT ( 'NONE',  ( 3.569601909448802513, -23.23944431787124643, -14.89441082719224596 ) ) ;
#32686 = CARTESIAN_POINT ( 'NONE',  ( 11.47796835573551988, 17.90614830826391923, -25.03692986855586256 ) ) ;
#32687 = CARTESIAN_POINT ( 'NONE',  ( 20.05787158664475101, 13.58148755638892169, -10.87997266152090781 ) ) ;
#32688 = PRESENTATION_LAYER_ASSIGNMENT (  '', '', ( #39801 ) ) ;
#32689 = CARTESIAN_POINT ( 'NONE',  ( 0.5000000000000004441, 36.00000000000000711, 9.500000000000000000 ) ) ;
#32690 = EDGE_LOOP ( 'NONE', ( #32430, #1337, #5309, #570 ) ) ;
#32691 = CARTESIAN_POINT ( 'NONE',  ( -7.446792957322618811, 36.70800515527383823, -4.999999999999999112 ) ) ;
#32692 = ORIENTED_EDGE ( 'NONE', *, *, #19550, .T. ) ;
#32693 = EDGE_CURVE ( 'NONE', #22086, #29202, #34503, .T. ) ;
#32694 = VECTOR ( 'NONE', #10359, 1000.000000000000000 ) ;
#32695 = DIRECTION ( 'NONE',  ( -0.000000000000000000, -0.000000000000000000, 1.000000000000000000 ) ) ;
#32696 = ORIENTED_EDGE ( 'NONE', *, *, #14570, .T. ) ;
#32697 = CYLINDRICAL_SURFACE ( 'NONE', #24471, 19.99999999999993250 ) ;
#32698 = CARTESIAN_POINT ( 'NONE',  ( 8.927394655428274817, 11.06314620770945290, 11.00000000000000000 ) ) ;
#32699 = ORIENTED_EDGE ( 'NONE', *, *, #37592, .T. ) ;
#32700 = CARTESIAN_POINT ( 'NONE',  ( -21.25873018001586701, 0.9006927932260392344, -25.02786347552343926 ) ) ;
#32701 = ORIENTED_EDGE ( 'NONE', *, *, #8091, .F. ) ;
#32702 = CARTESIAN_POINT ( 'NONE',  ( 34.75575196650723342, -11.62799908373506419, -8.009968735996103817 ) ) ;
#32703 = AXIS2_PLACEMENT_3D ( 'NONE', #29551, #36054, #33219 ) ;
#32704 = VERTEX_POINT ( 'NONE', #9722 ) ;
#32705 = CONTEXT_DEPENDENT_SHAPE_REPRESENTATION ( #26205, #37585 ) ;
#32706 = CARTESIAN_POINT ( 'NONE',  ( 14.11133924723984379, 27.61078317377175750, 10.49999999999999822 ) ) ;
#32707 = ORIENTED_EDGE ( 'NONE', *, *, #26160, .T. ) ;
#32708 = DIRECTION ( 'NONE',  ( 1.000000000000000000, 0.000000000000000000, 0.000000000000000000 ) ) ;
#32709 = DIRECTION ( 'NONE',  ( 0.000000000000000000, 0.000000000000000000, 1.000000000000000000 ) ) ;
#32710 = CARTESIAN_POINT ( 'NONE',  ( -6.761248272854020414, 33.72770196150105448, 18.87996532025709229 ) ) ;
#32711 = AXIS2_PLACEMENT_3D ( 'NONE', #33960, #3276, #12222 ) ;
#32712 = DIRECTION ( 'NONE',  ( 0.7431448254773961315, 0.6691306063588561281, 0.000000000000000000 ) ) ;
#32713 = VERTEX_POINT ( 'NONE', #28000 ) ;
#32714 = DIRECTION ( 'NONE',  ( 1.000000000000000000, 0.000000000000000000, 0.000000000000000000 ) ) ;
#32715 = CARTESIAN_POINT ( 'NONE',  ( -2.672146553953451242, 12.33340603770395560, 11.00000000000000000 ) ) ;
#32716 = DIRECTION ( 'NONE',  ( 0.000000000000000000, 0.000000000000000000, 1.000000000000000000 ) ) ;
#32717 = EDGE_CURVE ( 'NONE', #34673, #860, #838, .T. ) ;
#32718 = CARTESIAN_POINT ( 'NONE',  ( 15.43899379198432165, 13.87320894201425858, -26.55943958658228254 ) ) ;
#32719 = CARTESIAN_POINT ( 'NONE',  ( 11.64958443988100711, 33.23480978958207999, -6.767891074995996625 ) ) ;
#32720 = AXIS2_PLACEMENT_3D ( 'NONE', #8468, #20867, #33268 ) ;
#32721 = ORIENTED_EDGE ( 'NONE', *, *, #24665, .T. ) ;
#32722 = DIRECTION ( 'NONE',  ( 1.000000000000000000, 0.000000000000000000, 0.000000000000000000 ) ) ;
#32723 = DIRECTION ( 'NONE',  ( 1.000000000000000000, 0.000000000000000000, 0.000000000000000000 ) ) ;
#32724 = CARTESIAN_POINT ( 'NONE',  ( 15.64462842542821797, -26.65633373546051743, -6.882370998507620463 ) ) ;
#32725 = DIRECTION ( 'NONE',  ( 0.9510565162951503115, -0.3090169943749572767, 0.000000000000000000 ) ) ;
#32726 = CARTESIAN_POINT ( 'NONE',  ( 5.473344025737210572, 14.11593743010426394, 10.49999999999999822 ) ) ;
#32727 = ORIENTED_EDGE ( 'NONE', *, *, #33389, .F. ) ;
#32728 = CARTESIAN_POINT ( 'NONE',  ( -14.28759343413927674, 24.48013941304578367, -12.54985307008666418 ) ) ;
#32729 = CARTESIAN_POINT ( 'NONE',  ( -33.13502155305637586, -2.712192412331239755, 16.30093088680144930 ) ) ;
#32730 = CARTESIAN_POINT ( 'NONE',  ( 13.61137063728712349, -26.17156308209870019, -6.892411826510384643 ) ) ;
#32731 = CARTESIAN_POINT ( 'NONE',  ( 8.312035131040566682, 19.41226734497195849, 13.00000000000000178 ) ) ;
#32732 = ORIENTED_EDGE ( 'NONE', *, *, #36802, .F. ) ;
#32733 = ORIENTED_EDGE ( 'NONE', *, *, #23505, .T. ) ;
#32734 = CARTESIAN_POINT ( 'NONE',  ( -8.174017679424943950, 22.40856258689699843, -21.07428364536496446 ) ) ;
#32735 = DIRECTION ( 'NONE',  ( 0.000000000000000000, 0.000000000000000000, 1.000000000000000000 ) ) ;
#32736 = EDGE_CURVE ( 'NONE', #25142, #3653, #19249, .T. ) ;
#32737 = FACE_BOUND ( 'NONE', #12480, .T. ) ;
#32738 = AXIS2_PLACEMENT_3D ( 'NONE', #12374, #37359, #3032 ) ;
#32739 = CARTESIAN_POINT ( 'NONE',  ( -31.44780373369627924, -5.846625527196687599, -12.15987862009057707 ) ) ;
#32740 = DIRECTION ( 'NONE',  ( 0.000000000000000000, 0.000000000000000000, 1.000000000000000000 ) ) ;
#32741 = ORIENTED_EDGE ( 'NONE', *, *, #3395, .F. ) ;
#32742 = CARTESIAN_POINT ( 'NONE',  ( 30.80134931806678722, 0.02728179087148215054, -5.946091737772539076 ) ) ;
#32743 = EDGE_CURVE ( 'NONE', #5091, #38482, #5238, .T. ) ;
#32744 = CARTESIAN_POINT ( 'NONE',  ( -10.81260707898156959, 32.90853150812147021, 10.59344459855568843 ) ) ;
#32745 = DIRECTION ( 'NONE',  ( 0.2079116908177532919, -0.9781476007338070211, -0.000000000000000000 ) ) ;
#32746 = CARTESIAN_POINT ( 'NONE',  ( -1.485571585149857210, -11.24999999999982236, 6.000000000000000000 ) ) ;
#32747 = ORIENTED_EDGE ( 'NONE', *, *, #15720, .F. ) ;
#32748 = CARTESIAN_POINT ( 'NONE',  ( -23.93868645767142311, 0.4905013439724816293, -19.49701671461600938 ) ) ;
#32749 = CARTESIAN_POINT ( 'NONE',  ( -13.97943872024075951, 27.84235072122942611, 10.49999999999999822 ) ) ;
#32750 = ORIENTED_EDGE ( 'NONE', *, *, #35246, .T. ) ;
#32751 = CARTESIAN_POINT ( 'NONE',  ( 31.41098121239500784, -3.786779113504257221, -11.32952589658759024 ) ) ;
#32752 = VECTOR ( 'NONE', #32197, 1000.000000000000114 ) ;
#32753 = EDGE_CURVE ( 'NONE', #20104, #39848, #19450, .T. ) ;
#32754 = CARTESIAN_POINT ( 'NONE',  ( 17.04089262280485073, -28.02826808822959137, 15.13084544680119059 ) ) ;
#32755 = ORIENTED_EDGE ( 'NONE', *, *, #37592, .F. ) ;
#32756 = CARTESIAN_POINT ( 'NONE',  ( 16.50691157469017867, 29.07214648649524591, 13.32518128616620778 ) ) ;
#32757 = CARTESIAN_POINT ( 'NONE',  ( -15.89892447184056756, -25.15199583021358265, 17.92354375535250810 ) ) ;
#32758 = DIRECTION ( 'NONE',  ( 1.000000000000000000, 0.000000000000000000, 0.000000000000000000 ) ) ;
#32759 = CARTESIAN_POINT ( 'NONE',  ( 3.137032374298201365, 29.29040802067843074, 20.82122704794080192 ) ) ;
#32760 = LINE ( 'NONE', #10411, #13558 ) ;
#32761 = ORIENTED_EDGE ( 'NONE', *, *, #23736, .F. ) ;
#32762 = CARTESIAN_POINT ( 'NONE',  ( -7.748210172783978500, 9.655561136695068214, 7.102637441331450141 ) ) ;
#32763 = ADVANCED_FACE ( 'NONE', ( #22296 ), #12562, .T. ) ;
#32764 = EDGE_CURVE ( 'NONE', #9924, #22293, #18505, .T. ) ;
#32765 = AXIS2_PLACEMENT_3D ( 'NONE', #11583, #26817, #29263 ) ;
#32766 = CARTESIAN_POINT ( 'NONE',  ( 4.894819805308785909, 36.72758954802892362, -8.421019001303848839 ) ) ;
#32767 = FACE_OUTER_BOUND ( 'NONE', #3302, .T. ) ;
#32768 = CARTESIAN_POINT ( 'NONE',  ( 14.75813536907442192, 8.520613428072293161, 20.69868183039781329 ) ) ;
#32769 = CARTESIAN_POINT ( 'NONE',  ( 18.34994596701333691, -24.10411726525174458, -13.18475438623739926 ) ) ;
#32770 = FACE_OUTER_BOUND ( 'NONE', #32989, .T. ) ;
#32771 = VECTOR ( 'NONE', #28952, 1000.000000000000227 ) ;
#32772 = CARTESIAN_POINT ( 'NONE',  ( -35.10501578368283049, -15.25571008401125717, -4.999999999999999112 ) ) ;
#32773 = CARTESIAN_POINT ( 'NONE',  ( -4.817371740575545402, 23.83900317890010001, 23.00000000000000000 ) ) ;
#32774 = ORIENTED_EDGE ( 'NONE', *, *, #35196, .T. ) ;
#32775 = CARTESIAN_POINT ( 'NONE',  ( 15.36283324375265025, 26.87922326031363340, -5.944726108962296252 ) ) ;
#32776 = EDGE_LOOP ( 'NONE', ( #32193, #17727, #11790, #11353 ) ) ;
#32777 = AXIS2_PLACEMENT_3D ( 'NONE', #22492, #31252, #3813 ) ;
#32778 = CARTESIAN_POINT ( 'NONE',  ( -15.55253742554085150, 26.04285000535905681, -6.417767331807119113 ) ) ;
#32779 = CARTESIAN_POINT ( 'NONE',  ( -30.23838254412105186, -12.22961151633805166, 19.99202127657104811 ) ) ;
#32780 = DIRECTION ( 'NONE',  ( 0.000000000000000000, 0.000000000000000000, 1.000000000000000000 ) ) ;
#32781 = CARTESIAN_POINT ( 'NONE',  ( 15.13424392241500804, 26.03117488544685187, -8.768685094158927384 ) ) ;
#32782 = ORIENTED_EDGE ( 'NONE', *, *, #10805, .T. ) ;
#32783 = CARTESIAN_POINT ( 'NONE',  ( 25.05307922697820189, -14.82438956320695667, -16.62383189019713825 ) ) ;
#32784 = ORIENTED_EDGE ( 'NONE', *, *, #22388, .T. ) ;
#32786 = DIRECTION ( 'NONE',  ( 1.000000000000000000, 0.000000000000000000, 0.000000000000000000 ) ) ;
#32785 = CARTESIAN_POINT ( 'NONE',  ( -14.53593441609714532, 27.81463984687436408, -8.695921198377391192 ) ) ;
#32787 = CARTESIAN_POINT ( 'NONE',  ( -16.45245987805732923, -25.93375551561933179, -10.08876688787445097 ) ) ;
#32788 = EDGE_CURVE ( 'NONE', #1089, #10807, #13944, .T. ) ;
#32789 = FACE_BOUND ( 'NONE', #34187, .T. ) ;
#32790 = ORIENTED_EDGE ( 'NONE', *, *, #10166, .T. ) ;
#32791 = CARTESIAN_POINT ( 'NONE',  ( -19.15932531068841982, -7.943154726143056621, -27.72915435580758015 ) ) ;
#32792 = CARTESIAN_POINT ( 'NONE',  ( -14.25497869358564706, -25.70370180133969384, -9.718373509854576042 ) ) ;
#32793 = LINE ( 'NONE', #23437, #29372 ) ;
#32794 = CARTESIAN_POINT ( 'NONE',  ( 13.97033939041524597, 17.09349275497558196, -21.93499464288763079 ) ) ;
#32795 = EDGE_LOOP ( 'NONE', ( #6578, #19247 ) ) ;
#32796 = CARTESIAN_POINT ( 'NONE',  ( 20.47381378144825703, 2.410701076763831718, -28.14891251935899774 ) ) ;
#32797 = EDGE_CURVE ( 'NONE', #15571, #31096, #14441, .T. ) ;
#32798 = CARTESIAN_POINT ( 'NONE',  ( -8.395951170269910335, 10.09331379572990350, 10.68306085400108607 ) ) ;
#32799 = CARTESIAN_POINT ( 'NONE',  ( -25.22779562677311560, -30.53001673900746837, 23.00000000000093792 ) ) ;
#32800 = ORIENTED_EDGE ( 'NONE', *, *, #14456, .F. ) ;
#32801 = CARTESIAN_POINT ( 'NONE',  ( -24.68539487710851787, 0.1722238459068671235, -18.41696137871380046 ) ) ;
#32802 = CIRCLE ( 'NONE', #31476, 1.000000000000000000 ) ;
#32803 = CARTESIAN_POINT ( 'NONE',  ( 28.26373143719677472, -0.5205252554743069471, -13.43917560083705887 ) ) ;
#32804 = CARTESIAN_POINT ( 'NONE',  ( 32.53782915839349954, -12.43926102483652940, 18.87996532025783125 ) ) ;
#32805 = ORIENTED_EDGE ( 'NONE', *, *, #26160, .F. ) ;
#32806 = CARTESIAN_POINT ( 'NONE',  ( -27.50575908014011972, 1.800164312645714082, -11.66087879572743446 ) ) ;
#32807 = CIRCLE ( 'NONE', #20474, 1.000000000000000888 ) ;
#32808 = CARTESIAN_POINT ( 'NONE',  ( 2.927345865710861972E-15, 22.57051819516765789, -30.00000000000001421 ) ) ;
#32809 = DIRECTION ( 'NONE',  ( 1.000000000000000000, 0.000000000000000000, 0.000000000000000000 ) ) ;
#32810 = AXIS2_PLACEMENT_3D ( 'NONE', #13503, #23658, #36055 ) ;
#32811 = CIRCLE ( 'NONE', #8785, 1.000000000000000000 ) ;
#32812 = DIRECTION ( 'NONE',  ( 0.000000000000000000, 0.000000000000000000, 1.000000000000000000 ) ) ;
#32813 = DIRECTION ( 'NONE',  ( -0.000000000000000000, -0.000000000000000000, -1.000000000000000000 ) ) ;
#32814 = CARTESIAN_POINT ( 'NONE',  ( 16.00000000000000000, 22.50000000000000711, 0.000000000000000000 ) ) ;
#32815 = DIRECTION ( 'NONE',  ( -0.7071067811865500152, 1.239037099348077946E-16, -0.7071067811865451302 ) ) ;
#32816 = ORIENTED_EDGE ( 'NONE', *, *, #21510, .F. ) ;
#32817 = CARTESIAN_POINT ( 'NONE',  ( -25.29540831655226185, 6.194354954019752668, -7.886033299896356930 ) ) ;
#32818 = FACE_OUTER_BOUND ( 'NONE', #20115, .T. ) ;
#32819 = CARTESIAN_POINT ( 'NONE',  ( 4.096822963000107620, 8.035697679810645866, 11.00000000000000000 ) ) ;
#32820 = CARTESIAN_POINT ( 'NONE',  ( 16.10474936713543315, -14.84555984040918553, -24.35669833423021302 ) ) ;
#32821 = EDGE_CURVE ( 'NONE', #3600, #28389, #24331, .T. ) ;
#32822 = DIRECTION ( 'NONE',  ( 0.000000000000000000, 0.000000000000000000, 1.000000000000000000 ) ) ;
#32823 = CARTESIAN_POINT ( 'NONE',  ( -14.46041492111391946, 20.47739500831029957, 10.99387789255785108 ) ) ;
#32824 = CARTESIAN_POINT ( 'NONE',  ( 14.94663361625261189, 26.63105489887620081, -8.746052331878477304 ) ) ;
#32825 = PRESENTATION_STYLE_ASSIGNMENT (( #22852 ) ) ;
#32826 = ORIENTED_EDGE ( 'NONE', *, *, #215, .F. ) ;
#32827 = CARTESIAN_POINT ( 'NONE',  ( -16.02262695881562848, 21.94564375748138474, -10.73340876258623844 ) ) ;
#32828 = CARTESIAN_POINT ( 'NONE',  ( 24.65531199400543372, -28.60128534115915500, 10.99999999999989697 ) ) ;
#32829 = CARTESIAN_POINT ( 'NONE',  ( 15.23784189583742865, -26.55597465737094609, -6.888200020279732882 ) ) ;
#32830 = CARTESIAN_POINT ( 'NONE',  ( 6.330070799514983193, 27.28854476845134513, 12.00000000000000000 ) ) ;
#32831 = CARTESIAN_POINT ( 'NONE',  ( 14.03714680842188756, 23.91771073391425517, -13.51393999334652207 ) ) ;
#32832 = VERTEX_POINT ( 'NONE', #974 ) ;
#32833 = CARTESIAN_POINT ( 'NONE',  ( -7.953812613386786801, 14.77701242934787906, 12.00000000000000000 ) ) ;
#32834 = ORIENTED_EDGE ( 'NONE', *, *, #25728, .T. ) ;
#32835 = VECTOR ( 'NONE', #22402, 1000.000000000000000 ) ;
#32837 = DIRECTION ( 'NONE',  ( -1.000000000000000000, 0.000000000000000000, 0.000000000000000000 ) ) ;
#32836 = CARTESIAN_POINT ( 'NONE',  ( -12.56505670423899446, 21.18481041280805144, -18.43279161028919333 ) ) ;
#32838 = CARTESIAN_POINT ( 'NONE',  ( -11.92035180994863097, -21.48388645554785725, -18.45049858032665924 ) ) ;
#32839 = CARTESIAN_POINT ( 'NONE',  ( -29.92393930196035257, -26.04303208588109086, 11.00000000000017941 ) ) ;
#32840 = AXIS2_PLACEMENT_3D ( 'NONE', #14169, #1180, #13563 ) ;
#32841 = CONICAL_SURFACE ( 'NONE', #36079, 0.9999999999999986677, 0.7853981633974503884 ) ;
#32842 = CARTESIAN_POINT ( 'NONE',  ( -32.28394191823594639, -20.85172211888466620, -5.000000000000000888 ) ) ;
#32843 = CARTESIAN_POINT ( 'NONE',  ( -6.188423164013283184, -19.73497389761912046, -27.63864133075322016 ) ) ;
#32844 = CARTESIAN_POINT ( 'NONE',  ( 12.01968976909422260, 17.96829324440782827, -23.93304672575846581 ) ) ;
#32845 = EDGE_LOOP ( 'NONE', ( #5608, #25526, #38845, #22531 ) ) ;
#32846 = CARTESIAN_POINT ( 'NONE',  ( 19.85109443489771408, 8.256135034430100106, -22.21491113497751613 ) ) ;
#32847 = VECTOR ( 'NONE', #12719, 1000.000000000000000 ) ;
#32848 = FACE_OUTER_BOUND ( 'NONE', #14037, .T. ) ;
#32849 = DIRECTION ( 'NONE',  ( 0.7431448254773846962, -0.6691306063588690067, 0.000000000000000000 ) ) ;
#32850 = DIRECTION ( 'NONE',  ( -0.9945218953682730678, 0.1045284632676569819, -0.000000000000000000 ) ) ;
#32851 = ORIENTED_EDGE ( 'NONE', *, *, #87, .T. ) ;
#32852 = CARTESIAN_POINT ( 'NONE',  ( -31.51724108361762688, -1.592384348128919935, -8.686465100392110728 ) ) ;
#32853 = CARTESIAN_POINT ( 'NONE',  ( -13.48130249190472796, 27.93180293473203690, 11.00000000000000000 ) ) ;
#32854 = CARTESIAN_POINT ( 'NONE',  ( 24.49951449059906139, -14.14480128616252053, 20.99999999999999645 ) ) ;
#32855 = CARTESIAN_POINT ( 'NONE',  ( -4.984135866956331817, 36.15314577889358105, 10.50000000000000533 ) ) ;
#32856 = ADVANCED_FACE ( 'NONE', ( #34304 ), #6850, .T. ) ;
#32857 = CARTESIAN_POINT ( 'NONE',  ( 33.54263992596453647, -17.18436309121399574, -7.973046152344251070 ) ) ;
#32858 = CARTESIAN_POINT ( 'NONE',  ( 29.92393930195800422, -26.04303208588348184, 11.00000000000002487 ) ) ;
#32859 = ORIENTED_EDGE ( 'NONE', *, *, #8529, .T. ) ;
#32860 = CARTESIAN_POINT ( 'NONE',  ( -7.577547685840081648, 11.84256962714647798, 13.00000000000000178 ) ) ;
#32861 = VECTOR ( 'NONE', #20440, 1000.000000000000000 ) ;
#32862 = CARTESIAN_POINT ( 'NONE',  ( 2.871201846650637268, 31.30332840660451765, 12.00000000000000000 ) ) ;
#32863 = ORIENTED_EDGE ( 'NONE', *, *, #22386, .T. ) ;
#32864 = CARTESIAN_POINT ( 'NONE',  ( 0.8942644845752143468, 22.01017621520333378, -24.22054542436852742 ) ) ;
#32865 = DIRECTION ( 'NONE',  ( 0.000000000000000000, 0.000000000000000000, 1.000000000000000000 ) ) ;
#32866 = AXIS2_PLACEMENT_3D ( 'NONE', #21231, #12086, #34028 ) ;
#32867 = EDGE_CURVE ( 'NONE', #21421, #27921, #4216, .T. ) ;
#32868 = CARTESIAN_POINT ( 'NONE',  ( 14.85579657860257541, 20.34187940403349870, 10.49999999999999822 ) ) ;
#32869 = CARTESIAN_POINT ( 'NONE',  ( -14.09933648065464240, 26.02968990214173317, 11.00000000000000000 ) ) ;
#32871 = CARTESIAN_POINT ( 'NONE',  ( 6.082600654608392610, 21.41965916404854298, 13.00000000000000178 ) ) ;
#32870 = PRODUCT_DEFINITION ( 'UNKNOWN', '', #28811, #18340 ) ;
#32872 = DIRECTION ( 'NONE',  ( -0.5720614028176888022, -0.4156269377774527984, -0.7071067811865442421 ) ) ;
#32873 = CARTESIAN_POINT ( 'NONE',  ( 13.45995091351214690, 25.18522299110997764, -13.40001028691244400 ) ) ;
#32874 = LINE ( 'NONE', #38552, #4277 ) ;
#32875 = ORIENTED_EDGE ( 'NONE', *, *, #6469, .T. ) ;
#32877 = PLANE ( 'NONE',  #8375 ) ;
#32876 = CARTESIAN_POINT ( 'NONE',  ( -18.48907582165858798, 14.46313849928662165, -14.89271776214601140 ) ) ;
#32878 = EDGE_CURVE ( 'NONE', #2749, #3856, #37320, .T. ) ;
#32879 = CARTESIAN_POINT ( 'NONE',  ( -0.9938779058054629800, 37.09261900150649893, 10.49999999999999822 ) ) ;
#32880 = CARTESIAN_POINT ( 'NONE',  ( 14.77006329367439896, -25.65908439595070334, -10.17951868138070992 ) ) ;
#32881 = EDGE_CURVE ( 'NONE', #28480, #3881, #38591, .T. ) ;
#32882 = CARTESIAN_POINT ( 'NONE',  ( 2.036571916123615100, 8.108948098542045457, 7.499999999999990230 ) ) ;
#32883 = CARTESIAN_POINT ( 'NONE',  ( 15.40660648310854164, 26.81700542816128063, -5.474045217557533149 ) ) ;
#32884 = CARTESIAN_POINT ( 'NONE',  ( 17.34253826539385201, 27.32041144647958575, -5.000000000000000000 ) ) ;
#32885 = CYLINDRICAL_SURFACE ( 'NONE', #39517, 0.5000000000000000000 ) ;
#32886 = CARTESIAN_POINT ( 'NONE',  ( -19.16391196221957571, -17.99803450724484222, -18.76479932701361975 ) ) ;
#32887 = CARTESIAN_POINT ( 'NONE',  ( 1.817969461173305490, -24.76413945269762351, -5.483170422348042194 ) ) ;
#32888 = CARTESIAN_POINT ( 'NONE',  ( 14.87733101683222614, 24.99273381504638891, -10.66221022678619867 ) ) ;
#32889 = CARTESIAN_POINT ( 'NONE',  ( 19.10285424782163233, 12.84828869033409049, -15.93831158563282102 ) ) ;
#32890 = DIRECTION ( 'NONE',  ( 0.000000000000000000, 0.000000000000000000, 1.000000000000000000 ) ) ;
#32891 = EDGE_LOOP ( 'NONE', ( #30705, #9906, #29921, #25323 ) ) ;
#32892 = CARTESIAN_POINT ( 'NONE',  ( -5.072650811858919973, 29.32414667381679863, -15.74330015237563529 ) ) ;
#32893 = ORIENTED_EDGE ( 'NONE', *, *, #33108, .F. ) ;
#32894 = B_SPLINE_CURVE_WITH_KNOTS ( 'NONE', 3,
 ( #14744, #2157, #13782, #27133, #29227, #10539, #5396, #29025, #26174, #33247, #23883, #36479, #18002, #4443, #16845, #21040, #8647, #33449 ),
 .UNSPECIFIED., .F., .F.,
 ( 4, 2, 2, 2, 2, 2, 2, 2, 4 ),
 ( 0.000000000000000000, 0.1249999999999999167, 0.2499999999999998335, 0.3749999999999997780, 0.4999999999999996669, 0.6249999999999995559, 0.7499999999999995559, 0.8749999999999997780, 1.000000000000000000 ),
 .UNSPECIFIED. ) ;
#32895 = CIRCLE ( 'NONE', #6934, 0.5000000000000004441 ) ;
#32896 = CIRCLE ( 'NONE', #34190, 0.5000000000000007772 ) ;
#32897 = FACE_OUTER_BOUND ( 'NONE', #20800, .T. ) ;
#32898 = ORIENTED_EDGE ( 'NONE', *, *, #26789, .F. ) ;
#32899 = DIRECTION ( 'NONE',  ( 0.000000000000000000, 0.000000000000000000, -1.000000000000000000 ) ) ;
#32900 = ADVANCED_FACE ( 'NONE', ( #11122 ), #16821, .T. ) ;
#32901 = FACE_OUTER_BOUND ( 'NONE', #11761, .T. ) ;
#32902 = EDGE_CURVE ( 'NONE', #16528, #15223, #38748, .T. ) ;
#32903 = EDGE_LOOP ( 'NONE', ( #18348, #37196, #10683, #20405, #27739 ) ) ;
#32904 = CARTESIAN_POINT ( 'NONE',  ( -28.54007740871540122, 0.5227748155925792117, -11.61433878387980378 ) ) ;
#32905 = ORIENTED_EDGE ( 'NONE', *, *, #20961, .T. ) ;
#32906 = CARTESIAN_POINT ( 'NONE',  ( 20.95614885317017695, -6.336004544166005559, -24.36784054283095458 ) ) ;
#32907 = EDGE_LOOP ( 'NONE', ( #21733, #23060 ) ) ;
#32908 = CARTESIAN_POINT ( 'NONE',  ( -0.4999999999999998890, 37.50000000000000711, 10.49999999999999822 ) ) ;
#32909 = VERTEX_POINT ( 'NONE', #32047 ) ;
#32910 = CARTESIAN_POINT ( 'NONE',  ( 15.00309677617812376, 1.567672476142360383, 21.00000000000000000 ) ) ;
#32911 = LINE ( 'NONE', #33517, #22794 ) ;
#32912 = DIRECTION ( 'NONE',  ( -0.6691306063588570163, 0.7431448254773953543, -0.000000000000000000 ) ) ;
#32913 = VERTEX_POINT ( 'NONE', #38545 ) ;
#32914 = LINE ( 'NONE', #26603, #7440 ) ;
#32915 = CARTESIAN_POINT ( 'NONE',  ( -2.579909280894606916, 7.957613945008774614, 10.94611345180490325 ) ) ;
#32916 = CARTESIAN_POINT ( 'NONE',  ( -2.590592964390336927, 26.81117624614021011, 23.00000000000000000 ) ) ;
#32917 = EDGE_CURVE ( 'NONE', #3398, #8093, #22366, .T. ) ;
#32918 = CARTESIAN_POINT ( 'NONE',  ( 15.32941689225309112, 13.72693657690245672, -28.26505645429302405 ) ) ;
#32919 = CIRCLE ( 'NONE', #3063, 0.5000000000000004441 ) ;
#32920 = CARTESIAN_POINT ( 'NONE',  ( 12.35192597829481009, 32.37184802151152496, -6.781871780508718750 ) ) ;
#32921 = AXIS2_PLACEMENT_3D ( 'NONE', #28176, #3789, #40168 ) ;
#32922 = ORIENTED_EDGE ( 'NONE', *, *, #3758, .F. ) ;
#32923 = DIRECTION ( 'NONE',  ( 0.000000000000000000, 0.000000000000000000, 1.000000000000000000 ) ) ;
#32924 = CARTESIAN_POINT ( 'NONE',  ( -2.036571916123810055, 8.108948098542073879, 11.00000000000000000 ) ) ;
#32925 = CARTESIAN_POINT ( 'NONE',  ( 15.10869851544610931, -25.55731746936413629, -10.62300024995772318 ) ) ;
#32926 = CARTESIAN_POINT ( 'NONE',  ( 16.60464863832688565, -22.41657912773190375, 19.66345542862528362 ) ) ;
#32927 = AXIS2_PLACEMENT_3D ( 'NONE', #30646, #6048, #34089 ) ;
#32928 = DIRECTION ( 'NONE',  ( -0.000000000000000000, -0.000000000000000000, -1.000000000000000000 ) ) ;
#32929 = AXIS2_PLACEMENT_3D ( 'NONE', #27358, #11527, #8677 ) ;
#32930 = CARTESIAN_POINT ( 'NONE',  ( -14.02126489188123060, 23.95563206446321303, -13.51135549859506746 ) ) ;
#32931 = CARTESIAN_POINT ( 'NONE',  ( -35.93605200993580695, -16.45551934610077538, 14.53008259254024459 ) ) ;
#32932 = CARTESIAN_POINT ( 'NONE',  ( 10.32640477728945072, -21.13211831446180611, -19.62180369577067296 ) ) ;
#32933 = LINE ( 'NONE', #16891, #4957 ) ;
#32934 = VERTEX_POINT ( 'NONE', #10928 ) ;
#32935 = EDGE_LOOP ( 'NONE', ( #12421, #10339, #21496, #18448 ) ) ;
#32936 = CARTESIAN_POINT ( 'NONE',  ( -12.37123995031714863, 31.49198740136808539, -8.565043564655828945 ) ) ;
#32937 = DIRECTION ( 'NONE',  ( 0.000000000000000000, 0.000000000000000000, -1.000000000000000000 ) ) ;
#32938 = CARTESIAN_POINT ( 'NONE',  ( 6.576253646258387597, 14.29921418520925513, 11.00000000000000000 ) ) ;
#32939 = CARTESIAN_POINT ( 'NONE',  ( -20.77014107886579808, -3.131800453615022573, -26.53419280964595117 ) ) ;
#32940 = DIRECTION ( 'NONE',  ( -0.000000000000000000, -0.000000000000000000, -1.000000000000000000 ) ) ;
#32941 = ORIENTED_EDGE ( 'NONE', *, *, #11789, .F. ) ;
#32942 = CARTESIAN_POINT ( 'NONE',  ( 23.91506835619285809, 0.5469039752616722261, -19.50346979283914450 ) ) ;
#32943 = CYLINDRICAL_SURFACE ( 'NONE', #5711, 0.5000000000000000000 ) ;
#32944 = DIRECTION ( 'NONE',  ( 1.000000000000000000, 0.000000000000000000, 0.000000000000000000 ) ) ;
#32945 = CARTESIAN_POINT ( 'NONE',  ( -21.78011286655814871, -29.15515566786809032, 10.99999999999984546 ) ) ;
#32946 = EDGE_CURVE ( 'NONE', #18096, #22349, #32665, .T. ) ;
#32947 = ORIENTED_EDGE ( 'NONE', *, *, #16236, .T. ) ;
#32948 = CARTESIAN_POINT ( 'NONE',  ( -20.48147506303724441, 0.8713082578521275101, -29.34858951695225571 ) ) ;
#32949 = CARTESIAN_POINT ( 'NONE',  ( 3.211395437248501850, 12.61633075744433796, 13.00000000000000178 ) ) ;
#32951 = ADVANCED_FACE ( 'NONE', ( #4822 ), #17431, .F. ) ;
#32950 = ORIENTED_EDGE ( 'NONE', *, *, #4020, .T. ) ;
#32952 = CARTESIAN_POINT ( 'NONE',  ( 33.38598080700936066, -4.103730722464701053, -7.695482771259642973 ) ) ;
#32953 = CIRCLE ( 'NONE', #5038, 15.00000000000000000 ) ;
#32954 = CIRCLE ( 'NONE', #6328, 0.5000000000000004441 ) ;
#32955 = CARTESIAN_POINT ( 'NONE',  ( 30.37673449013164984, -23.61083502489066177, 15.72805884748940386 ) ) ;
#32956 = ORIENTED_EDGE ( 'NONE', *, *, #26611, .T. ) ;
#32957 = CARTESIAN_POINT ( 'NONE',  ( -1.856244906471939737, 39.65430245495498696, 14.53008259254010959 ) ) ;
#32958 = AXIS2_PLACEMENT_3D ( 'NONE', #22043, #2966, #33855 ) ;
#32959 = CARTESIAN_POINT ( 'NONE',  ( -10.60610353951573259, -24.43405348875333871, 17.42190598798822521 ) ) ;
#32960 = CARTESIAN_POINT ( 'NONE',  ( -3.000488737322915878, 30.46850471150003159, 9.000000000000001776 ) ) ;
#32961 = CARTESIAN_POINT ( 'NONE',  ( -0.8947151973526094038, 30.76432767446198824, 20.69868183039781329 ) ) ;
#32962 = AXIS2_PLACEMENT_3D ( 'NONE', #29283, #9846, #12886 ) ;
#32963 = CARTESIAN_POINT ( 'NONE',  ( 4.003793318659404576, 8.455722206104576699, 10.49999999999999822 ) ) ;
#32964 = EDGE_LOOP ( 'NONE', ( #9800, #20976, #26392, #17273, #8794, #34366 ) ) ;
#32965 = DIRECTION ( 'NONE',  ( 1.000000000000000000, 0.000000000000000000, 0.000000000000000000 ) ) ;
#32966 = CARTESIAN_POINT ( 'NONE',  ( -11.39464589777670867, 26.66807349098043289, 6.000000000000000000 ) ) ;
#32967 = ADVANCED_FACE ( 'NONE', ( #32464 ), #32255, .F. ) ;
#32968 = CARTESIAN_POINT ( 'NONE',  ( 3.380733272816430546, 20.85284384237622746, -26.30940457203467275 ) ) ;
#32969 = DIRECTION ( 'NONE',  ( -0.000000000000000000, -0.000000000000000000, -1.000000000000000000 ) ) ;
#32970 = ADVANCED_FACE ( 'NONE', ( #13961 ), #16619, .F. ) ;
#32971 = CARTESIAN_POINT ( 'NONE',  ( 22.54917513123528394, -0.2132175735513469617, 20.25080042702448679 ) ) ;
#32972 = CARTESIAN_POINT ( 'NONE',  ( 19.71634060764898067, -27.14742637253563373, -6.361116528107567447 ) ) ;
#32973 = CARTESIAN_POINT ( 'NONE',  ( -2.806807826039844578, 9.295007390093649846, 7.000000000000000000 ) ) ;
#32974 = VECTOR ( 'NONE', #1238, 1000.000000000000114 ) ;
#32975 = DIRECTION ( 'NONE',  ( 1.000000000000000000, 0.000000000000000000, 0.000000000000000000 ) ) ;
#32976 = CARTESIAN_POINT ( 'NONE',  ( 2.109203785269305964, 7.931710454523196674, 10.49999999999999822 ) ) ;
#32977 = EDGE_LOOP ( 'NONE', ( #38832, #15725, #30837, #15459, #25487 ) ) ;
#32978 = CARTESIAN_POINT ( 'NONE',  ( 14.98081254870050039, 26.09019376164257409, -9.232264583633339683 ) ) ;
#32979 = AXIS2_PLACEMENT_3D ( 'NONE', #19852, #28184, #361 ) ;
#32980 = ORIENTED_EDGE ( 'NONE', *, *, #19282, .T. ) ;
#32982 = AXIS2_PLACEMENT_3D ( 'NONE', #35833, #29535, #17956 ) ;
#32981 = CARTESIAN_POINT ( 'NONE',  ( -12.66284596178592459, 20.13327502018258031, -19.54334862798365080 ) ) ;
#32983 = EDGE_CURVE ( 'NONE', #22904, #1365, #15378, .T. ) ;
#32984 = CARTESIAN_POINT ( 'NONE',  ( -23.01245512501514057, -23.08877437847487002, 19.27171037444190205 ) ) ;
#32985 = CARTESIAN_POINT ( 'NONE',  ( -14.14332487906608549, 26.04398259919136294, 10.49999999999999822 ) ) ;
#32986 = CARTESIAN_POINT ( 'NONE',  ( 14.79573094385063037, 25.22704658224830254, -10.65696934714573985 ) ) ;
#32987 = VERTEX_POINT ( 'NONE', #14368 ) ;
#32988 = CARTESIAN_POINT ( 'NONE',  ( 31.85050647178360705, -20.18765053876312265, -7.972301957832756969 ) ) ;
#32989 = EDGE_LOOP ( 'NONE', ( #18547, #3682, #15803, #32816 ) ) ;
#32990 = AXIS2_PLACEMENT_3D ( 'NONE', #33214, #11465, #24053 ) ;
#32992 = CYLINDRICAL_SURFACE ( 'NONE', #19241, 0.5000000000000004441 ) ;
#32991 = CARTESIAN_POINT ( 'NONE',  ( -14.79259077307489889, 26.65558470197620267, -9.204917952329308761 ) ) ;
#32993 = CARTESIAN_POINT ( 'NONE',  ( -18.29333439512888759, -27.14906503354761824, -6.376644952967080116 ) ) ;
#32994 = FACE_OUTER_BOUND ( 'NONE', #29410, .T. ) ;
#32995 = AXIS2_PLACEMENT_3D ( 'NONE', #17053, #25576, #29235 ) ;
#32996 = ORIENTED_EDGE ( 'NONE', *, *, #35228, .T. ) ;
#32997 = CARTESIAN_POINT ( 'NONE',  ( -29.92619010456159856, -11.28214714606756175, -13.85028604681554754 ) ) ;
#32998 = CARTESIAN_POINT ( 'NONE',  ( -14.15683454941679464, -25.37115389201304438, -10.66325925726328272 ) ) ;
#32999 = CARTESIAN_POINT ( 'NONE',  ( 21.91981567634952199, -15.65087685632054004, 23.00000000000000000 ) ) ;
#33000 = EDGE_LOOP ( 'NONE', ( #4126, #30621 ) ) ;
#33001 = CARTESIAN_POINT ( 'NONE',  ( 29.14407284010881227, 1.139970232528481953, -8.782330516724952574 ) ) ;
#33002 = CARTESIAN_POINT ( 'NONE',  ( -12.68475447279705470, 27.14725768220950641, 9.500000000000000000 ) ) ;
#33003 = CYLINDRICAL_SURFACE ( 'NONE', #19296, 1.000000000000000000 ) ;
#33004 = EDGE_CURVE ( 'NONE', #18451, #32281, #6790, .T. ) ;
#33005 = ORIENTED_EDGE ( 'NONE', *, *, #16612, .T. ) ;
#33006 = EDGE_CURVE ( 'NONE', #31948, #7370, #12004, .T. ) ;
#33007 = CARTESIAN_POINT ( 'NONE',  ( -24.60177868520493050, 0.3453315261475468634, -18.44044427177923851 ) ) ;
#33008 = EDGE_CURVE ( 'NONE', #38994, #17440, #10512, .T. ) ;
#33009 = CARTESIAN_POINT ( 'NONE',  ( 20.63866867332527022, 0.2073280320569168000, -28.04521516201818443 ) ) ;
#33010 = CARTESIAN_POINT ( 'NONE',  ( 29.95833833019052150, -4.698917079249050666, 19.27171037444192692 ) ) ;
#33011 = ORIENTED_EDGE ( 'NONE', *, *, #29898, .T. ) ;
#33012 = CARTESIAN_POINT ( 'NONE',  ( -27.90312125966312351, 1.785194626332250234, -10.70166145795786150 ) ) ;
#33013 = CARTESIAN_POINT ( 'NONE',  ( -11.31392148919591811, 36.91540483778867099, -5.000000000000009770 ) ) ;
#33014 = DIRECTION ( 'NONE',  ( 1.000000000000000000, 0.000000000000000000, 0.000000000000000000 ) ) ;
#33015 = CIRCLE ( 'NONE', #9661, 16.99999999999999645 ) ;
#33016 = CARTESIAN_POINT ( 'NONE',  ( -16.23042486173916288, -23.86708630543299847, 18.87996532025784191 ) ) ;
#33017 = VECTOR ( 'NONE', #14103, 1000.000000000000000 ) ;
#33018 = EDGE_CURVE ( 'NONE', #19729, #25837, #39884, .T. ) ;
#33019 = AXIS2_PLACEMENT_3D ( 'NONE', #15792, #27983, #9103 ) ;
#33020 = FACE_OUTER_BOUND ( 'NONE', #24799, .T. ) ;
#33021 = LINE ( 'NONE', #30158, #2850 ) ;
#33022 = EDGE_CURVE ( 'NONE', #21064, #16758, #7456, .T. ) ;
#33023 = LINE ( 'NONE', #27106, #11424 ) ;
#33024 = ORIENTED_EDGE ( 'NONE', *, *, #7352, .F. ) ;
#33025 = CARTESIAN_POINT ( 'NONE',  ( -22.35010935049834657, 5.092895750971690561, -18.86795456680612304 ) ) ;
#33026 = CARTESIAN_POINT ( 'NONE',  ( 8.917734535019441466, 14.47043272369397116, 13.00000000000000178 ) ) ;
#33027 = CARTESIAN_POINT ( 'NONE',  ( -33.75875814100324845, 2.759858869446484064, 23.00000000000000000 ) ) ;
#33028 = CARTESIAN_POINT ( 'NONE',  ( 15.24051681827566718, -14.92785667918263925, -25.72502823181857323 ) ) ;
#33029 = DIRECTION ( 'NONE',  ( -0.000000000000000000, -0.000000000000000000, -1.000000000000000000 ) ) ;
#33030 = DIRECTION ( 'NONE',  ( 0.000000000000000000, 0.000000000000000000, 1.000000000000000000 ) ) ;
#33031 = CARTESIAN_POINT ( 'NONE',  ( 15.28661535835308349, 27.13569895802415388, -5.942075632022802090 ) ) ;
#33032 = CARTESIAN_POINT ( 'NONE',  ( 5.055868909836068070, -26.71495157282352650, 12.14047268033097460 ) ) ;
#33033 = EDGE_LOOP ( 'NONE', ( #36375, #13002, #40181, #30049 ) ) ;
#33034 = CARTESIAN_POINT ( 'NONE',  ( -16.73766650064135320, 21.43861104905754189, -8.822088556755165456 ) ) ;
#33035 = CARTESIAN_POINT ( 'NONE',  ( -26.61692196988933645, -13.50708991729978514, 20.82122704794079482 ) ) ;
#33036 = LINE ( 'NONE', #5185, #39285 ) ;
#33037 = CARTESIAN_POINT ( 'NONE',  ( 12.66086287625040541, 21.04242839094937167, -18.45356328166587900 ) ) ;
#33038 = VERTEX_POINT ( 'NONE', #39741 ) ;
#33039 = CARTESIAN_POINT ( 'NONE',  ( -14.86131180699622334, 21.44076732726277967, 10.82238861112337247 ) ) ;
#33040 = ORIENTED_EDGE ( 'NONE', *, *, #24968, .T. ) ;
#33042 = LINE ( 'NONE', #36076, #32211 ) ;
#33041 = CARTESIAN_POINT ( 'NONE',  ( -12.03858661653558748, 20.03409609272645397, -20.52224590143303828 ) ) ;
#33043 = CARTESIAN_POINT ( 'NONE',  ( -15.41099496508465982, -26.52696749137851384, -7.355554215977166521 ) ) ;
#33044 = CARTESIAN_POINT ( 'NONE',  ( -18.84564290660914310, -29.34375446593495695, 11.55979286843968801 ) ) ;
#33045 = CIRCLE ( 'NONE', #10963, 62.00000000000014211 ) ;
#33046 = AXIS2_PLACEMENT_3D ( 'NONE', #19018, #21467, #28159 ) ;
#33047 = CARTESIAN_POINT ( 'NONE',  ( -33.23797450146873445, -18.71509596241817164, -7.116742953870333288 ) ) ;
#33048 = CARTESIAN_POINT ( 'NONE',  ( -6.760112097234737050, -24.51974927990703179, -10.32779609532193454 ) ) ;
#33049 = CARTESIAN_POINT ( 'NONE',  ( 4.984135866956514782, 36.15314577889351000, 10.49999999999999822 ) ) ;
#33050 = CARTESIAN_POINT ( 'NONE',  ( 11.67910349775616652, 17.21656688193314366, -26.88047951749153341 ) ) ;
#33051 = ORIENTED_EDGE ( 'NONE', *, *, #22309, .T. ) ;
#33052 = CARTESIAN_POINT ( 'NONE',  ( 25.32158894843077945, 6.480252874148680675, -5.478621571544178614 ) ) ;
#33053 = CARTESIAN_POINT ( 'NONE',  ( -17.34253826607186966, 27.32041144404027122, 0.000000000000000000 ) ) ;
#33054 = DIRECTION ( 'NONE',  ( -0.2876062384759514590, -0.6459741880212531706, -0.7071067811865452413 ) ) ;
#33055 = CARTESIAN_POINT ( 'NONE',  ( 0.000000000000000000, 22.50000000000000355, 7.000000000000000000 ) ) ;
#33056 = AXIS2_PLACEMENT_3D ( 'NONE', #4718, #28894, #1271 ) ;
#33057 = ORIENTED_EDGE ( 'NONE', *, *, #25674, .F. ) ;
#33058 = CARTESIAN_POINT ( 'NONE',  ( -30.86022713980213794, -1.524650393404385129, -10.07426524678920821 ) ) ;
#33059 = CARTESIAN_POINT ( 'NONE',  ( 29.65047528457347426, -0.01023675481382509654, -10.17575680121469262 ) ) ;
#33060 = FACE_OUTER_BOUND ( 'NONE', #37081, .T. ) ;
#33061 = CARTESIAN_POINT ( 'NONE',  ( 18.52756972024298676, -17.82802275548051796, 20.94377226548369819 ) ) ;
#33062 = CYLINDRICAL_SURFACE ( 'NONE', #35578, 5.999999999999996447 ) ;
#33063 = CARTESIAN_POINT ( 'NONE',  ( 0.3762615568374529929, 19.56555719779890978, 13.00000000000000178 ) ) ;
#33064 = FACE_OUTER_BOUND ( 'NONE', #13022, .T. ) ;
#33065 = EDGE_LOOP ( 'NONE', ( #27205, #2860, #11992 ) ) ;
#33066 = FACE_OUTER_BOUND ( 'NONE', #17485, .T. ) ;
#33067 = AXIS2_PLACEMENT_3D ( 'NONE', #21019, #17787, #11278 ) ;
#33068 = DIRECTION ( 'NONE',  ( 1.000000000000000000, 0.000000000000000000, 0.000000000000000000 ) ) ;
#33069 = ORIENTED_EDGE ( 'NONE', *, *, #4143, .F. ) ;
#33070 = CARTESIAN_POINT ( 'NONE',  ( 0.3375428170692008623, 31.33837579149849262, -14.73082907740201009 ) ) ;
#33071 = CARTESIAN_POINT ( 'NONE',  ( -5.440908595777636414, 35.94977745735568675, 7.500000000000000888 ) ) ;
#33072 = CARTESIAN_POINT ( 'NONE',  ( -13.03339520833720222, 15.55251603720152431, 10.94611345180490680 ) ) ;
#33073 = CARTESIAN_POINT ( 'NONE',  ( 5.082600654608392610, 21.41965916404854298, 12.00000000000000000 ) ) ;
#33074 = AXIS2_PLACEMENT_3D ( 'NONE', #424, #620, #12406 ) ;
#33075 = CARTESIAN_POINT ( 'NONE',  ( -12.05736835487443237, 14.38397459621567442, 9.500000000000000000 ) ) ;
#33076 = LINE ( 'NONE', #36314, #37270 ) ;
#33077 = CARTESIAN_POINT ( 'NONE',  ( 13.48130249190479191, 27.93180293473185927, 10.50000000000000533 ) ) ;
#33078 = CARTESIAN_POINT ( 'NONE',  ( 14.90467518106525269, 28.31725849260483585, -5.467169310882759703 ) ) ;
#33079 = DIRECTION ( 'NONE',  ( -0.2876062384759508483, -0.6459741880212497289, -0.7071067811865486830 ) ) ;
#33080 = ORIENTED_EDGE ( 'NONE', *, *, #3348, .F. ) ;
#33082 = DIRECTION ( 'NONE',  ( 0.000000000000000000, 0.000000000000000000, 1.000000000000000000 ) ) ;
#33081 = CARTESIAN_POINT ( 'NONE',  ( -19.04904607429094554, 15.01394467124153564, -11.86198345635079932 ) ) ;
#33083 = CARTESIAN_POINT ( 'NONE',  ( -14.02836544648977579, 27.77630492435593013, 10.49999999999999822 ) ) ;
#33084 = CARTESIAN_POINT ( 'NONE',  ( 13.73281793707762155, -24.12020055917744799, -13.51159965186342404 ) ) ;
#33085 = CARTESIAN_POINT ( 'NONE',  ( -3.503793317224517700, 8.420815634768727520, 7.000000000000000000 ) ) ;
#33086 = CARTESIAN_POINT ( 'NONE',  ( 10.95987886464238059, 17.32429135621979555, -30.00000000000000355 ) ) ;
#33087 = DIRECTION ( 'NONE',  ( -0.2079116908177663092, -0.9781476007338041345, 0.000000000000000000 ) ) ;
#33088 = DIRECTION ( 'NONE',  ( 0.000000000000000000, 0.000000000000000000, 1.000000000000000000 ) ) ;
#33089 = CARTESIAN_POINT ( 'NONE',  ( -17.11419722955264433, -16.05889537474196516, -22.00308921696831632 ) ) ;
#33090 = CARTESIAN_POINT ( 'NONE',  ( 1.732327452010537616, -24.13709212142373062, -10.88692373186505336 ) ) ;
#33091 = CARTESIAN_POINT ( 'NONE',  ( 13.62424208523637859, 22.55708696713261929, -15.46943763161296559 ) ) ;
#33092 = CARTESIAN_POINT ( 'NONE',  ( 18.69607909436101423, 11.44394688062264009, -20.12350778403434504 ) ) ;
#33093 = CARTESIAN_POINT ( 'NONE',  ( -9.771904059883794957, 33.31711103041964606, 7.000000000000000000 ) ) ;
#33094 = ORIENTED_EDGE ( 'NONE', *, *, #17972, .F. ) ;
#33095 = CARTESIAN_POINT ( 'NONE',  ( -5.707447616493412923, 27.97779256337231146, -16.72301236455337303 ) ) ;
#33096 = VERTEX_POINT ( 'NONE', #27753 ) ;
#33097 = VECTOR ( 'NONE', #78, 1000.000000000000000 ) ;
#33098 = DIRECTION ( 'NONE',  ( -0.000000000000000000, -0.000000000000000000, -1.000000000000000000 ) ) ;
#33099 = ORIENTED_EDGE ( 'NONE', *, *, #27945, .F. ) ;
#33100 = LINE ( 'NONE', #27190, #28443 ) ;
#33101 = EDGE_CURVE ( 'NONE', #26001, #27435, #11524, .T. ) ;
#33102 = CARTESIAN_POINT ( 'NONE',  ( 9.428145666828122273, 11.00786382055638768, 10.49999999999999822 ) ) ;
#33103 = AXIS2_PLACEMENT_3D ( 'NONE', #38339, #16616, #7662 ) ;
#33104 = ORIENTED_EDGE ( 'NONE', *, *, #6313, .T. ) ;
#33105 = CARTESIAN_POINT ( 'NONE',  ( -20.95165138070167998, 0.9770979443023026789, -26.23948052383034479 ) ) ;
#33106 = ORIENTED_EDGE ( 'NONE', *, *, #32983, .F. ) ;
#33107 = CARTESIAN_POINT ( 'NONE',  ( 34.27195656595002760, -11.45219146868936910, -8.887004270612056445 ) ) ;
#33108 = EDGE_CURVE ( 'NONE', #33983, #24685, #14964, .T. ) ;
#33109 = VERTEX_POINT ( 'NONE', #17831 ) ;
#33110 = CARTESIAN_POINT ( 'NONE',  ( 13.74617375768325900, 27.96120515612769708, 10.49999999999999822 ) ) ;
#33111 = ORIENTED_EDGE ( 'NONE', *, *, #6896, .T. ) ;
#33112 = EDGE_CURVE ( 'NONE', #29442, #7636, #5614, .T. ) ;
#33113 = DIRECTION ( 'NONE',  ( 1.000000000000000000, 0.000000000000000000, 0.000000000000000000 ) ) ;
#33114 = CARTESIAN_POINT ( 'NONE',  ( 6.354454053420414361, 35.54304081427980577, 11.00000000000000000 ) ) ;
#33115 = DIRECTION ( 'NONE',  ( -0.000000000000000000, -0.000000000000000000, 1.000000000000000000 ) ) ;
#33116 = ORIENTED_EDGE ( 'NONE', *, *, #1577, .T. ) ;
#33117 = FACE_OUTER_BOUND ( 'NONE', #13721, .T. ) ;
#33118 = CARTESIAN_POINT ( 'NONE',  ( -7.064571727552472424, 31.45661825943146894, 13.00000000000000178 ) ) ;
#33119 = CARTESIAN_POINT ( 'NONE',  ( 4.671113270415285790, 24.36520164658795551, 23.00000000000000000 ) ) ;
#33120 = CARTESIAN_POINT ( 'NONE',  ( 14.89366125532731822, 14.36502201557359193, -27.10073944775506760 ) ) ;
#33121 = CARTESIAN_POINT ( 'NONE',  ( 11.88982892552273007, 30.98811914902011111, -9.910042724562915240 ) ) ;
#33122 = ORIENTED_EDGE ( 'NONE', *, *, #25537, .F. ) ;
#33123 = CARTESIAN_POINT ( 'NONE',  ( -19.59276562800022248, 8.779838875553902966, -22.22895676643048191 ) ) ;
#33124 = CARTESIAN_POINT ( 'NONE',  ( 10.44103466624280507, 32.57396620494213124, 11.00000000000000000 ) ) ;
#33125 = DIRECTION ( 'NONE',  ( -0.000000000000000000, -0.000000000000000000, -1.000000000000000000 ) ) ;
#33126 = ADVANCED_FACE ( 'NONE', ( #18025 ), #27354, .T. ) ;
#33127 = EDGE_CURVE ( 'NONE', #20195, #36614, #20674, .T. ) ;
#33128 = CARTESIAN_POINT ( 'NONE',  ( 10.70129962474131879, -19.52760334584666069, -22.71333977806620297 ) ) ;
#33129 = CARTESIAN_POINT ( 'NONE',  ( -7.917741276437941345, 30.52956727630665057, 12.00000000000000000 ) ) ;
#33130 = VECTOR ( 'NONE', #5169, 1000.000000000000000 ) ;
#33131 = LINE ( 'NONE', #14832, #19861 ) ;
#33132 = CARTESIAN_POINT ( 'NONE',  ( -13.48068414432812645, 22.83747268959859511, -15.44824800343550919 ) ) ;
#33133 = CARTESIAN_POINT ( 'NONE',  ( -35.73275206861759301, -5.440967016230455755, 14.53008259254057499 ) ) ;
#33134 = CARTESIAN_POINT ( 'NONE',  ( 11.05990709802074257, -21.55257169122715410, -18.53364441852212252 ) ) ;
#33135 = CARTESIAN_POINT ( 'NONE',  ( -9.381156159426771168, 10.79514327830607101, 7.482036690254806111 ) ) ;
#33136 = VERTEX_POINT ( 'NONE', #33472 ) ;
#33137 = ORIENTED_EDGE ( 'NONE', *, *, #22554, .F. ) ;
#33138 = CARTESIAN_POINT ( 'NONE',  ( -7.322902666698219321, 19.93973914737491526, -25.85775467558311647 ) ) ;
#33139 = DIRECTION ( 'NONE',  ( 0.000000000000000000, 0.000000000000000000, -1.000000000000000000 ) ) ;
#33140 = DIRECTION ( 'NONE',  ( 1.000000000000000000, 0.000000000000000000, 0.000000000000000000 ) ) ;
#33141 = AXIS2_PLACEMENT_3D ( 'NONE', #4413, #28591, #35704 ) ;
#33142 = DIRECTION ( 'NONE',  ( -0.8660254037844425934, -0.4999999999999933942, 0.000000000000000000 ) ) ;
#33143 = ORIENTED_EDGE ( 'NONE', *, *, #40040, .T. ) ;
#33144 = CARTESIAN_POINT ( 'NONE',  ( 20.52456465525489193, 0.9065716826278377161, -28.70867527313039602 ) ) ;
#33145 = AXIS2_PLACEMENT_3D ( 'NONE', #17636, #23909, #8473 ) ;
#33146 = CYLINDRICAL_SURFACE ( 'NONE', #35556, 21.00000000000002842 ) ;
#33147 = FACE_OUTER_BOUND ( 'NONE', #12307, .T. ) ;
#33148 = CARTESIAN_POINT ( 'NONE',  ( -2.444768620640030754, 7.712926687590090147, 10.49999999999999822 ) ) ;
#33149 = ORIENTED_EDGE ( 'NONE', *, *, #21707, .F. ) ;
#33150 = CARTESIAN_POINT ( 'NONE',  ( -29.58395905627514821, 0.06330276854539861053, -10.18073491376308404 ) ) ;
#33151 = B_SPLINE_CURVE_WITH_KNOTS ( 'NONE', 3,
 ( #10119, #29207, #31850, #1378 ),
 .UNSPECIFIED., .F., .F.,
 ( 4, 4 ),
 ( 0.000000000000000000, 1.000000000000000000 ),
 .UNSPECIFIED. ) ;
#33152 = ADVANCED_FACE ( 'NONE', ( #30416 ), #39255, .T. ) ;
#33153 = DIRECTION ( 'NONE',  ( 0.000000000000000000, 0.000000000000000000, -1.000000000000000000 ) ) ;
#33154 = ORIENTED_EDGE ( 'NONE', *, *, #14847, .T. ) ;
#33155 = CARTESIAN_POINT ( 'NONE',  ( 25.01210607124402685, -2.904145798682293389, -19.09601541136637337 ) ) ;
#33156 = CARTESIAN_POINT ( 'NONE',  ( 33.41351084210645439, -21.43470647212788194, 14.53008259254008472 ) ) ;
#33157 = ORIENTED_EDGE ( 'NONE', *, *, #6409, .F. ) ;
#33158 = CARTESIAN_POINT ( 'NONE',  ( 1.888379873391452080, 39.95159812444028091, 13.92931973827809067 ) ) ;
#33159 = B_SPLINE_CURVE_WITH_KNOTS ( 'NONE', 3,
 ( #20909, #33716, #26800, #17677 ),
 .UNSPECIFIED., .F., .F.,
 ( 4, 4 ),
 ( 0.000000000000000000, 1.000000000000000000 ),
 .UNSPECIFIED. ) ;
#33160 = CIRCLE ( 'NONE', #14318, 1.000000000000016431 ) ;
#33161 = CARTESIAN_POINT ( 'NONE',  ( -5.938964939928987441, -16.21345324574345170, 20.82122704794080192 ) ) ;
#33162 = CARTESIAN_POINT ( 'NONE',  ( 3.118671991557230516, 37.17221401100731981, 6.000000000000000000 ) ) ;
#33163 = CARTESIAN_POINT ( 'NONE',  ( -6.050433455602103287E-14, 29.93655406406124087, 20.82122704794079837 ) ) ;
#33164 = DIRECTION ( 'NONE',  ( 1.000000000000000000, 0.000000000000000000, 0.000000000000000000 ) ) ;
#33165 = ORIENTED_EDGE ( 'NONE', *, *, #12109, .T. ) ;
#33166 = DIRECTION ( 'NONE',  ( 1.000000000000000000, 0.000000000000000000, 0.000000000000000000 ) ) ;
#33167 = DIRECTION ( 'NONE',  ( 1.000000000000000000, 0.000000000000000000, 0.000000000000000000 ) ) ;
#33168 = CARTESIAN_POINT ( 'NONE',  ( 6.754942957401739889, 34.60620598615416554, -10.21839231443158980 ) ) ;
#33169 = AXIS2_PLACEMENT_3D ( 'NONE', #36601, #5913, #21361 ) ;
#33170 = CARTESIAN_POINT ( 'NONE',  ( 20.66458278928015702, 17.76169105511801050, -4.999999999999998224 ) ) ;
#33171 = CARTESIAN_POINT ( 'NONE',  ( 21.91791918713443721, -0.7365302468260908064, 20.50957957746798854 ) ) ;
#33172 = CONICAL_SURFACE ( 'NONE', #7191, 1.000000000000000888, 0.7853981633974552734 ) ;
#33173 = EDGE_CURVE ( 'NONE', #33798, #35217, #33272, .T. ) ;
#33174 = CARTESIAN_POINT ( 'NONE',  ( 11.78077084959020482, -16.85122407151366986, -28.61443936225239426 ) ) ;
#33175 = DIRECTION ( 'NONE',  ( -1.000000000000000000, 0.000000000000000000, 0.000000000000000000 ) ) ;
#33176 = CARTESIAN_POINT ( 'NONE',  ( 9.221287281574507944, 10.65863771052197784, 11.00000000000000000 ) ) ;
#33177 = DIRECTION ( 'NONE',  ( 0.000000000000000000, 0.000000000000000000, 1.000000000000000000 ) ) ;
#33178 = ORIENTED_EDGE ( 'NONE', *, *, #3666, .T. ) ;
#33179 = CARTESIAN_POINT ( 'NONE',  ( 13.44109819990983290, 22.91835836550887606, -15.43893112778157217 ) ) ;
#33180 = ORIENTED_EDGE ( 'NONE', *, *, #33660, .F. ) ;
#33181 = CARTESIAN_POINT ( 'NONE',  ( -15.49750644015885115, 26.39995258097018649, -5.946129726914544555 ) ) ;
#33182 = CARTESIAN_POINT ( 'NONE',  ( -19.02194587268434844, -24.34812480527924450, 18.87996532025819363 ) ) ;
#33183 = DIRECTION ( 'NONE',  ( 0.000000000000000000, 0.000000000000000000, 1.000000000000000000 ) ) ;
#33184 = CARTESIAN_POINT ( 'NONE',  ( 11.26998537048577909, 17.69417195558794376, -26.23399489620831915 ) ) ;
#33185 = VERTEX_POINT ( 'NONE', #36109 ) ;
#33186 = CARTESIAN_POINT ( 'NONE',  ( 32.49036733324588511, -19.22569735934472135, -7.970791907112693586 ) ) ;
#33187 = AXIS2_PLACEMENT_3D ( 'NONE', #20916, #5664, #30466 ) ;
#33188 = ORIENTED_EDGE ( 'NONE', *, *, #485, .F. ) ;
#33190 = CYLINDRICAL_SURFACE ( 'NONE', #40003, 1.000000000000000000 ) ;
#33189 = CARTESIAN_POINT ( 'NONE',  ( -12.07266892161228355, 20.90528892331724720, -19.43091586989769226 ) ) ;
#33191 = CARTESIAN_POINT ( 'NONE',  ( -18.36895873238599108, -27.24750037505589262, -5.462138457986313256 ) ) ;
#33192 = CARTESIAN_POINT ( 'NONE',  ( 14.85188145504474022, 20.30462949162087938, 10.49999999999999645 ) ) ;
#33193 = ORIENTED_EDGE ( 'NONE', *, *, #13339, .F. ) ;
#33194 = CARTESIAN_POINT ( 'NONE',  ( -29.06794499706158419, -9.974587258729167516, -14.80302332772542506 ) ) ;
#33195 = CARTESIAN_POINT ( 'NONE',  ( -10.03238663440694189, -19.23125872514161117, -23.87728478131429100 ) ) ;
#33196 = CARTESIAN_POINT ( 'NONE',  ( -5.184280209938394890, 31.68549066217158483, 10.50000000000000355 ) ) ;
#33197 = ORIENTED_EDGE ( 'NONE', *, *, #23609, .T. ) ;
#33198 = CARTESIAN_POINT ( 'NONE',  ( 23.21163472181913434, 2.226247987215279167, -19.68527219316008114 ) ) ;
#33199 = DIRECTION ( 'NONE',  ( 0.000000000000000000, 0.000000000000000000, 1.000000000000000000 ) ) ;
#33200 = CARTESIAN_POINT ( 'NONE',  ( 1.605696033269625955, 17.55816537872232530, 6.000000000000000000 ) ) ;
#33201 = VERTEX_POINT ( 'NONE', #5222 ) ;
#33202 = CARTESIAN_POINT ( 'NONE',  ( -29.89510730381624271, -0.05789195541120888133, -9.702364829962164094 ) ) ;
#33203 = EDGE_CURVE ( 'NONE', #34486, #25343, #7497, .T. ) ;
#33204 = ORIENTED_EDGE ( 'NONE', *, *, #15000, .F. ) ;
#33205 = CARTESIAN_POINT ( 'NONE',  ( 30.37910132873993874, -0.8766162490441101740, -10.11428594850108631 ) ) ;
#33206 = VECTOR ( 'NONE', #25544, 1000.000000000000114 ) ;
#33207 = ADVANCED_FACE ( 'NONE', ( #11721 ), #36707, .T. ) ;
#33208 = CARTESIAN_POINT ( 'NONE',  ( 18.99711117635948554, -25.05170312385142495, 18.42518152272109333 ) ) ;
#33209 = VECTOR ( 'NONE', #3263, 1000.000000000000000 ) ;
#33210 = EDGE_LOOP ( 'NONE', ( #7943, #22159, #39020, #31166 ) ) ;
#33211 = EDGE_CURVE ( 'NONE', #11176, #34232, #24108, .T. ) ;
#33212 = CARTESIAN_POINT ( 'NONE',  ( -20.18092276982249444, 3.603208870470906433, -29.99999999999999645 ) ) ;
#33213 = CARTESIAN_POINT ( 'NONE',  ( 7.096882951594525757, 29.56287847632727050, 10.00000000000000000 ) ) ;
#33214 = CARTESIAN_POINT ( 'NONE',  ( 1.000000000000000000, 37.50000000000000711, 10.50000000000000178 ) ) ;
#33215 = EDGE_CURVE ( 'NONE', #4297, #37780, #14568, .T. ) ;
#33216 = CYLINDRICAL_SURFACE ( 'NONE', #8356, 0.5000000000000000000 ) ;
#33217 = VECTOR ( 'NONE', #35782, 1000.000000000000000 ) ;
#33218 = DIRECTION ( 'NONE',  ( 1.000000000000000000, 0.000000000000000000, 0.000000000000000000 ) ) ;
#33219 = DIRECTION ( 'NONE',  ( -1.000000000000000000, 0.000000000000000000, 0.000000000000000000 ) ) ;
#33220 = DIRECTION ( 'NONE',  ( -0.000000000000000000, -0.000000000000000000, -1.000000000000000000 ) ) ;
#33221 = ORIENTED_EDGE ( 'NONE', *, *, #11983, .F. ) ;
#33222 = CARTESIAN_POINT ( 'NONE',  ( -19.92127511057237754, 5.002871685069139929, -28.81673539866426026 ) ) ;
#33223 = DIRECTION ( 'NONE',  ( 1.000000000000000000, 0.000000000000000000, 0.000000000000000000 ) ) ;
#33224 = CARTESIAN_POINT ( 'NONE',  ( 9.221287281574507944, 10.65863771052197784, 10.49999999999999822 ) ) ;
#33225 = CARTESIAN_POINT ( 'NONE',  ( 22.69918949349588289, -23.64247662620741153, -12.09428551148041997 ) ) ;
#33226 = EDGE_CURVE ( 'NONE', #17512, #25213, #1014, .T. ) ;
#33227 = CARTESIAN_POINT ( 'NONE',  ( 2.525645716490518389, 8.212903943950921715, 7.000000000000000000 ) ) ;
#33228 = CARTESIAN_POINT ( 'NONE',  ( -9.806982162272253944, 13.84996144622306247, 12.00000000000000000 ) ) ;
#33229 = EDGE_CURVE ( 'NONE', #38194, #31599, #30209, .T. ) ;
#33230 = CARTESIAN_POINT ( 'NONE',  ( 15.21602949246752878, 27.19738721321897046, -6.408861906063099134 ) ) ;
#33231 = CARTESIAN_POINT ( 'NONE',  ( -5.078902502065747449, -26.44091005802452798, 13.32518128616608877 ) ) ;
#33232 = ORIENTED_EDGE ( 'NONE', *, *, #39274, .T. ) ;
#33233 =( REPRESENTATION_RELATIONSHIP ('NONE','NONE', #15382, #12760 ) REPRESENTATION_RELATIONSHIP_WITH_TRANSFORMATION ( #17271 )SHAPE_REPRESENTATION_RELATIONSHIP( ) );
#33234 = CARTESIAN_POINT ( 'NONE',  ( -16.49044098933246971, 22.78194265982236999, -7.375859867825446337 ) ) ;
#33235 = CARTESIAN_POINT ( 'NONE',  ( -24.70330546561586615, -7.131334670376221041, 20.94377226548378701 ) ) ;
#33236 = CYLINDRICAL_SURFACE ( 'NONE', #23040, 6.000000000000001776 ) ;
#33237 = CARTESIAN_POINT ( 'NONE',  ( 15.24558589560055921, 26.36101825730073500, -7.828016443727952023 ) ) ;
#33238 = ORIENTED_EDGE ( 'NONE', *, *, #2203, .T. ) ;
#33239 = CARTESIAN_POINT ( 'NONE',  ( 12.30736835487432757, 14.81698729810772441, 7.000000000000000000 ) ) ;
#33240 = ORIENTED_EDGE ( 'NONE', *, *, #18293, .T. ) ;
#33242 = CARTESIAN_POINT ( 'NONE',  ( -12.74038105676665289, 14.56698729810790027, 11.00000000000000000 ) ) ;
#33241 = CARTESIAN_POINT ( 'NONE',  ( -13.12858674853676533, 22.38440377439352247, -16.42546611361683162 ) ) ;
#33243 = CARTESIAN_POINT ( 'NONE',  ( -15.27160128745916978, -26.39939704235120033, -7.827145747842149781 ) ) ;
#33244 = CARTESIAN_POINT ( 'NONE',  ( 7.848705329595008884, 10.27943253798616219, 10.66666666666666075 ) ) ;
#33245 = CARTESIAN_POINT ( 'NONE',  ( -20.71396996789364309, -11.66691485040002618, -21.83546244019694171 ) ) ;
#33246 = CARTESIAN_POINT ( 'NONE',  ( -5.633083642327312290, -21.97579894125815514, -18.92636197450212165 ) ) ;
#33247 = CARTESIAN_POINT ( 'NONE',  ( -23.54493052986482837, -14.21898406159469275, 21.00000000000000355 ) ) ;
#33248 = CARTESIAN_POINT ( 'NONE',  ( 16.04266474709265466, 24.30463473437875876, -6.894355676570810054 ) ) ;
#33249 = EDGE_LOOP ( 'NONE', ( #27838, #5206, #25540 ) ) ;
#33250 = CARTESIAN_POINT ( 'NONE',  ( 22.76663162612608815, 7.095554964298814049, -14.84575477948635047 ) ) ;
#33251 = CARTESIAN_POINT ( 'NONE',  ( 12.05833259093393117, 18.99598562053712314, -30.00000000000000000 ) ) ;
#33252 = AXIS2_PLACEMENT_3D ( 'NONE', #4648, #29430, #1606 ) ;
#33253 = CARTESIAN_POINT ( 'NONE',  ( 4.817371740575539185, 23.83900317890011422, 23.00000000000000000 ) ) ;
#33254 = CARTESIAN_POINT ( 'NONE',  ( -13.94482798346716201, 26.50521816028930644, 9.000000000000001776 ) ) ;
#33255 = ORIENTED_EDGE ( 'NONE', *, *, #916, .F. ) ;
#33256 = CARTESIAN_POINT ( 'NONE',  ( -27.65556173257783712, -0.4991889210311690195, -14.39343928979999454 ) ) ;
#33257 = EDGE_CURVE ( 'NONE', #39980, #13142, #13861, .T. ) ;
#33258 = CARTESIAN_POINT ( 'NONE',  ( 30.96479225765983045, -0.1042645752839200801, -4.999999999999999112 ) ) ;
#33259 = CIRCLE ( 'NONE', #20910, 1.000000000000000000 ) ;
#33260 = DIRECTION ( 'NONE',  ( 0.9510565162951544194, 0.3090169943749449533, -0.000000000000000000 ) ) ;
#33261 = EDGE_CURVE ( 'NONE', #39628, #38676, #2325, .T. ) ;
#33262 = CARTESIAN_POINT ( 'NONE',  ( 25.00594398452619771, -16.29738563782240490, 20.82122704794094048 ) ) ;
#33263 = LINE ( 'NONE', #36697, #26806 ) ;
#33264 = CARTESIAN_POINT ( 'NONE',  ( 16.87498849720599736, -29.16588574430810255, 10.99999999999838352 ) ) ;
#33265 = EDGE_CURVE ( 'NONE', #31717, #7910, #22134, .T. ) ;
#33266 = VECTOR ( 'NONE', #35612, 1000.000000000000000 ) ;
#33267 = ORIENTED_EDGE ( 'NONE', *, *, #38933, .T. ) ;
#33268 = DIRECTION ( 'NONE',  ( -1.000000000000000000, 0.000000000000000000, 0.000000000000000000 ) ) ;
#33269 = DIRECTION ( 'NONE',  ( 1.000000000000000000, 0.000000000000000000, 0.000000000000000000 ) ) ;
#33270 = ORIENTED_EDGE ( 'NONE', *, *, #24059, .F. ) ;
#33271 = CARTESIAN_POINT ( 'NONE',  ( 1.495161097472319733, 36.13038531284369981, -10.17381497340915253 ) ) ;
#33272 = LINE ( 'NONE', #5819, #16556 ) ;
#33273 = DIRECTION ( 'NONE',  ( -0.000000000000000000, 1.000000000000000000, -0.000000000000000000 ) ) ;
#33274 = AXIS2_PLACEMENT_3D ( 'NONE', #32949, #23791, #5107 ) ;
#33275 = PLANE ( 'NONE',  #10308 ) ;
#33276 = DIRECTION ( 'NONE',  ( -0.000000000000000000, -0.000000000000000000, 1.000000000000000000 ) ) ;
#33277 = CARTESIAN_POINT ( 'NONE',  ( 12.42073081513896327, 14.75153745115793313, 11.00000000000000000 ) ) ;
#33278 = CARTESIAN_POINT ( 'NONE',  ( 4.881458130668207218, -28.77689918168226058, 11.00000000000000000 ) ) ;
#33279 = EDGE_CURVE ( 'NONE', #20514, #32554, #5559, .T. ) ;
#33280 = CARTESIAN_POINT ( 'NONE',  ( 9.553997640115609258, 18.14112040201965925, -29.31786277955754016 ) ) ;
#33281 = CARTESIAN_POINT ( 'NONE',  ( 9.365580931528452169, 10.78282772046311599, 7.485646746502377269 ) ) ;
#33282 = ORIENTED_EDGE ( 'NONE', *, *, #28179, .F. ) ;
#33283 = CIRCLE ( 'NONE', #833, 1.000000000000000000 ) ;
#33285 = PLANE ( 'NONE',  #9045 ) ;
#33284 = CARTESIAN_POINT ( 'NONE',  ( -19.20284012471338642, 16.64839643360665633, -4.999999999999998224 ) ) ;
#33286 = DIRECTION ( 'NONE',  ( 1.000000000000000000, 0.000000000000000000, 0.000000000000000000 ) ) ;
#33287 = CARTESIAN_POINT ( 'NONE',  ( 11.20545772873020773, -20.46486250540106155, -20.53879684372101266 ) ) ;
#33288 = CARTESIAN_POINT ( 'NONE',  ( 23.61737546510196850, -7.194424252577107382, 21.00000000000000355 ) ) ;
#33289 = CARTESIAN_POINT ( 'NONE',  ( 15.22079284100554020, 26.44578639166762812, -7.826464274378870378 ) ) ;
#33290 = CARTESIAN_POINT ( 'NONE',  ( -18.69487370500357670, 22.45507383323637995, -5.000000000000000000 ) ) ;
#33291 = PLANE ( 'NONE',  #5696 ) ;
#33292 = CARTESIAN_POINT ( 'NONE',  ( -26.67886893852930541, -22.27379109059698337, -11.10442598990957208 ) ) ;
#33293 = CARTESIAN_POINT ( 'NONE',  ( 1.787030523841364404, -24.53966749997911379, -8.409682478326351074 ) ) ;
#33294 = CARTESIAN_POINT ( 'NONE',  ( 11.24783307583270542, 17.38369397674119909, -27.46121733726331016 ) ) ;
#33295 = CARTESIAN_POINT ( 'NONE',  ( 17.97214472351401326, 10.06683318593142396, -27.73766613656769309 ) ) ;
#33296 = CARTESIAN_POINT ( 'NONE',  ( 9.165204679926031162, 20.33931832809677331, 13.00000000000000178 ) ) ;
#33297 = CARTESIAN_POINT ( 'NONE',  ( -4.351811147998932761, 21.49055966318188382, -24.33120353158464155 ) ) ;
#33298 = VERTEX_POINT ( 'NONE', #34845 ) ;
#33299 = VECTOR ( 'NONE', #36264, 1000.000000000000114 ) ;
#33300 = CARTESIAN_POINT ( 'NONE',  ( -32.33143948541735568, 1.358872982502395521, 11.55979286843934872 ) ) ;
#33301 = VERTEX_POINT ( 'NONE', #31793 ) ;
#33302 = EDGE_CURVE ( 'NONE', #16943, #8916, #30855, .T. ) ;
#33303 = PLANE ( 'NONE',  #8994 ) ;
#33304 = AXIS2_PLACEMENT_3D ( 'NONE', #3267, #21551, #34749 ) ;
#33305 = CYLINDRICAL_SURFACE ( 'NONE', #16761, 18.00000000000002842 ) ;
#33306 = CARTESIAN_POINT ( 'NONE',  ( -30.43551396330494185, 0.4041362800276669942, -5.946213268253427664 ) ) ;
#33307 = CARTESIAN_POINT ( 'NONE',  ( 32.74700643712070303, -9.834764673945183944, -11.13845360772282511 ) ) ;
#33308 = AXIS2_PLACEMENT_3D ( 'NONE', #26515, #1942, #32620 ) ;
#33309 = ORIENTED_EDGE ( 'NONE', *, *, #1920, .F. ) ;
#33310 = APPLICATION_PROTOCOL_DEFINITION ( 'draft international standard', 'automotive_design', 1998, #3361 ) ;
#33311 = CARTESIAN_POINT ( 'NONE',  ( 8.541469607472738090, 17.40487552589537401, 13.00000000000000178 ) ) ;
#33312 = ORIENTED_EDGE ( 'NONE', *, *, #9062, .F. ) ;
#33313 = DIRECTION ( 'NONE',  ( 1.000000000000000000, 0.000000000000000000, 0.000000000000000000 ) ) ;
#33314 = DIRECTION ( 'NONE',  ( 0.000000000000000000, 0.000000000000000000, -1.000000000000000000 ) ) ;
#33315 = AXIS2_PLACEMENT_3D ( 'NONE', #14969, #21070, #8678 ) ;
#33316 = DIRECTION ( 'NONE',  ( 0.4999999999999921174, -0.8660254037844431485, -0.000000000000000000 ) ) ;
#33317 = ORIENTED_EDGE ( 'NONE', *, *, #39419, .T. ) ;
#33318 = CIRCLE ( 'NONE', #15782, 1.000000000000000888 ) ;
#33319 = CARTESIAN_POINT ( 'NONE',  ( 13.47830981910552062, 21.58612669357077607, 9.500000000000000000 ) ) ;
#33320 = FACE_OUTER_BOUND ( 'NONE', #14418, .T. ) ;
#33321 = CARTESIAN_POINT ( 'NONE',  ( 2.247466774197339756, 28.36888560440311480, 12.00000000000000000 ) ) ;
#33322 = CARTESIAN_POINT ( 'NONE',  ( 16.34210300462141774, 12.63939967215257276, -27.15615485920570649 ) ) ;
#33323 = CIRCLE ( 'NONE', #24859, 1.000000000000000888 ) ;
#33324 = CARTESIAN_POINT ( 'NONE',  ( 8.877500795550918866, 25.05368196378992351, -17.91181479415199718 ) ) ;
#33325 = EDGE_LOOP ( 'NONE', ( #6305, #37540, #24003, #12443 ) ) ;
#33326 = CARTESIAN_POINT ( 'NONE',  ( -18.72697364270403497, 8.503055164644706565, -28.29311283217969830 ) ) ;
#33327 = CARTESIAN_POINT ( 'NONE',  ( -6.354454053420248272, 35.54304081427989814, 9.000000000000001776 ) ) ;
#33328 = CARTESIAN_POINT ( 'NONE',  ( 5.100636323082810009, 29.29593658752792962, 13.00000000000000178 ) ) ;
#33329 = ADVANCED_FACE ( 'NONE', ( #6406 ), #21109, .T. ) ;
#33330 = MECHANICAL_DESIGN_GEOMETRIC_PRESENTATION_REPRESENTATION (  '', ( #17117 ), #38494 ) ;
#33331 = CARTESIAN_POINT ( 'NONE',  ( 11.91525068712948254, -20.93073338464350641, -19.44990459973941910 ) ) ;
#33332 = CARTESIAN_POINT ( 'NONE',  ( -6.101049646136835314, 36.20318186463909882, 7.000000000000000000 ) ) ;
#33333 = EDGE_CURVE ( 'NONE', #24423, #19575, #28545, .T. ) ;
#33334 = CARTESIAN_POINT ( 'NONE',  ( 22.40982762235196901, 2.618079236896951656, -30.00000000000000355 ) ) ;
#33335 = CARTESIAN_POINT ( 'NONE',  ( -15.09589218995242099, 26.15653917439733434, -8.766821195319815629 ) ) ;
#33336 = VECTOR ( 'NONE', #6058, 1000.000000000000000 ) ;
#33337 = CARTESIAN_POINT ( 'NONE',  ( -23.49851162867760834, -26.24496101125836489, -7.634993703461408820 ) ) ;
#33338 = CARTESIAN_POINT ( 'NONE',  ( 9.722871408072341737, -20.24786012184059203, -21.74715278292957521 ) ) ;
#33339 = CARTESIAN_POINT ( 'NONE',  ( 11.48173768534036121, 32.16538668264416145, 10.49999999999999822 ) ) ;
#33340 = EDGE_CURVE ( 'NONE', #9244, #23354, #34732, .T. ) ;
#33341 = VERTEX_POINT ( 'NONE', #34256 ) ;
#33342 = ORIENTED_EDGE ( 'NONE', *, *, #30842, .T. ) ;
#33343 = CARTESIAN_POINT ( 'NONE',  ( -7.187532856906145184, 19.54428593781422663, -27.17658705043585954 ) ) ;
#33344 = CARTESIAN_POINT ( 'NONE',  ( 33.75875814100317029, 2.759858869446390361, 3.000000000000000000 ) ) ;
#33345 = CARTESIAN_POINT ( 'NONE',  ( -12.99377146717201015, 26.19620116591435632, 9.500000000000000000 ) ) ;
#33346 = AXIS2_PLACEMENT_3D ( 'NONE', #28339, #38490, #22238 ) ;
#33347 = DIRECTION ( 'NONE',  ( -0.2876062384759501267, -0.6459741880212528375, -0.7071067811865461294 ) ) ;
#33348 = VERTEX_POINT ( 'NONE', #18814 ) ;
#33349 = CARTESIAN_POINT ( 'NONE',  ( 20.60629022519899323, 0.9185454123476016752, -28.08089029072296228 ) ) ;
#33350 = DIRECTION ( 'NONE',  ( -1.000000000000000000, 0.000000000000000000, 0.000000000000000000 ) ) ;
#33351 = CARTESIAN_POINT ( 'NONE',  ( -2.291516524179419978, 7.763791616332306411, 10.49999999999999822 ) ) ;
#33352 = ORIENTED_EDGE ( 'NONE', *, *, #9033, .T. ) ;
#33353 = CARTESIAN_POINT ( 'NONE',  ( -24.54801195516354184, 0.4553628621481798922, -18.45485564081276664 ) ) ;
#33354 = FACE_OUTER_BOUND ( 'NONE', #30428, .T. ) ;
#33355 = ORIENTED_EDGE ( 'NONE', *, *, #13497, .F. ) ;
#33356 = CARTESIAN_POINT ( 'NONE',  ( 22.04779665452936044, -3.160493293077858201, -23.41725161139969558 ) ) ;
#33357 = CIRCLE ( 'NONE', #5444, 0.5000000000000000000 ) ;
#33358 = CARTESIAN_POINT ( 'NONE',  ( 31.72789954390550093, 0.7664678198853781543, 14.53008259254011492 ) ) ;
#33359 = ORIENTED_EDGE ( 'NONE', *, *, #8910, .F. ) ;
#33360 = CARTESIAN_POINT ( 'NONE',  ( -14.19638663437040904, 32.12978188971815996, 14.53008259254011136 ) ) ;
#33361 = ADVANCED_FACE ( 'NONE', ( #31589 ), #12314, .T. ) ;
#33362 = CARTESIAN_POINT ( 'NONE',  ( 6.143904198944455608, -13.77689918168226235, 20.99999999999999645 ) ) ;
#33363 = CARTESIAN_POINT ( 'NONE',  ( -31.47283671532259675, -25.12609584734821411, -5.000000000000013323 ) ) ;
#33364 = CARTESIAN_POINT ( 'NONE',  ( -3.166027244386082629, 31.89862848374658455, 20.25080042701565830 ) ) ;
#33365 = CIRCLE ( 'NONE', #15829, 0.4999999999999993339 ) ;
#33366 = DIRECTION ( 'NONE',  ( 0.9945218953682730678, -0.1045284632676569819, 0.000000000000000000 ) ) ;
#33367 = ORIENTED_EDGE ( 'NONE', *, *, #22787, .F. ) ;
#33368 = CARTESIAN_POINT ( 'NONE',  ( -13.22866120779009336, 26.17694675929173798, 18.42518152272108267 ) ) ;
#33369 = FACE_OUTER_BOUND ( 'NONE', #22490, .T. ) ;
#33370 = CARTESIAN_POINT ( 'NONE',  ( 8.094956495243176064, 35.93012217760205118, -7.153226857005175354 ) ) ;
#33371 = DIRECTION ( 'NONE',  ( 0.000000000000000000, 0.000000000000000000, 1.000000000000000000 ) ) ;
#33372 = VECTOR ( 'NONE', #31453, 1000.000000000000000 ) ;
#33373 = CARTESIAN_POINT ( 'NONE',  ( 14.79097147050401873, 14.99953367535683668, 19.66345542862543638 ) ) ;
#33374 = EDGE_CURVE ( 'NONE', #23691, #17784, #719, .T. ) ;
#33375 = CARTESIAN_POINT ( 'NONE',  ( 17.41019067503492579, -24.19678871709856338, -13.24119691528997578 ) ) ;
#33376 = CARTESIAN_POINT ( 'NONE',  ( -15.98961535660691347, 30.99268274074325902, 10.99999999999966604 ) ) ;
#33377 = CARTESIAN_POINT ( 'NONE',  ( 11.11016527260166420, 31.83082137946473367, 7.499999999999997335 ) ) ;
#33378 = LINE ( 'NONE', #5522, #13551 ) ;
#33379 = PRODUCT_RELATED_PRODUCT_CATEGORY ( 'part', '', ( #7087 ) ) ;
#33380 = ORIENTED_EDGE ( 'NONE', *, *, #39678, .F. ) ;
#33381 = CARTESIAN_POINT ( 'NONE',  ( 10.93429579500015159, 17.39409148898324986, -28.70396595981947385 ) ) ;
#33382 = CONICAL_SURFACE ( 'NONE', #28171, 1.000000000000002665, 0.7853981633974548293 ) ;
#33383 = EDGE_LOOP ( 'NONE', ( #2092, #11255, #5784, #3105 ) ) ;
#33384 = CARTESIAN_POINT ( 'NONE',  ( -14.25035268484812079, 23.42487517527639795, -13.53819545498157240 ) ) ;
#33385 = CARTESIAN_POINT ( 'NONE',  ( -27.44755207257315988, -22.53416897284578368, 18.42518152272109333 ) ) ;
#33386 = ADVANCED_FACE ( 'NONE', ( #10060, #31006 ), #34055, .T. ) ;
#33387 = CARTESIAN_POINT ( 'NONE',  ( -3.900351417861621428, 8.105760029628179097, 10.49999999999999822 ) ) ;
#33388 = CARTESIAN_POINT ( 'NONE',  ( 11.56427562401083797, 18.36828347780292958, -23.86608368699767979 ) ) ;
#33389 = EDGE_CURVE ( 'NONE', #25420, #31354, #11921, .T. ) ;
#33390 = EDGE_LOOP ( 'NONE', ( #12100, #29386, #37922, #38931 ) ) ;
#33391 = CARTESIAN_POINT ( 'NONE',  ( 32.30856083864753714, -20.47190428664634609, -6.697067119202526619 ) ) ;
#33392 = VERTEX_POINT ( 'NONE', #19200 ) ;
#33394 = DIRECTION ( 'NONE',  ( 0.000000000000000000, -0.000000000000000000, -1.000000000000000000 ) ) ;
#33393 = CARTESIAN_POINT ( 'NONE',  ( -12.40092118849391589, 21.42237501319575443, -18.39783089657061055 ) ) ;
#33395 = CARTESIAN_POINT ( 'NONE',  ( -10.20341636066711288, -17.78360352085077878, -29.99999999999999645 ) ) ;
#33396 = DIRECTION ( 'NONE',  ( -0.000000000000000000, -0.000000000000000000, -1.000000000000000000 ) ) ;
#33397 = ORIENTED_EDGE ( 'NONE', *, *, #15348, .F. ) ;
#33398 = CARTESIAN_POINT ( 'NONE',  ( -30.84121824956582714, -11.62399599295376973, -12.93016321018791892 ) ) ;
#33399 = PRODUCT_DEFINITION_CONTEXT ( 'detailed design', #31140, 'design' ) ;
#33400 = CARTESIAN_POINT ( 'NONE',  ( -9.442374748160709430, -18.42736121383703463, -27.46044148871083124 ) ) ;
#33401 = CARTESIAN_POINT ( 'NONE',  ( 29.22254794995044946, -28.85350742528273926, 22.99999999999905853 ) ) ;
#33402 = ORIENTED_EDGE ( 'NONE', *, *, #3444, .T. ) ;
#33403 = CARTESIAN_POINT ( 'NONE',  ( 22.88331890279000547, 2.992971246632968096, -19.75484460905745365 ) ) ;
#33404 = DIRECTION ( 'NONE',  ( 1.000000000000000000, 0.000000000000000000, 0.000000000000000000 ) ) ;
#33405 = DIRECTION ( 'NONE',  ( 1.000000000000000000, 0.000000000000000000, 0.000000000000000000 ) ) ;
#33406 = VERTEX_POINT ( 'NONE', #25486 ) ;
#33407 = CARTESIAN_POINT ( 'NONE',  ( -30.95087757567503672, -0.08989953764334650266, -5.473884744044031692 ) ) ;
#33408 = VERTEX_POINT ( 'NONE', #3365 ) ;
#33409 = CARTESIAN_POINT ( 'NONE',  ( 31.81105852766241071, -1.386432505721455044, -7.313011137699476194 ) ) ;
#33410 = CARTESIAN_POINT ( 'NONE',  ( 34.17506821248620952, -14.20748230372561238, 17.42190598798392998 ) ) ;
#33411 = ADVANCED_FACE ( 'NONE', ( #25100 ), #37886, .T. ) ;
#33412 = VERTEX_POINT ( 'NONE', #3563 ) ;
#33413 = CARTESIAN_POINT ( 'NONE',  ( -24.03416057413138063, 3.517989641964785363, -16.69879147254576424 ) ) ;
#33414 = EDGE_CURVE ( 'NONE', #19420, #40188, #6996, .T. ) ;
#33415 = CIRCLE ( 'NONE', #26088, 1.000000000000002665 ) ;
#33416 = CARTESIAN_POINT ( 'NONE',  ( 0.5000000000000004441, 36.00000000000000711, 9.500000000000000000 ) ) ;
#33417 = AXIS2_PLACEMENT_3D ( 'NONE', #35967, #32527, #30070 ) ;
#33418 = CARTESIAN_POINT ( 'NONE',  ( -6.577547685840081648, 11.84256962714647798, 12.00000000000000000 ) ) ;
#33419 = CARTESIAN_POINT ( 'NONE',  ( 14.47283171447379502, 21.48159823030311344, 7.000000000000000000 ) ) ;
#33420 = CARTESIAN_POINT ( 'NONE',  ( -3.161220354320351422, 12.43736188311283897, 11.00000000000000000 ) ) ;
#33421 = VECTOR ( 'NONE', #20029, 1000.000000000000114 ) ;
#33422 = CIRCLE ( 'NONE', #6133, 1.000000000000000000 ) ;
#33423 = FACE_BOUND ( 'NONE', #35502, .T. ) ;
#33424 = DIRECTION ( 'NONE',  ( 1.000000000000000000, 0.000000000000000000, 0.000000000000000000 ) ) ;
#33425 = VERTEX_POINT ( 'NONE', #15961 ) ;
#33426 = CARTESIAN_POINT ( 'NONE',  ( -25.12800499762355599, 6.178422606789070848, -8.856332134561709424 ) ) ;
#33427 = CARTESIAN_POINT ( 'NONE',  ( -4.100643064501314328, 15.70406341247269211, 6.000000000000000000 ) ) ;
#33428 = DIRECTION ( 'NONE',  ( 1.000000000000000000, 0.000000000000000000, 0.000000000000000000 ) ) ;
#33429 = CARTESIAN_POINT ( 'NONE',  ( 25.25565081207486884, -26.17063864068946444, -5.878154196310728885 ) ) ;
#33430 = CARTESIAN_POINT ( 'NONE',  ( -9.997483185316568211, 21.95197631500770186, 10.49999999999999289 ) ) ;
#33431 = EDGE_CURVE ( 'NONE', #4287, #34838, #523, .T. ) ;
#33432 = CARTESIAN_POINT ( 'NONE',  ( 15.07890253828262672, 26.90834617882325830, -7.811347429530628439 ) ) ;
#33433 = CARTESIAN_POINT ( 'NONE',  ( 10.19059090746689833, -26.87498467585813344, 13.92931973827711900 ) ) ;
#33434 = EDGE_LOOP ( 'NONE', ( #37339, #21736 ) ) ;
#33435 = CARTESIAN_POINT ( 'NONE',  ( -14.97475431996716466, 18.42973550644392233, -17.73616635726436286 ) ) ;
#33436 = CARTESIAN_POINT ( 'NONE',  ( -26.10558707266139677, -11.85287147006304309, 20.94377226548378346 ) ) ;
#33437 = CARTESIAN_POINT ( 'NONE',  ( 19.48557158514975285, -11.24999999999995737, 10.00000000000000000 ) ) ;
#33438 = CARTESIAN_POINT ( 'NONE',  ( 15.35012758518023723, 26.57588627132344783, -6.887990273041626921 ) ) ;
#33439 = EDGE_LOOP ( 'NONE', ( #23993, #23484, #28778 ) ) ;
#33440 = CARTESIAN_POINT ( 'NONE',  ( 11.68691289177315085, 18.91070414389386656, -22.73532874761467326 ) ) ;
#33441 = ORIENTED_EDGE ( 'NONE', *, *, #38997, .T. ) ;
#33443 = CARTESIAN_POINT ( 'NONE',  ( 14.64210930126480115, 24.20081211342298744, 13.00000000000000178 ) ) ;
#33442 = CARTESIAN_POINT ( 'NONE',  ( -15.03952492485649550, 26.34161984541752588, -8.758635656526267965 ) ) ;
#33444 = CARTESIAN_POINT ( 'NONE',  ( -9.744066905365848186, -18.41592494163657889, -26.82585431338213411 ) ) ;
#33445 = CARTESIAN_POINT ( 'NONE',  ( 8.118377661053333583, 10.47536095541699197, 11.00000000000000000 ) ) ;
#33446 = AXIS2_PLACEMENT_3D ( 'NONE', #17036, #20082, #22910 ) ;
#33447 = CARTESIAN_POINT ( 'NONE',  ( -33.58157224492879322, -18.91014262129728962, -5.435336751253355025 ) ) ;
#33448 = CARTESIAN_POINT ( 'NONE',  ( -11.53315257097601254, -25.74693630043225667, -6.423746070632376792 ) ) ;
#33449 = CARTESIAN_POINT ( 'NONE',  ( -18.23649648353780961, -16.09146789626143814, 20.99999999999999645 ) ) ;
#33450 = CARTESIAN_POINT ( 'NONE',  ( 13.89352154402242334, 21.03800918229289252, -16.54585482098419646 ) ) ;
#33451 = ORIENTED_EDGE ( 'NONE', *, *, #19600, .F. ) ;
#33452 = CARTESIAN_POINT ( 'NONE',  ( 19.65936727364617198, 6.642930537632695476, -26.56611033146918999 ) ) ;
#33453 = CARTESIAN_POINT ( 'NONE',  ( -1.605702774688126722, 27.44183462127829642, 12.00000000000000000 ) ) ;
#33454 = FACE_OUTER_BOUND ( 'NONE', #1204, .T. ) ;
#33455 = CARTESIAN_POINT ( 'NONE',  ( -32.33143948541797386, 1.358872982501903248, 11.00000000000000000 ) ) ;
#33456 = CIRCLE ( 'NONE', #13964, 1.000000000000000888 ) ;
#33457 = EDGE_LOOP ( 'NONE', ( #14292, #16803, #19285, #26942 ) ) ;
#33458 = CARTESIAN_POINT ( 'NONE',  ( -20.49507156785942641, -0.4678258087238867380, -29.32393442354705471 ) ) ;
#33459 = CARTESIAN_POINT ( 'NONE',  ( 30.54358385272748677, -0.07321200605768496406, -7.825060034502334894 ) ) ;
#33460 = VECTOR ( 'NONE', #14620, 1000.000000000000000 ) ;
#33461 = AXIS2_PLACEMENT_3D ( 'NONE', #5689, #36574, #5890 ) ;
#33462 = CARTESIAN_POINT ( 'NONE',  ( 5.187504188494417079, 36.60991850771481637, 10.50000000000000000 ) ) ;
#33463 = CARTESIAN_POINT ( 'NONE',  ( 19.22070351544489597, -18.72532327798363383, 20.82122704794079482 ) ) ;
#33464 = PLANE ( 'NONE',  #9300 ) ;
#33465 = EDGE_CURVE ( 'NONE', #31607, #19767, #3958, .T. ) ;
#33466 = CARTESIAN_POINT ( 'NONE',  ( 37.09709568333403240, -7.051483854461488399, 11.00000000000007994 ) ) ;
#33467 = ORIENTED_EDGE ( 'NONE', *, *, #26045, .F. ) ;
#33468 = CARTESIAN_POINT ( 'NONE',  ( 14.99771543937018414, 22.21207258816060559, 7.102637441331453694 ) ) ;
#33469 = CARTESIAN_POINT ( 'NONE',  ( 6.830039222088956308, 35.38192592444566742, 10.49999999999999822 ) ) ;
#33470 = CARTESIAN_POINT ( 'NONE',  ( -3.118678732975735279, 7.827785988993307242, 6.000000000000000000 ) ) ;
#33471 = CARTESIAN_POINT ( 'NONE',  ( 1.533581810152732761, 37.14075507769783258, -8.844061256007341498 ) ) ;
#33472 = CARTESIAN_POINT ( 'NONE',  ( -3.914034194965524183, 30.06176806842423943, 7.000000000000000000 ) ) ;
#33473 = CARTESIAN_POINT ( 'NONE',  ( 10.34254640628217992, 25.37474234120048067, 19.99202127657104100 ) ) ;
#33474 = LINE ( 'NONE', #30420, #28489 ) ;
#33475 = CARTESIAN_POINT ( 'NONE',  ( -14.96930490892015797, 21.54088032874991399, 7.500000000000004441 ) ) ;
#33476 = DIRECTION ( 'NONE',  ( -0.000000000000000000, -0.000000000000000000, -1.000000000000000000 ) ) ;
#33477 = EDGE_CURVE ( 'NONE', #18376, #9166, #24903, .T. ) ;
#33478 = CARTESIAN_POINT ( 'NONE',  ( 6.354454053420414361, 35.54304081427980577, 7.000000000000000000 ) ) ;
#33479 = CARTESIAN_POINT ( 'NONE',  ( 9.864563461025730007, 18.03425384675588816, -28.65979497051309721 ) ) ;
#33481 = VECTOR ( 'NONE', #26092, 999.9999999999998863 ) ;
#33480 = LINE ( 'NONE', #36317, #26902 ) ;
#33482 = ORIENTED_EDGE ( 'NONE', *, *, #11685, .T. ) ;
#33485 = CIRCLE ( 'NONE', #30249, 0.9999999999999995559 ) ;
#33484 = LINE ( 'NONE', #23721, #25879 ) ;
#33483 = CARTESIAN_POINT ( 'NONE',  ( -15.97641923477408454, 13.01946753566105919, -27.71082971353359170 ) ) ;
#33486 = FACE_OUTER_BOUND ( 'NONE', #31024, .T. ) ;
#33487 = EDGE_CURVE ( 'NONE', #20155, #31096, #4361, .T. ) ;
#33488 = CARTESIAN_POINT ( 'NONE',  ( 15.44845846858325267, -26.70665584896979183, -5.946081595203406955 ) ) ;
#33489 = CARTESIAN_POINT ( 'NONE',  ( 14.84111742463143813, 25.60591702902538813, -10.18041830445565843 ) ) ;
#33490 = CARTESIAN_POINT ( 'NONE',  ( 11.05073784553093219, 17.51747009666078725, -27.44606399619430448 ) ) ;
#33491 = ORIENTED_EDGE ( 'NONE', *, *, #14614, .T. ) ;
#33492 = CARTESIAN_POINT ( 'NONE',  ( 7.118377661053320260, 10.47536095541698486, 7.000000000000000000 ) ) ;
#33493 = DIRECTION ( 'NONE',  ( 1.000000000000000000, 0.000000000000000000, 0.000000000000000000 ) ) ;
#33494 = ADVANCED_FACE ( 'NONE', ( #19809 ), #23051, .F. ) ;
#33495 = CARTESIAN_POINT ( 'NONE',  ( -26.00859912514732741, -20.40482213449253379, -12.92116335214409162 ) ) ;
#33496 = CARTESIAN_POINT ( 'NONE',  ( -2.510360893402116655, -24.33974617660730289, -9.887043164262214745 ) ) ;
#33497 = CARTESIAN_POINT ( 'NONE',  ( 14.77156457488188934, 24.32677381516164061, -11.61821993547884802 ) ) ;
#33498 = CARTESIAN_POINT ( 'NONE',  ( 21.63088251164382214, 12.03979545591979772, -5.967650224983321650 ) ) ;
#33499 = CARTESIAN_POINT ( 'NONE',  ( 1.693998953219512105, 12.12549434688614625, 11.00000000000000000 ) ) ;
#33500 = B_SPLINE_CURVE_WITH_KNOTS ( 'NONE', 3,
 ( #27632, #3647, #24984, #28230, #31283, #28426, #18497, #9946, #9351, #5896, #18299, #34138, #40015, #12594, #12193, #9149, #6289, #31087 ),
 .UNSPECIFIED., .F., .F.,
 ( 4, 2, 2, 2, 2, 2, 2, 2, 4 ),
 ( 0.000000000000000000, 0.1250000000000001943, 0.2500000000000001665, 0.3750000000000001110, 0.5000000000000001110, 0.6250000000000001110, 0.7500000000000000000, 0.8750000000000000000, 1.000000000000000000 ),
 .UNSPECIFIED. ) ;
#33501 = CARTESIAN_POINT ( 'NONE',  ( -3.299821718920390001, 23.43477659572061711, -21.89659664273044370 ) ) ;
#33502 = ORIENTED_EDGE ( 'NONE', *, *, #21667, .F. ) ;
#33503 = CARTESIAN_POINT ( 'NONE',  ( -18.69515074622356821, 22.45407711376244109, 11.00000000002425971 ) ) ;
#33504 = ORIENTED_EDGE ( 'NONE', *, *, #16846, .F. ) ;
#33505 = CARTESIAN_POINT ( 'NONE',  ( 0.9819609608163288872, 14.62372257652092422, 13.00000000000000178 ) ) ;
#33506 = DIRECTION ( 'NONE',  ( -0.000000000000000000, -0.000000000000000000, 1.000000000000000000 ) ) ;
#33507 = CARTESIAN_POINT ( 'NONE',  ( -20.80513200209605884, 0.9511744672526275535, -26.83982028479031356 ) ) ;
#33508 = ADVANCED_FACE ( 'NONE', ( #35654 ), #20419, .F. ) ;
#33509 = CARTESIAN_POINT ( 'NONE',  ( 30.13983096139770979, -9.052337329862529813, -13.90091081929475081 ) ) ;
#33510 = EDGE_CURVE ( 'NONE', #1570, #12591, #35850, .T. ) ;
#33511 = AXIS2_PLACEMENT_3D ( 'NONE', #18387, #18192, #2940 ) ;
#33512 = AXIS2_PLACEMENT_3D ( 'NONE', #24515, #8484, #17844 ) ;
#33513 = ORIENTED_EDGE ( 'NONE', *, *, #21557, .F. ) ;
#33514 = CARTESIAN_POINT ( 'NONE',  ( -2.036571916123810055, 8.108948098542073879, 10.49999999999999822 ) ) ;
#33515 = ORIENTED_EDGE ( 'NONE', *, *, #19587, .F. ) ;
#33516 = CARTESIAN_POINT ( 'NONE',  ( 14.97283170755579818, 21.46414480565946903, 10.49999999999999822 ) ) ;
#33517 = CARTESIAN_POINT ( 'NONE',  ( 9.625795778761983001, 10.95253033666821274, 10.50000000000000000 ) ) ;
#33518 = CARTESIAN_POINT ( 'NONE',  ( -2.568190708544555001, 12.82247983807085134, 10.50000000000000533 ) ) ;
#33519 = ORIENTED_EDGE ( 'NONE', *, *, #27995, .T. ) ;
#33520 = CARTESIAN_POINT ( 'NONE',  ( 9.541469607472739867, 17.40487552589537401, 6.000000000000000000 ) ) ;
#33521 = CYLINDRICAL_SURFACE ( 'NONE', #39683, 0.5000000000000004441 ) ;
#33522 = FACE_OUTER_BOUND ( 'NONE', #18385, .T. ) ;
#33523 = CARTESIAN_POINT ( 'NONE',  ( 21.99787872679462808, -16.91788285020105675, -17.63963683105944824 ) ) ;
#33524 = EDGE_CURVE ( 'NONE', #6233, #22876, #25890, .T. ) ;
#33525 = CARTESIAN_POINT ( 'NONE',  ( 19.91164419919741846, 14.82880737701476548, -7.913098018804059386 ) ) ;
#33526 = CARTESIAN_POINT ( 'NONE',  ( 11.10948248300046082, 31.49357332391675968, -10.33061176195978170 ) ) ;
#33527 = ORIENTED_EDGE ( 'NONE', *, *, #26093, .T. ) ;
#33528 = CARTESIAN_POINT ( 'NONE',  ( -21.41702733524243030, 11.56821114029789754, -9.888691875779725748 ) ) ;
#33529 = CARTESIAN_POINT ( 'NONE',  ( -4.678013043399448456, 44.50832101651065642, 7.000000000000000000 ) ) ;
#33530 = CARTESIAN_POINT ( 'NONE',  ( -36.48557158514989140, -11.24999999999987743, 10.00000000000000000 ) ) ;
#33531 = ADVANCED_FACE ( 'NONE', ( #38290 ), #20014, .F. ) ;
#33532 = CARTESIAN_POINT ( 'NONE',  ( 10.96665850233910966, -19.96023790109854090, -21.59991616212109733 ) ) ;
#33533 = DIRECTION ( 'NONE',  ( 1.000000000000000000, 0.000000000000000000, 0.000000000000000000 ) ) ;
#33534 = CARTESIAN_POINT ( 'NONE',  ( 19.69645987729881043, 11.37175641224107814, -21.56489709563629376 ) ) ;
#33535 = CARTESIAN_POINT ( 'NONE',  ( -14.51563583855034878, 25.01866666866954603, -11.59546205423767873 ) ) ;
#33536 = CIRCLE ( 'NONE', #3642, 18.00000000000000355 ) ;
#33537 = CARTESIAN_POINT ( 'NONE',  ( -14.90132355581796730, -16.76330623373688411, -23.29508989526930662 ) ) ;
#33538 = CARTESIAN_POINT ( 'NONE',  ( 13.35370518262597983, -25.77141642152969325, -8.785306460286980368 ) ) ;
#33539 = CARTESIAN_POINT ( 'NONE',  ( -7.953812613386786801, 14.77701242934787906, 6.000000000000000000 ) ) ;
#33540 = EDGE_LOOP ( 'NONE', ( #35783, #28111, #21549, #8425 ) ) ;
#33541 = ORIENTED_EDGE ( 'NONE', *, *, #466, .F. ) ;
#33542 = CARTESIAN_POINT ( 'NONE',  ( -6.109668991155474238, 20.41692942102680419, -25.77087616168875783 ) ) ;
#33543 = DIRECTION ( 'NONE',  ( 0.000000000000000000, 0.000000000000000000, 1.000000000000000000 ) ) ;
#33544 = DIRECTION ( 'NONE',  ( 0.000000000000000000, 0.000000000000000000, 1.000000000000000000 ) ) ;
#33545 = DIRECTION ( 'NONE',  ( 1.000000000000000000, 3.469446951953598806E-15, 0.000000000000000000 ) ) ;
#33546 = VERTEX_POINT ( 'NONE', #10668 ) ;
#33547 = CARTESIAN_POINT ( 'NONE',  ( 24.53203630004508184, 0.4888770433563241480, -18.45847561789426550 ) ) ;
#33548 = CARTESIAN_POINT ( 'NONE',  ( -1.265509184090266137, 8.754836972118123839, 13.00000000000000178 ) ) ;
#33549 = CARTESIAN_POINT ( 'NONE',  ( 13.62967667376826419, 40.40898974728997217, 11.00000000000000000 ) ) ;
#33550 = EDGE_LOOP ( 'NONE', ( #36238, #15147, #25676 ) ) ;
#33551 = CARTESIAN_POINT ( 'NONE',  ( -27.73675306567175269, 0.1912042389513601559, -13.51357499948137963 ) ) ;
#33552 = FACE_OUTER_BOUND ( 'NONE', #29431, .T. ) ;
#33553 = ORIENTED_EDGE ( 'NONE', *, *, #29419, .T. ) ;
#33554 = CARTESIAN_POINT ( 'NONE',  ( 20.45176271469480866, -2.234166952769147230, -28.59864995799237164 ) ) ;
#33555 = CARTESIAN_POINT ( 'NONE',  ( 35.73276616393376770, -5.440996109072101738, 14.53008259253983248 ) ) ;
#33556 = ORIENTED_EDGE ( 'NONE', *, *, #28126, .T. ) ;
#33557 = CARTESIAN_POINT ( 'NONE',  ( 16.52773037515741805, 27.09393310379826758, 14.53008259254011136 ) ) ;
#33558 = EDGE_CURVE ( 'NONE', #3451, #5601, #25640, .T. ) ;
#33559 = CARTESIAN_POINT ( 'NONE',  ( 4.307564594982224211E-14, -17.04122685614420263, 20.69868183039781684 ) ) ;
#33560 = CARTESIAN_POINT ( 'NONE',  ( 0.000000000000000000, 22.50000000000000355, 10.00000000000000000 ) ) ;
#33561 = CARTESIAN_POINT ( 'NONE',  ( -8.773674293808889584E-14, 33.23463598332012481, 19.99202127657103034 ) ) ;
#33562 = CIRCLE ( 'NONE', #8229, 59.99999999999995026 ) ;
#33563 = CARTESIAN_POINT ( 'NONE',  ( 10.70158575030369796, 30.79011836036717753, 10.00000000000000000 ) ) ;
#33564 = EDGE_LOOP ( 'NONE', ( #18673, #30352, #564, #14405 ) ) ;
#33565 = CARTESIAN_POINT ( 'NONE',  ( 10.81260707898150386, 32.90853150812155548, 10.49999999999999822 ) ) ;
#33566 = CYLINDRICAL_SURFACE ( 'NONE', #2676, 1.000000000000000000 ) ;
#33567 = CARTESIAN_POINT ( 'NONE',  ( 3.279674764711696611, 20.24540435116753301, -30.00000000000000000 ) ) ;
#33568 = CARTESIAN_POINT ( 'NONE',  ( -9.151574469205524309, 1.945227203041487218, 7.000000000000000000 ) ) ;
#33569 = CARTESIAN_POINT ( 'NONE',  ( 11.07177992392776567, 13.25002113302786988, 20.82122704794082679 ) ) ;
#33570 = CARTESIAN_POINT ( 'NONE',  ( 13.78700921972296811, -18.31297507672437774, -22.32604137707055969 ) ) ;
#33571 = DIRECTION ( 'NONE',  ( 1.000000000000000000, 0.000000000000000000, 0.000000000000000000 ) ) ;
#33572 = DIRECTION ( 'NONE',  ( -0.7071067811865493491, 0.000000000000000000, -0.7071067811865456854 ) ) ;
#33573 = DIRECTION ( 'NONE',  ( -1.000000000000000000, 0.000000000000000000, 0.000000000000000000 ) ) ;
#33574 = VERTEX_POINT ( 'NONE', #22844 ) ;
#33575 = CARTESIAN_POINT ( 'NONE',  ( 15.20466363552954014, 26.50075720148702985, -7.824641958460332170 ) ) ;
#33576 = ORIENTED_EDGE ( 'NONE', *, *, #27498, .T. ) ;
#33577 = CARTESIAN_POINT ( 'NONE',  ( -12.53910291074082295, 20.29581086541950441, -19.52226377206912034 ) ) ;
#33578 = CARTESIAN_POINT ( 'NONE',  ( -25.82842257350429804, -22.71926374633573786, 18.87996532025750440 ) ) ;
#33579 = CARTESIAN_POINT ( 'NONE',  ( 13.62263039894608774, -24.10683431214565431, -13.51722375663292830 ) ) ;
#33580 = CARTESIAN_POINT ( 'NONE',  ( -3.607749162633349105, 7.931741834401817570, 10.59344459855560316 ) ) ;
#33581 = CARTESIAN_POINT ( 'NONE',  ( 14.09135169103296725, 23.79168831276296103, -13.52014011376467373 ) ) ;
#33582 = ORIENTED_EDGE ( 'NONE', *, *, #19085, .T. ) ;
#33583 = CARTESIAN_POINT ( 'NONE',  ( 21.28379295669234139, -14.39448103213696228, -19.64396054145414183 ) ) ;
#33584 = ORIENTED_EDGE ( 'NONE', *, *, #3997, .T. ) ;
#33586 = CARTESIAN_POINT ( 'NONE',  ( 8.412270287199559604, 10.07085245822950981, 10.50000000000000178 ) ) ;
#33585 = CARTESIAN_POINT ( 'NONE',  ( -14.77784559536929443, 28.35253144409951176, -6.851657844549249532 ) ) ;
#33587 = CARTESIAN_POINT ( 'NONE',  ( -13.11275354201897692, -20.03949469003612904, -20.29527925755206752 ) ) ;
#33588 = DIRECTION ( 'NONE',  ( 1.000000000000000000, 0.000000000000000000, 0.000000000000000000 ) ) ;
#33589 = VECTOR ( 'NONE', #23442, 1000.000000000000000 ) ;
#33590 = AXIS2_PLACEMENT_3D ( 'NONE', #26983, #14795, #23935 ) ;
#33591 = ORIENTED_EDGE ( 'NONE', *, *, #19694, .F. ) ;
#33592 = CARTESIAN_POINT ( 'NONE',  ( -20.01100984268285288, -7.597414617152628225, -25.63648934281255976 ) ) ;
#33593 = CARTESIAN_POINT ( 'NONE',  ( -14.74418213917750364, -26.06945053339236296, -8.770932666061078464 ) ) ;
#33594 = CARTESIAN_POINT ( 'NONE',  ( 36.53988293556081857, -0.5802930328954534200, 11.00000000000000000 ) ) ;
#33595 = ORIENTED_EDGE ( 'NONE', *, *, #5391, .F. ) ;
#33596 = CARTESIAN_POINT ( 'NONE',  ( 28.51836663967885599, 2.011535347156353737, -8.319471814027734169 ) ) ;
#33597 = DIRECTION ( 'NONE',  ( 1.000000000000000000, 0.000000000000000000, 0.000000000000000000 ) ) ;
#33598 = CYLINDRICAL_SURFACE ( 'NONE', #13439, 1.000000000000000000 ) ;
#33599 = AXIS2_PLACEMENT_3D ( 'NONE', #6985, #19391, #31787 ) ;
#33600 = EDGE_LOOP ( 'NONE', ( #1741, #36520 ) ) ;
#33601 = CARTESIAN_POINT ( 'NONE',  ( -20.69976415826234373, 0.7537836665104515887, -27.44232068374074274 ) ) ;
#33602 = VERTEX_POINT ( 'NONE', #8011 ) ;
#33603 = CARTESIAN_POINT ( 'NONE',  ( 23.54702740617528178, -0.1080853855451005679, -20.45226996084934257 ) ) ;
#33604 = VECTOR ( 'NONE', #36687, 999.9999999999998863 ) ;
#33605 = CARTESIAN_POINT ( 'NONE',  ( 32.11924139737163841, -16.82817082614038995, 18.42518152272108622 ) ) ;
#33606 = EDGE_CURVE ( 'NONE', #9581, #18534, #32612, .T. ) ;
#33607 = ORIENTED_EDGE ( 'NONE', *, *, #10096, .T. ) ;
#33608 = CARTESIAN_POINT ( 'NONE',  ( -22.64987897201472933, 3.535174575633820204, -19.80251213055704440 ) ) ;
#33609 = DIRECTION ( 'NONE',  ( -1.000000000000000000, 0.000000000000000000, 0.000000000000000000 ) ) ;
#33610 = CARTESIAN_POINT ( 'NONE',  ( 2.594149110900703992, 26.80855565015188446, 20.99999999999999645 ) ) ;
#33611 = CARTESIAN_POINT ( 'NONE',  ( -15.00437666251167101, -28.61930095463374357, 12.14047268033097637 ) ) ;
#33612 = EDGE_CURVE ( 'NONE', #37387, #36832, #4894, .T. ) ;
#33613 = DIRECTION ( 'NONE',  ( 0.8090169943749504489, 0.5877852522924690293, -0.000000000000000000 ) ) ;
#33614 = EDGE_CURVE ( 'NONE', #5349, #10226, #26507, .T. ) ;
#33615 = B_SPLINE_CURVE_WITH_KNOTS ( 'NONE', 3,
 ( #36793, #8970, #21357, #36004, #20569, #2079 ),
 .UNSPECIFIED., .F., .F.,
 ( 4, 2, 4 ),
 ( 0.000000000000000000, 0.5000000000000000000, 1.000000000000000000 ),
 .UNSPECIFIED. ) ;
#33616 = CIRCLE ( 'NONE', #7642, 0.5000000000000004441 ) ;
#33617 = CIRCLE ( 'NONE', #25795, 1.000000000000000000 ) ;
#33618 = FACE_BOUND ( 'NONE', #40173, .T. ) ;
#33619 = DIRECTION ( 'NONE',  ( -0.7431448254773953543, -0.6691306063588570163, 0.000000000000000000 ) ) ;
#33620 = ORIENTED_EDGE ( 'NONE', *, *, #27200, .F. ) ;
#33621 = CARTESIAN_POINT ( 'NONE',  ( -23.68415675949719557, 7.936142738517225403, -9.861203543945475047 ) ) ;
#33622 = DIRECTION ( 'NONE',  ( 1.000000000000000000, 0.000000000000000000, 0.000000000000000000 ) ) ;
#33623 = DIRECTION ( 'NONE',  ( 1.000000000000000000, 0.000000000000000000, 0.000000000000000000 ) ) ;
#33624 = CARTESIAN_POINT ( 'NONE',  ( 23.74789423688137546, -24.71003432651541587, -10.27501004622590131 ) ) ;
#33625 = CIRCLE ( 'NONE', #39434, 1.000000000000000000 ) ;
#33626 = CYLINDRICAL_SURFACE ( 'NONE', #817, 6.000000000000003553 ) ;
#33627 = CARTESIAN_POINT ( 'NONE',  ( 15.34186426957387184, 27.04214388478009923, -5.000000000000000888 ) ) ;
#33628 = CIRCLE ( 'NONE', #9630, 0.5000000000000004441 ) ;
#33629 = CARTESIAN_POINT ( 'NONE',  ( -10.19059090746470098, -26.87498467587872142, 13.92931973828929770 ) ) ;
#33630 = EDGE_LOOP ( 'NONE', ( #15897, #28762, #23676, #35122 ) ) ;
#33631 = CARTESIAN_POINT ( 'NONE',  ( -16.18955875647491993, 22.24348330894682135, -9.768321104223245399 ) ) ;
#33632 = CARTESIAN_POINT ( 'NONE',  ( -26.01028601707387011, -6.099477938991039849, 20.69868183039782394 ) ) ;
#33633 = EDGE_CURVE ( 'NONE', #21531, #19894, #16769, .T. ) ;
#33634 = ADVANCED_FACE ( 'NONE', ( #38898 ), #38698, .T. ) ;
#33635 = FACE_OUTER_BOUND ( 'NONE', #27092, .T. ) ;
#33636 = CARTESIAN_POINT ( 'NONE',  ( 11.32363492297296759, 18.02741897415885930, -25.01640571929745605 ) ) ;
#33637 = ORIENTED_EDGE ( 'NONE', *, *, #34932, .F. ) ;
#33638 = CARTESIAN_POINT ( 'NONE',  ( -14.84898236231945745, 21.81673761604096384, 10.49999999999999822 ) ) ;
#33639 = EDGE_LOOP ( 'NONE', ( #10766, #17568, #11435, #24867 ) ) ;
#33641 = CARTESIAN_POINT ( 'NONE',  ( 7.468455364333220103, 29.89744377950669474, 10.50000000000000000 ) ) ;
#33640 = CARTESIAN_POINT ( 'NONE',  ( -15.37369053509020667, 26.93276585663874556, -5.473472025586896272 ) ) ;
#33642 = CARTESIAN_POINT ( 'NONE',  ( -15.16696621437007764, -26.16659013829510627, -8.764073972218964670 ) ) ;
#33643 = CYLINDRICAL_SURFACE ( 'NONE', #32866, 1.000000000000000000 ) ;
#33644 = CARTESIAN_POINT ( 'NONE',  ( -33.54211376200377259, -17.56714898150389104, -7.545851557378520980 ) ) ;
#33645 = CARTESIAN_POINT ( 'NONE',  ( -7.605472735516510596, -19.34647446169307727, -26.98872577642229587 ) ) ;
#33646 = CARTESIAN_POINT ( 'NONE',  ( 1.000000000000000000, 37.00000000000000711, 11.00000000000000000 ) ) ;
#33647 = CARTESIAN_POINT ( 'NONE',  ( 16.29902410653496148, 23.87181549541910641, -5.000000000000001776 ) ) ;
#33648 = VERTEX_POINT ( 'NONE', #35451 ) ;
#33649 = CARTESIAN_POINT ( 'NONE',  ( 24.29960814844372408, 7.334394940551312025, -8.871400124960164391 ) ) ;
#33650 = CARTESIAN_POINT ( 'NONE',  ( 1.871201846650637046, 31.30332840660451765, 13.00000000000000178 ) ) ;
#33651 = DIRECTION ( 'NONE',  ( -1.000000000000000000, 0.000000000000000000, 0.000000000000000000 ) ) ;
#33652 = FACE_OUTER_BOUND ( 'NONE', #38011, .T. ) ;
#33653 = ORIENTED_EDGE ( 'NONE', *, *, #31537, .T. ) ;
#33654 = CARTESIAN_POINT ( 'NONE',  ( -20.74261079067644786, -0.4953610022129137924, -27.36091918602213013 ) ) ;
#33655 = CARTESIAN_POINT ( 'NONE',  ( 30.92694434159519901, -0.1013669071028381469, -5.945198762247071222 ) ) ;
#33656 = AXIS2_PLACEMENT_3D ( 'NONE', #38069, #25873, #22625 ) ;
#33657 = DIRECTION ( 'NONE',  ( 1.000000000000000000, 0.000000000000000000, 0.000000000000000000 ) ) ;
#33658 = CARTESIAN_POINT ( 'NONE',  ( 25.52323811238489881, -15.66556294379320136, 20.82122704794079837 ) ) ;
#33659 = AXIS2_PLACEMENT_3D ( 'NONE', #23255, #38894, #17375 ) ;
#33660 = EDGE_CURVE ( 'NONE', #3751, #23354, #7608, .T. ) ;
#33661 = CARTESIAN_POINT ( 'NONE',  ( 19.79815887584821610, 19.84782313723624370, -13.42901749168597192 ) ) ;
#33663 = VECTOR ( 'NONE', #31630, 1000.000000000000000 ) ;
#33662 = CARTESIAN_POINT ( 'NONE',  ( -11.61016527260153808, 31.83082137946488643, 7.500000000000004441 ) ) ;
#33664 = VERTEX_POINT ( 'NONE', #16563 ) ;
#33665 = PLANE ( 'NONE',  #23634 ) ;
#33666 = CARTESIAN_POINT ( 'NONE',  ( 14.36830325120613594, 20.48707633493483371, 7.000000000000000000 ) ) ;
#33667 = CARTESIAN_POINT ( 'NONE',  ( -4.727507481117093846, 31.88885898370948269, 10.00000000000000000 ) ) ;
#33668 = CARTESIAN_POINT ( 'NONE',  ( 3.867670317776020994, 37.97392467330134735, -5.858600071952766442 ) ) ;
#33669 = CARTESIAN_POINT ( 'NONE',  ( -6.282361020112269046, 14.70372268239681546, 10.50000000000000178 ) ) ;
#33670 = CARTESIAN_POINT ( 'NONE',  ( 8.768078002822829120, 24.93711404285870969, 20.50957957746028981 ) ) ;
#33671 = DIRECTION ( 'NONE',  ( 1.000000000000000000, 0.000000000000000000, -0.000000000000000000 ) ) ;
#33672 = DIRECTION ( 'NONE',  ( 0.000000000000000000, 0.000000000000000000, 1.000000000000000000 ) ) ;
#33673 = DIRECTION ( 'NONE',  ( 1.000000000000000000, 0.000000000000000000, 0.000000000000000000 ) ) ;
#33674 = CARTESIAN_POINT ( 'NONE',  ( 14.23945615837883949, -31.58416516429907972, 0.000000000000000000 ) ) ;
#33675 = AXIS2_PLACEMENT_3D ( 'NONE', #29016, #29420, #13572 ) ;
#33676 = CARTESIAN_POINT ( 'NONE',  ( 11.27257766325769239, 20.01675547985872683, -21.50247975293300584 ) ) ;
#33677 = CARTESIAN_POINT ( 'NONE',  ( 0.5000000000000035527, 32.50000000000000000, 10.50000000000000178 ) ) ;
#33678 = AXIS2_PLACEMENT_3D ( 'NONE', #9991, #9797, #22177 ) ;
#33679 = VERTEX_POINT ( 'NONE', #920 ) ;
#33681 = DIRECTION ( 'NONE',  ( -0.1277282058445971258, 0.8064441531181095746, 0.5773502691896276184 ) ) ;
#33680 = CARTESIAN_POINT ( 'NONE',  ( -19.16847334494743649, 16.60965121416508339, -6.446626008538204111 ) ) ;
#33682 = CARTESIAN_POINT ( 'NONE',  ( -11.62435565298221185, 14.63397459621566910, 9.500000000000000000 ) ) ;
#33683 = CARTESIAN_POINT ( 'NONE',  ( 14.85648237307818498, -25.82965647359291950, -9.709266928100928951 ) ) ;
#33684 = EDGE_CURVE ( 'NONE', #31289, #6084, #13296, .T. ) ;
#33685 = CARTESIAN_POINT ( 'NONE',  ( -17.96239324037909668, -22.68179410725907275, -15.04167774667985569 ) ) ;
#33686 = FACE_OUTER_BOUND ( 'NONE', #685, .T. ) ;
#33687 = B_SPLINE_CURVE_WITH_KNOTS ( 'NONE', 3,
 ( #16533, #6767, #687, #25661, #16940, #13473 ),
 .UNSPECIFIED., .F., .F.,
 ( 4, 2, 4 ),
 ( 0.000000000000000000, 0.5000000000000000000, 1.000000000000000000 ),
 .UNSPECIFIED. ) ;
#33688 = CARTESIAN_POINT ( 'NONE',  ( 12.11672168374641956, 19.94100266206895711, -20.53805629048271797 ) ) ;
#33689 = ORIENTED_EDGE ( 'NONE', *, *, #8064, .T. ) ;
#33690 = LINE ( 'NONE', #12727, #10785 ) ;
#33691 = CARTESIAN_POINT ( 'NONE',  ( 34.33271598312541784, -24.82403719196558001, 11.00000000000000000 ) ) ;
#33692 = CARTESIAN_POINT ( 'NONE',  ( -20.97423577176458309, -16.41428094411201499, -18.66848081662921999 ) ) ;
#33693 = CARTESIAN_POINT ( 'NONE',  ( -0.3884064831159054210, -24.73345553465953017, -6.453633902575101722 ) ) ;
#33694 = CARTESIAN_POINT ( 'NONE',  ( 15.46285928058480152, 25.94289359300809750, -7.360000718803358488 ) ) ;
#33695 = CARTESIAN_POINT ( 'NONE',  ( 18.90977336216788629, 11.58301458159701092, -19.06584539304483528 ) ) ;
#33696 = DIRECTION ( 'NONE',  ( 0.000000000000000000, 0.000000000000000000, 1.000000000000000000 ) ) ;
#33697 = CARTESIAN_POINT ( 'NONE',  ( -3.891894238164187225, 27.44735175141750716, -17.64614778283444352 ) ) ;
#33698 = ORIENTED_EDGE ( 'NONE', *, *, #8552, .T. ) ;
#33699 = CARTESIAN_POINT ( 'NONE',  ( -32.83126665819848711, -6.129261575006776930, -10.33078432171702055 ) ) ;
#33700 = CARTESIAN_POINT ( 'NONE',  ( -31.72789954390187006, 0.7664678198892422856, 14.53008259254010959 ) ) ;
#33701 = ORIENTED_EDGE ( 'NONE', *, *, #26921, .T. ) ;
#33702 = CARTESIAN_POINT ( 'NONE',  ( 1.734965421685031872, 7.600674680189132282, 7.000000000000000000 ) ) ;
#33703 = LINE ( 'NONE', #9506, #8319 ) ;
#33704 = CARTESIAN_POINT ( 'NONE',  ( -29.22879574628063182, 0.6855083203516167956, -9.721972840624630408 ) ) ;
#33705 = EDGE_CURVE ( 'NONE', #5508, #7975, #4653, .T. ) ;
#33706 = CARTESIAN_POINT ( 'NONE',  ( 20.07302653732184439, -7.417995268840763323, -25.64353969630302998 ) ) ;
#33707 = CIRCLE ( 'NONE', #2552, 1.000000000000000000 ) ;
#33708 = AXIS2_PLACEMENT_3D ( 'NONE', #35719, #26971, #29613 ) ;
#33709 = EDGE_CURVE ( 'NONE', #29758, #29828, #26967, .T. ) ;
#33710 = EDGE_LOOP ( 'NONE', ( #22969, #39601, #34926 ) ) ;
#33711 = ADVANCED_FACE ( 'NONE', ( #30363 ), #31489, .T. ) ;
#33712 = CARTESIAN_POINT ( 'NONE',  ( 3.000488737323008248, 30.46850471149999962, 7.000000000000000000 ) ) ;
#33713 = ORIENTED_EDGE ( 'NONE', *, *, #8091, .T. ) ;
#33714 = AXIS2_PLACEMENT_3D ( 'NONE', #11620, #11813, #8562 ) ;
#33715 = DIRECTION ( 'NONE',  ( 0.000000000000000000, 0.000000000000000000, 1.000000000000000000 ) ) ;
#33716 = CARTESIAN_POINT ( 'NONE',  ( 6.658969205967948390, 35.40746193325453817, 10.66666666666666430 ) ) ;
#33717 = EDGE_CURVE ( 'NONE', #32632, #16758, #9457, .T. ) ;
#33718 = DIRECTION ( 'NONE',  ( -1.000000000000000000, 0.000000000000000000, 0.000000000000000000 ) ) ;
#33719 = ORIENTED_EDGE ( 'NONE', *, *, #24021, .T. ) ;
#33720 = CARTESIAN_POINT ( 'NONE',  ( -3.059748728390603745, 38.05383510088704213, -6.278958135869814328 ) ) ;
#33721 = CYLINDRICAL_SURFACE ( 'NONE', #5526, 0.5000000000000004441 ) ;
#33722 = FACE_OUTER_BOUND ( 'NONE', #24671, .T. ) ;
#33723 = CARTESIAN_POINT ( 'NONE',  ( 2.113538555224950155, 27.06402972250564432, 23.00000000000000355 ) ) ;
#33724 = CARTESIAN_POINT ( 'NONE',  ( 24.61464500862492244, -18.95959619293818577, -14.76315794208474053 ) ) ;
#33725 = CARTESIAN_POINT ( 'NONE',  ( 18.72885360190822368, 15.10340418431515097, -12.86103651079863930 ) ) ;
#33726 = CARTESIAN_POINT ( 'NONE',  ( 6.972563247160245226, 19.50015755702453291, -27.85944964339131857 ) ) ;
#33727 = ORIENTED_EDGE ( 'NONE', *, *, #22054, .F. ) ;
#33728 = CARTESIAN_POINT ( 'NONE',  ( -18.87236092649526142, 8.549343831987949116, -26.60993495225021732 ) ) ;
#33729 = DIRECTION ( 'NONE',  ( 0.8090169943749426773, -0.5877852522924797984, 0.000000000000000000 ) ) ;
#33730 = CARTESIAN_POINT ( 'NONE',  ( 14.16900449820494678, -24.63218968044553847, -12.54074064262510291 ) ) ;
#33731 = CARTESIAN_POINT ( 'NONE',  ( 13.46929972531963848, 26.35070966310165375, 10.00000000000000000 ) ) ;
#33732 = ADVANCED_FACE ( 'NONE', ( #14312 ), #36654, .F. ) ;
#33733 = ADVANCED_FACE ( 'NONE', ( #26704 ), #14917, .T. ) ;
#33734 = CARTESIAN_POINT ( 'NONE',  ( 12.05832241004688399, 18.99596958976722760, -30.00000000000000000 ) ) ;
#33735 = EDGE_CURVE ( 'NONE', #19392, #20347, #17382, .T. ) ;
#33737 = CIRCLE ( 'NONE', #16202, 0.5000000000000004441 ) ;
#33736 = CARTESIAN_POINT ( 'NONE',  ( -11.05339688301675594, 17.51568747190060904, -27.44627114179852256 ) ) ;
#33738 = CARTESIAN_POINT ( 'NONE',  ( -13.46176099346681809, -16.14434513549814909, -26.50464527480163213 ) ) ;
#33739 = CARTESIAN_POINT ( 'NONE',  ( 11.40532025035704677, -23.47631050763437344, -14.58224395303332699 ) ) ;
#33740 = DIRECTION ( 'NONE',  ( 0.000000000000000000, 0.000000000000000000, -1.000000000000000000 ) ) ;
#33741 = ORIENTED_EDGE ( 'NONE', *, *, #4115, .T. ) ;
#33742 = ORIENTED_EDGE ( 'NONE', *, *, #25374, .T. ) ;
#33743 = CIRCLE ( 'NONE', #36974, 1.000000000000000888 ) ;
#33744 = CARTESIAN_POINT ( 'NONE',  ( -6.672699392047024780, 22.34245898429709598, -22.09591057274325365 ) ) ;
#33745 = CARTESIAN_POINT ( 'NONE',  ( -13.64211604268330724, 20.79918788657763429, 13.00000000000000178 ) ) ;
#33746 = DIRECTION ( 'NONE',  ( 0.000000000000000000, 0.000000000000000000, 1.000000000000000000 ) ) ;
#33747 = CARTESIAN_POINT ( 'NONE',  ( -9.665073660138979506, 25.11464168560200605, 10.49999999999999112 ) ) ;
#33748 = ORIENTED_EDGE ( 'NONE', *, *, #12866, .T. ) ;
#33749 = CARTESIAN_POINT ( 'NONE',  ( 25.84101663196772947, 0.3562117509880242672, -16.44710462539339346 ) ) ;
#33750 = CARTESIAN_POINT ( 'NONE',  ( -13.94482798346716201, 26.50521816028930999, 7.499999999999993783 ) ) ;
#33751 = CARTESIAN_POINT ( 'NONE',  ( 19.48557158514982746, -11.25000000000009415, 0.000000000000000000 ) ) ;
#33752 = ORIENTED_EDGE ( 'NONE', *, *, #18311, .F. ) ;
#33753 = CARTESIAN_POINT ( 'NONE',  ( -20.52702548769616442, 0.8561983801584475140, -28.70691147235546836 ) ) ;
#33754 = DIRECTION ( 'NONE',  ( 0.000000000000000000, 0.000000000000000000, 1.000000000000000000 ) ) ;
#33755 = EDGE_CURVE ( 'NONE', #39268, #37780, #39886, .T. ) ;
#33756 = ORIENTED_EDGE ( 'NONE', *, *, #31121, .T. ) ;
#33757 = CARTESIAN_POINT ( 'NONE',  ( 29.73061004676158348, -5.254439166030093311, -14.04169227091120042 ) ) ;
#33758 = EDGE_CURVE ( 'NONE', #18974, #5349, #20820, .T. ) ;
#33759 = EDGE_LOOP ( 'NONE', ( #20316, #37385, #6961, #11189 ) ) ;
#33760 = CARTESIAN_POINT ( 'NONE',  ( -10.77072277543642187, 36.67279993932645255, 12.73282698324853079 ) ) ;
#33761 = CARTESIAN_POINT ( 'NONE',  ( -12.15426487966493596, -15.33773963145039332, 20.99999999999999645 ) ) ;
#33762 = DIRECTION ( 'NONE',  ( 0.000000000000000000, 0.000000000000000000, 1.000000000000000000 ) ) ;
#33763 = CARTESIAN_POINT ( 'NONE',  ( -8.084330871572442234, 26.79335594083840633, 20.50957957746031113 ) ) ;
#33764 = CIRCLE ( 'NONE', #3238, 1.000000000000002665 ) ;
#33765 = DIRECTION ( 'NONE',  ( 1.000000000000000000, 0.000000000000000000, 0.000000000000000000 ) ) ;
#33766 = EDGE_LOOP ( 'NONE', ( #28685, #3854, #22853, #36725, #13538 ) ) ;
#33767 = CARTESIAN_POINT ( 'NONE',  ( -14.97058623676949729, 26.66112013780927015, 16.87380292611441845 ) ) ;
#33768 = CARTESIAN_POINT ( 'NONE',  ( 3.503793317224326298, 8.420815634768676006, 9.500000000000000000 ) ) ;
#33769 = VECTOR ( 'NONE', #4359, 1000.000000000000000 ) ;
#33770 = CARTESIAN_POINT ( 'NONE',  ( 4.056192851408421340, 20.98781719672311397, -25.66352865187444365 ) ) ;
#33771 = DIRECTION ( 'NONE',  ( -1.000000000000000000, -1.224646799147351235E-16, 0.000000000000000000 ) ) ;
#33772 = CARTESIAN_POINT ( 'NONE',  ( 16.51452683366346363, -26.94346954434094243, -5.935747864356960335 ) ) ;
#33773 = CARTESIAN_POINT ( 'NONE',  ( 75.15099915297797395, 43.38844959084117647, 0.000000000000000000 ) ) ;
#33774 = DIRECTION ( 'NONE',  ( 0.5821182788257952545, 0.000000000000000000, 0.8131041196900269385 ) ) ;
#33775 = DIRECTION ( 'NONE',  ( 0.000000000000000000, -0.5906904945688840058, 0.8068982213550648375 ) ) ;
#33776 = ORIENTED_EDGE ( 'NONE', *, *, #38040, .F. ) ;
#33777 = CARTESIAN_POINT ( 'NONE',  ( -15.42498320908520704, 26.75103934920171511, -5.474196440071953162 ) ) ;
#33778 = AXIS2_PLACEMENT_3D ( 'NONE', #15308, #14715, #24650 ) ;
#33779 = CARTESIAN_POINT ( 'NONE',  ( -32.23453252384940271, -8.210301902002639096, 18.87996532025712071 ) ) ;
#33780 = CARTESIAN_POINT ( 'NONE',  ( 12.42243934462404553, -22.55512267161180517, -16.46144506859675261 ) ) ;
#33781 = CARTESIAN_POINT ( 'NONE',  ( 3.718716484603448613, 7.955328666817497840, 10.49999999999999822 ) ) ;
#33782 = EDGE_LOOP ( 'NONE', ( #23890, #2963, #37661, #5970 ) ) ;
#33783 = EDGE_LOOP ( 'NONE', ( #20015, #18277, #16727, #18081, #30076, #31362, #39652 ) ) ;
#33785 = CARTESIAN_POINT ( 'NONE',  ( 8.016213763118591018, 9.982035245863860595, 10.49999999999999822 ) ) ;
#33784 = CARTESIAN_POINT ( 'NONE',  ( -14.15606045317429462, 26.98637277077674312, -10.55315924151954121 ) ) ;
#33786 = CARTESIAN_POINT ( 'NONE',  ( -18.79972725875673234, -26.44331049119935173, -9.081311273665734873 ) ) ;
#33787 = SHAPE_REPRESENTATION ( 'Protective Beveled Outer Blade Guard', ( #24238 ), #27483 ) ;
#33788 = CARTESIAN_POINT ( 'NONE',  ( 18.68254918188133473, 8.687943646703843115, 9.500000000000000000 ) ) ;
#33789 = ORIENTED_EDGE ( 'NONE', *, *, #14642, .T. ) ;
#33790 = CARTESIAN_POINT ( 'NONE',  ( -20.21455581687538228, -6.984773374644928978, -25.66161433552150584 ) ) ;
#33791 = CARTESIAN_POINT ( 'NONE',  ( -14.53915841217452787, -25.76227397208802117, -9.714023261601081316 ) ) ;
#33792 = CARTESIAN_POINT ( 'NONE',  ( 33.75875814100313477, 2.759858869446413010, 23.00000000000000000 ) ) ;
#33793 = ORIENTED_EDGE ( 'NONE', *, *, #20072, .T. ) ;
#33794 = CARTESIAN_POINT ( 'NONE',  ( 30.59650344009811462, 0.1707353974115741191, -6.417298568035493034 ) ) ;
#33795 = DIRECTION ( 'NONE',  ( -0.3090169943749448977, 0.9510565162951543083, 0.000000000000000000 ) ) ;
#33796 = CARTESIAN_POINT ( 'NONE',  ( -19.23557158514982746, 34.18301270189230934, 11.00000000000000000 ) ) ;
#33797 = AXIS2_PLACEMENT_3D ( 'NONE', #3073, #25396, #31503 ) ;
#33798 = VERTEX_POINT ( 'NONE', #29951 ) ;
#33799 = CARTESIAN_POINT ( 'NONE',  ( -22.23634261291865855, 0.6022514368306863819, -22.72707163159650534 ) ) ;
#33800 = VERTEX_POINT ( 'NONE', #11868 ) ;
#33801 = CARTESIAN_POINT ( 'NONE',  ( 31.01104622761054230, -0.9322571436193676231, -8.717104344044161124 ) ) ;
#33802 = CARTESIAN_POINT ( 'NONE',  ( -1.247473515615844075, 16.63111439559750693, 6.000000000000000000 ) ) ;
#33803 = CARTESIAN_POINT ( 'NONE',  ( 23.78889779961332707, -25.69434382178437914, 17.42190598798433854 ) ) ;
#33804 = EDGE_LOOP ( 'NONE', ( #37327, #34391 ) ) ;
#33805 = CARTESIAN_POINT ( 'NONE',  ( -26.85005620991422859, 2.655769742037339398, -11.69190580713203964 ) ) ;
#33806 = CARTESIAN_POINT ( 'NONE',  ( 17.34253826539385201, 27.32041144647958575, -13.70816084473008800 ) ) ;
#33807 = CARTESIAN_POINT ( 'NONE',  ( 1.247466774197339978, 28.36888560440311480, 6.000000000000000000 ) ) ;
#33808 = AXIS2_PLACEMENT_3D ( 'NONE', #5318, #11816, #24203 ) ;
#33809 = CARTESIAN_POINT ( 'NONE',  ( -36.58707756785061349, -5.516531573120356136, 11.00000000000008527 ) ) ;
#33810 = AXIS2_PLACEMENT_3D ( 'NONE', #5821, #26754, #8674 ) ;
#33811 = DIRECTION ( 'NONE',  ( 0.6916548014802246236, -0.1470157664652213536, -0.7071067811865437980 ) ) ;
#33812 = FACE_BOUND ( 'NONE', #13307, .T. ) ;
#33813 = CARTESIAN_POINT ( 'NONE',  ( -5.203512939752292787, 36.56867331639969620, 7.338691926023215295 ) ) ;
#33814 = ORIENTED_EDGE ( 'NONE', *, *, #28478, .F. ) ;
#33815 = CARTESIAN_POINT ( 'NONE',  ( -21.57472102895474109, 6.664260218504890254, -18.95869221603280153 ) ) ;
#33816 = DIRECTION ( 'NONE',  ( 0.000000000000000000, 0.000000000000000000, 1.000000000000000000 ) ) ;
#33817 = CARTESIAN_POINT ( 'NONE',  ( 4.476901250629513385, 26.36149378532653031, 6.000000000000000000 ) ) ;
#33818 = CARTESIAN_POINT ( 'NONE',  ( 14.77033916382619694, -15.37368051247184120, -25.75951637363165148 ) ) ;
#33819 = TOROIDAL_SURFACE ( 'NONE', #1387, 1.000000000000000000, 0.5000000000000000000 ) ;
#33820 = DIRECTION ( 'NONE',  ( -0.000000000000000000, -0.000000000000000000, 1.000000000000000000 ) ) ;
#33821 = CARTESIAN_POINT ( 'NONE',  ( 15.32541171586220941, 27.00755533933892139, -5.943389983610922300 ) ) ;
#33822 = EDGE_LOOP ( 'NONE', ( #17975, #9779, #18103, #10343 ) ) ;
#33823 = CARTESIAN_POINT ( 'NONE',  ( -15.23324207282226261, 23.13468747206823650, -11.65450899073664814 ) ) ;
#33824 = CARTESIAN_POINT ( 'NONE',  ( -23.85459647502774416, -16.20858856896902367, 20.94377226548378346 ) ) ;
#33825 = EDGE_CURVE ( 'NONE', #9944, #9209, #19151, .T. ) ;
#33826 = DIRECTION ( 'NONE',  ( 0.9135454576426059736, 0.4067366430757887730, 0.000000000000000000 ) ) ;
#33827 = CARTESIAN_POINT ( 'NONE',  ( 14.30395659009414011, 24.43853900399440704, -12.55159526015550675 ) ) ;
#33828 = EDGE_LOOP ( 'NONE', ( #10232, #22989 ) ) ;
#33829 = CYLINDRICAL_SURFACE ( 'NONE', #19008, 18.00000000000001421 ) ;
#33830 = ORIENTED_EDGE ( 'NONE', *, *, #14464, .F. ) ;
#33832 = FACE_OUTER_BOUND ( 'NONE', #22862, .T. ) ;
#33831 = CARTESIAN_POINT ( 'NONE',  ( -10.97252080025042353, 17.71808212118776638, -26.81605910367778023 ) ) ;
#33833 = CARTESIAN_POINT ( 'NONE',  ( -9.580852559982135475, -18.12344168749379492, -29.34663924488240738 ) ) ;
#33834 = DIRECTION ( 'NONE',  ( 0.000000000000000000, 0.000000000000000000, 1.000000000000000000 ) ) ;
#33835 = CARTESIAN_POINT ( 'NONE',  ( -33.84414506509371989, -17.72909435222108598, -6.697593496457613149 ) ) ;
#33836 = CARTESIAN_POINT ( 'NONE',  ( -11.46491240625375951, -25.63296783226419251, -7.374722599587664185 ) ) ;
#33837 = LINE ( 'NONE', #33646, #18327 ) ;
#33838 = CARTESIAN_POINT ( 'NONE',  ( 12.11158980248019645, 16.54297856518634902, -30.00000000000000000 ) ) ;
#33839 = EDGE_CURVE ( 'NONE', #2968, #9588, #14513, .T. ) ;
#33840 = ORIENTED_EDGE ( 'NONE', *, *, #31342, .T. ) ;
#33841 = CARTESIAN_POINT ( 'NONE',  ( 19.44092958653124725, 6.613309545252517019, -28.84111800654028457 ) ) ;
#33842 = VECTOR ( 'NONE', #66, 1000.000000000000114 ) ;
#33843 = DIRECTION ( 'NONE',  ( 1.000000000000000000, 0.000000000000000000, 0.000000000000000000 ) ) ;
#33844 = DIRECTION ( 'NONE',  ( 0.2185080122244077161, -0.6724985119639543818, 0.7071067811865513475 ) ) ;
#33845 = EDGE_CURVE ( 'NONE', #39810, #30652, #11471, .T. ) ;
#33846 = PLANE ( 'NONE',  #6967 ) ;
#33847 = ORIENTED_EDGE ( 'NONE', *, *, #27248, .T. ) ;
#33848 = CARTESIAN_POINT ( 'NONE',  ( -31.38524255402332841, -1.184009006764249472, -8.242489630512061183 ) ) ;
#33849 = CARTESIAN_POINT ( 'NONE',  ( 20.97531576542675680, 0.7517682979586068903, -26.21993259525444842 ) ) ;
#33850 = CARTESIAN_POINT ( 'NONE',  ( 13.32151712420403555, 20.09434385051835648, 9.500000000000000000 ) ) ;
#33851 = CARTESIAN_POINT ( 'NONE',  ( 17.42101839920122686, -19.25229542401860527, 20.69868183039781684 ) ) ;
#33852 = VERTEX_POINT ( 'NONE', #8215 ) ;
#33853 = VECTOR ( 'NONE', #25182, 1000.000000000000114 ) ;
#33854 = CARTESIAN_POINT ( 'NONE',  ( 17.34253826539385201, 27.32041144647958575, -13.70816084473008800 ) ) ;
#33855 = DIRECTION ( 'NONE',  ( 0.4067366430758010964, 0.9135454576426005335, 0.000000000000000000 ) ) ;
#33856 = ORIENTED_EDGE ( 'NONE', *, *, #37498, .F. ) ;
#33857 = ADVANCED_FACE ( 'NONE', ( #24452 ), #8424, .F. ) ;
#33858 = DIRECTION ( 'NONE',  ( 0.4999999999999912292, -0.8660254037844437036, 0.000000000000000000 ) ) ;
#33859 = CIRCLE ( 'NONE', #22820, 18.00000000000000000 ) ;
#33860 = LINE ( 'NONE', #27551, #14935 ) ;
#33861 = FACE_OUTER_BOUND ( 'NONE', #28665, .T. ) ;
#33862 = CARTESIAN_POINT ( 'NONE',  ( 3.399496789611879066, 33.07784035496857200, -12.90587768247559275 ) ) ;
#33863 = LINE ( 'NONE', #22241, #13659 ) ;
#33864 = LINE ( 'NONE', #6015, #20064 ) ;
#33865 = LINE ( 'NONE', #18421, #16713 ) ;
#33866 = LINE ( 'NONE', #31401, #3454 ) ;
#33867 = CARTESIAN_POINT ( 'NONE',  ( -5.537946624085890335, 36.44027069998196566, 7.500000000000000888 ) ) ;
#33868 = CARTESIAN_POINT ( 'NONE',  ( 13.09714986319504781, 23.57938164331712372, -15.36463189380894612 ) ) ;
#33869 = CARTESIAN_POINT ( 'NONE',  ( -3.458872323573595864, 26.51478363815348160, 12.00000000000000000 ) ) ;
#33870 = ORIENTED_EDGE ( 'NONE', *, *, #33633, .F. ) ;
#33872 = DIRECTION ( 'NONE',  ( -1.000000000000000000, 0.000000000000000000, 0.000000000000000000 ) ) ;
#33871 = CARTESIAN_POINT ( 'NONE',  ( -18.64675247270446334, 17.55525769010250059, -7.410062710081297688 ) ) ;
#33873 = CARTESIAN_POINT ( 'NONE',  ( -9.762586613238248390, -29.39641002289260285, 11.00000000000000000 ) ) ;
#33874 = AXIS2_PLACEMENT_3D ( 'NONE', #22983, #38024, #16700 ) ;
#33875 = CARTESIAN_POINT ( 'NONE',  ( 11.54455564027605163, -20.97676539060953615, -19.49701577318683832 ) ) ;
#33876 = CARTESIAN_POINT ( 'NONE',  ( -13.59760052849660461, -18.39269962030116190, -22.34963271257799633 ) ) ;
#33877 = CARTESIAN_POINT ( 'NONE',  ( 24.20198940123850306, -6.620595927253059010, 20.94377226548378701 ) ) ;
#33878 = CARTESIAN_POINT ( 'NONE',  ( 15.22536027402585646, 26.43007570565260522, -7.826986632856818282 ) ) ;
#33879 = ORIENTED_EDGE ( 'NONE', *, *, #37381, .F. ) ;
#33880 = DIRECTION ( 'NONE',  ( -0.5877852522924791323, -0.8090169943749430104, 0.000000000000000000 ) ) ;
#33881 = EDGE_CURVE ( 'NONE', #40077, #9569, #33023, .T. ) ;
#33882 = CARTESIAN_POINT ( 'NONE',  ( -14.89343483659701661, -25.97116541732223283, -9.239377617673552479 ) ) ;
#33883 = CARTESIAN_POINT ( 'NONE',  ( -36.50335543116000991, -9.090109797570214312, 14.53008259254010959 ) ) ;
#33884 = CARTESIAN_POINT ( 'NONE',  ( -28.56121237968124049, -23.79504838712581360, -7.568206030601050571 ) ) ;
#33885 = CARTESIAN_POINT ( 'NONE',  ( 1.236634163872074366, -20.51914614933548719, -30.00000000000001066 ) ) ;
#33886 = CARTESIAN_POINT ( 'NONE',  ( 13.22294849863610722, 21.18001974898340478, -17.48564420674206943 ) ) ;
#33887 = CARTESIAN_POINT ( 'NONE',  ( 19.80460749329455084, 12.16438029996845493, -14.92251035621654331 ) ) ;
#33888 = LINE ( 'NONE', #9891, #5011 ) ;
#33889 = ADVANCED_FACE ( 'NONE', ( #5769 ), #26906, .T. ) ;
#33890 = CARTESIAN_POINT ( 'NONE',  ( -3.458130042104727409, 20.20612265101129168, -29.22679435874877996 ) ) ;
#33891 = ORIENTED_EDGE ( 'NONE', *, *, #25894, .F. ) ;
#33892 = CARTESIAN_POINT ( 'NONE',  ( -29.79436624158082481, -5.527400279271972749, -14.02904961299980791 ) ) ;
#33893 = CARTESIAN_POINT ( 'NONE',  ( -31.94006737154283471, 0.9747213384881107112, 13.92931973827808534 ) ) ;
#33894 = ORIENTED_EDGE ( 'NONE', *, *, #9465, .T. ) ;
#33895 = DIRECTION ( 'NONE',  ( 1.000000000000000000, 0.000000000000000000, 0.000000000000000000 ) ) ;
#33896 = DIRECTION ( 'NONE',  ( 0.000000000000000000, 0.000000000000000000, 1.000000000000000000 ) ) ;
#33897 = CARTESIAN_POINT ( 'NONE',  ( -22.62160857727931784, 0.9731345702083473714, -21.66193316938567293 ) ) ;
#33898 = CARTESIAN_POINT ( 'NONE',  ( 19.51071764920130391, -6.549296650950685361, -28.48338599449614605 ) ) ;
#33899 = EDGE_LOOP ( 'NONE', ( #2930, #13880, #33402, #38636 ) ) ;
#33900 = ADVANCED_FACE ( 'NONE', ( #8620 ), #30563, .F. ) ;
#33901 = AXIS2_PLACEMENT_3D ( 'NONE', #4095, #7336, #10401 ) ;
#33902 = CYLINDRICAL_SURFACE ( 'NONE', #34944, 0.5000000000000004441 ) ;
#33903 = ORIENTED_EDGE ( 'NONE', *, *, #35182, .T. ) ;
#33904 = EDGE_CURVE ( 'NONE', #8719, #14392, #40041, .T. ) ;
#33905 = CARTESIAN_POINT ( 'NONE',  ( 9.892954722048896699, 20.95745441963929068, 10.50000000000000355 ) ) ;
#33906 = FACE_OUTER_BOUND ( 'NONE', #15919, .T. ) ;
#33907 = CARTESIAN_POINT ( 'NONE',  ( -5.473344025737326923, 14.11593743010433499, 10.50000000000000000 ) ) ;
#33908 = ORIENTED_EDGE ( 'NONE', *, *, #992, .T. ) ;
#33909 = CARTESIAN_POINT ( 'NONE',  ( -2.908402701707879068, 35.88643271034062820, -10.18049541942522573 ) ) ;
#33910 = CARTESIAN_POINT ( 'NONE',  ( -3.666817917346822941, 8.455467583238350571, 10.83333333333333215 ) ) ;
#33911 = CARTESIAN_POINT ( 'NONE',  ( 4.096822963000107620, 8.035697679810645866, 10.49999999999999289 ) ) ;
#33912 = CARTESIAN_POINT ( 'NONE',  ( -8.118377661053486349, 10.47536095541708967, 11.00000000000000000 ) ) ;
#33913 = CARTESIAN_POINT ( 'NONE',  ( 29.86472888556171768, -22.97618816406824749, -7.129344454106402829 ) ) ;
#33914 = CARTESIAN_POINT ( 'NONE',  ( 16.23943293897244544, 12.53170227796935343, -29.42461426250243051 ) ) ;
#33915 = CARTESIAN_POINT ( 'NONE',  ( 8.203324777427138059, 19.12455918632797491, -27.23712529939752969 ) ) ;
#33916 = VERTEX_POINT ( 'NONE', #21801 ) ;
#33917 = CARTESIAN_POINT ( 'NONE',  ( -18.67511144159872316, 8.486512637698147898, -30.00000000000000000 ) ) ;
#33918 = CARTESIAN_POINT ( 'NONE',  ( 11.44134295108989186, 15.31698729810772797, 10.50000000000000000 ) ) ;
#33919 = CARTESIAN_POINT ( 'NONE',  ( 15.27392571247604103, -26.19117440705182176, -8.759444881256309046 ) ) ;
#33920 = CARTESIAN_POINT ( 'NONE',  ( -6.953812613386785912, 14.77701242934787906, 13.00000000000000178 ) ) ;
#33921 = CARTESIAN_POINT ( 'NONE',  ( 13.28992586503610340, -18.25382200079949513, -29.99999999999999289 ) ) ;
#33922 = ADVANCED_FACE ( 'NONE', ( #6356 ), #15913, .T. ) ;
#33923 = AXIS2_PLACEMENT_3D ( 'NONE', #27699, #18174, #40091 ) ;
#33924 = CARTESIAN_POINT ( 'NONE',  ( -12.63209216405648405, 21.08522415426002539, -18.44753828729430367 ) ) ;
#33925 = CARTESIAN_POINT ( 'NONE',  ( -21.98991108409586204, -24.65262130162854959, -11.21756587170641772 ) ) ;
#33926 = CARTESIAN_POINT ( 'NONE',  ( 8.648529717685608631, -19.31184748484744773, -25.15118541177943712 ) ) ;
#33927 = CARTESIAN_POINT ( 'NONE',  ( 11.28725060478870823, 31.99026972875169150, 10.94387467463331731 ) ) ;
#33928 = ORIENTED_EDGE ( 'NONE', *, *, #19463, .T. ) ;
#33929 = CARTESIAN_POINT ( 'NONE',  ( -6.648157636961573580, 19.96354927932426548, -26.46540010809100707 ) ) ;
#33930 = CARTESIAN_POINT ( 'NONE',  ( -3.992867117591420545, 8.524771480177605554, 11.00000000000000000 ) ) ;
#33931 = CARTESIAN_POINT ( 'NONE',  ( -8.412270287199726582, 10.07085245822961994, 10.49999999999999822 ) ) ;
#33932 = CARTESIAN_POINT ( 'NONE',  ( -9.381390373407009875, 11.27850996657559790, 10.49999999999999822 ) ) ;
#33933 = ORIENTED_EDGE ( 'NONE', *, *, #40180, .T. ) ;
#33934 = CARTESIAN_POINT ( 'NONE',  ( 30.78432895970654926, -0.02295136688160604593, -6.417004196556904461 ) ) ;
#33935 = CARTESIAN_POINT ( 'NONE',  ( 6.688300058587269170, 16.47782454277055564, 12.00000000000000000 ) ) ;
#33936 = DIRECTION ( 'NONE',  ( 0.5877852522924796874, 0.8090169943749426773, 0.000000000000000000 ) ) ;
#33937 = ORIENTED_EDGE ( 'NONE', *, *, #30624, .F. ) ;
#33938 = CARTESIAN_POINT ( 'NONE',  ( -30.84974397859977557, 0.01335361837341130647, -4.999999999999999112 ) ) ;
#33939 = CARTESIAN_POINT ( 'NONE',  ( 14.97009266215792778, 21.42933399866928568, 7.000000000000000000 ) ) ;
#33940 = AXIS2_PLACEMENT_3D ( 'NONE', #23714, #24112, #36113 ) ;
#33941 = ORIENTED_EDGE ( 'NONE', *, *, #27498, .F. ) ;
#33942 = CARTESIAN_POINT ( 'NONE',  ( 32.74085591134507212, -5.827811756920110220, -10.33996608089739055 ) ) ;
#33943 = ORIENTED_EDGE ( 'NONE', *, *, #18917, .F. ) ;
#33944 = CARTESIAN_POINT ( 'NONE',  ( 13.54525386577604351, 33.99767725470013602, 13.32518128616618469 ) ) ;
#33945 = CARTESIAN_POINT ( 'NONE',  ( -6.077490221915047286, -14.56650175400723946, 20.99999999999999645 ) ) ;
#33946 = LINE ( 'NONE', #37390, #32534 ) ;
#33947 = ADVANCED_FACE ( 'NONE', ( #9421 ), #22393, .F. ) ;
#33948 = CARTESIAN_POINT ( 'NONE',  ( -9.535956184589343465, 27.56440042312200589, 19.99202127657105166 ) ) ;
#33949 = CARTESIAN_POINT ( 'NONE',  ( 4.984135866956514782, 36.15314577889351000, 10.49999999999999467 ) ) ;
#33950 = EDGE_LOOP ( 'NONE', ( #33928, #37906 ) ) ;
#33951 =( LENGTH_UNIT ( ) NAMED_UNIT ( * ) SI_UNIT ( .MILLI., .METRE. ) );
#33952 = DIRECTION ( 'NONE',  ( 0.000000000000000000, 0.000000000000000000, 1.000000000000000000 ) ) ;
#33953 = AXIS2_PLACEMENT_3D ( 'NONE', #19366, #28510, #38055 ) ;
#33954 = DIRECTION ( 'NONE',  ( -0.4067366430758009299, -0.9135454576426005335, 0.000000000000000000 ) ) ;
#33955 = CARTESIAN_POINT ( 'NONE',  ( -6.811226782241547539, 35.33967249274200384, 7.500000000000000888 ) ) ;
#33956 = CARTESIAN_POINT ( 'NONE',  ( 9.852384739805275515, 34.25028444780376446, -8.049578315757582203 ) ) ;
#33957 = VECTOR ( 'NONE', #13801, 1000.000000000000000 ) ;
#33958 = PLANE ( 'NONE',  #34761 ) ;
#33959 = CARTESIAN_POINT ( 'NONE',  ( 17.59916522844583753, -27.17459308133313201, -5.000000000000004441 ) ) ;
#33960 = CARTESIAN_POINT ( 'NONE',  ( -4.724378136954611840, 12.76962061027129458, 6.000000000000000000 ) ) ;
#33961 = DIRECTION ( 'NONE',  ( 0.1045284632676415082, -0.9945218953682745111, 0.000000000000000000 ) ) ;
#33962 = FACE_OUTER_BOUND ( 'NONE', #5275, .T. ) ;
#33963 = EDGE_CURVE ( 'NONE', #21146, #11250, #13349, .T. ) ;
#33964 = AXIS2_PLACEMENT_3D ( 'NONE', #23465, #29958, #21021 ) ;
#33965 = ORIENTED_EDGE ( 'NONE', *, *, #33717, .F. ) ;
#33966 = CARTESIAN_POINT ( 'NONE',  ( -13.06770973401748215, 21.42831458027773550, -17.46073772354927556 ) ) ;
#33967 = AXIS2_PLACEMENT_3D ( 'NONE', #5423, #8060, #13958 ) ;
#33968 = CARTESIAN_POINT ( 'NONE',  ( -34.55475982899667287, -10.97206003969062849, 17.42190598798472934 ) ) ;
#33969 = CARTESIAN_POINT ( 'NONE',  ( 14.48426304913733986, -25.43374522747946287, -10.65622368699242628 ) ) ;
#33970 = ADVANCED_FACE ( 'NONE', ( #15517 ), #38245, .F. ) ;
#33971 = DIRECTION ( 'NONE',  ( 1.000000000000000000, 0.000000000000000000, 0.000000000000000000 ) ) ;
#33972 = ORIENTED_EDGE ( 'NONE', *, *, #39802, .F. ) ;
#33973 = ORIENTED_EDGE ( 'NONE', *, *, #450, .T. ) ;
#33974 = CARTESIAN_POINT ( 'NONE',  ( -14.00751334334244191, 28.57779656496513354, -9.118724234240687565 ) ) ;
#33975 = CARTESIAN_POINT ( 'NONE',  ( -11.86207838096284917, -17.26656891588605447, -26.63928184976938951 ) ) ;
#33976 = DIRECTION ( 'NONE',  ( -0.7032331762534065334, 0.07391278520356939219, -0.7071067811865449082 ) ) ;
#33977 = AXIS2_PLACEMENT_3D ( 'NONE', #1785, #30216, #26964 ) ;
#33978 = VERTEX_POINT ( 'NONE', #18520 ) ;
#33979 = EDGE_CURVE ( 'NONE', #6485, #30397, #15305, .T. ) ;
#33980 = CARTESIAN_POINT ( 'NONE',  ( -35.33786424633182577, -8.799366064169335644, -5.444321735654653160 ) ) ;
#33981 = CARTESIAN_POINT ( 'NONE',  ( -9.365571907152105524, -18.46390408244730708, -27.46573865726494290 ) ) ;
#33982 = CARTESIAN_POINT ( 'NONE',  ( -5.348113209407908464, 9.835177808069893501, 12.00000000000000000 ) ) ;
#33983 = VERTEX_POINT ( 'NONE', #12219 ) ;
#33984 = CARTESIAN_POINT ( 'NONE',  ( 29.58057729095054000, 0.2898696450949133085, -9.714030781592626340 ) ) ;
#33985 = CARTESIAN_POINT ( 'NONE',  ( 9.331903152615748098, 11.35703883385568780, 10.49999999999999645 ) ) ;
#33986 = DIRECTION ( 'NONE',  ( 0.000000000000000000, 0.000000000000000000, -1.000000000000000000 ) ) ;
#33987 = EDGE_LOOP ( 'NONE', ( #7192, #17538, #36361, #8557 ) ) ;
#33988 = CARTESIAN_POINT ( 'NONE',  ( -20.61180082990850693, 0.8259781403983986747, -28.07628969275633324 ) ) ;
#33989 = EDGE_LOOP ( 'NONE', ( #11433, #36961, #37330, #22224 ) ) ;
#33990 = CARTESIAN_POINT ( 'NONE',  ( 25.99411550134611559, -1.208840217080102031, -17.24439678332520742 ) ) ;
#33991 =( REPRESENTATION_RELATIONSHIP ('NONE','NONE', #15382, #28068 ) REPRESENTATION_RELATIONSHIP_WITH_TRANSFORMATION ( #23951 )SHAPE_REPRESENTATION_RELATIONSHIP( ) );
#33992 = VECTOR ( 'NONE', #21305, 1000.000000000000114 ) ;
#33993 = CARTESIAN_POINT ( 'NONE',  ( -19.48557158514998022, -11.24999999999982414, 3.000000000000000000 ) ) ;
#33994 = CARTESIAN_POINT ( 'NONE',  ( 18.97485329855508240, -25.68201384536907383, 17.92354375535252942 ) ) ;
#33995 = VERTEX_POINT ( 'NONE', #27857 ) ;
#33996 = CARTESIAN_POINT ( 'NONE',  ( -20.27181835515031949, 3.600595787728656738, -28.19117047517736196 ) ) ;
#33997 = EDGE_CURVE ( 'NONE', #4123, #6233, #7085, .T. ) ;
#33998 = CARTESIAN_POINT ( 'NONE',  ( -5.982165713378357452, 28.55918256678905465, 9.000000000000001776 ) ) ;
#33999 = EDGE_CURVE ( 'NONE', #4629, #22450, #34703, .T. ) ;
#34000 = CARTESIAN_POINT ( 'NONE',  ( -1.000000000000000000, 37.00000000000000711, 7.500000000000000888 ) ) ;
#34001 = CYLINDRICAL_SURFACE ( 'NONE', #23954, 1.000000000000000888 ) ;
#34002 = CARTESIAN_POINT ( 'NONE',  ( 8.806975420853749625, 31.15003855377755571, 13.00000000000000178 ) ) ;
#34003 = B_SPLINE_SURFACE_WITH_KNOTS ( 'NONE', 1, 3, ( 
 ( #28558, #37899, #17336, #10073, #29711, #7009, #32976, #28353, #533, #23217 ),
 ( #12917, #9871, #30116, #8778, #39251, #8383, #27066, #24616, #26862, #11432 ) ),
 .UNSPECIFIED., .F., .F., .F.,
 ( 2, 2 ),
 ( 4, 2, 2, 2, 4 ),
 ( 0.000000000000000000, 1.000000000000000000 ),
 ( 4.563205465131974670, 4.955904546830696589, 5.348603628529417620, 5.741302710228138650, 6.134001791926860570 ),
 .UNSPECIFIED. ) ;
#34004 = VECTOR ( 'NONE', #18820, 1000.000000000000000 ) ;
#34005 = FACE_OUTER_BOUND ( 'NONE', #7077, .T. ) ;
#34006 = AXIS2_PLACEMENT_3D ( 'NONE', #5568, #29555, #5371 ) ;
#34007 = CARTESIAN_POINT ( 'NONE',  ( 28.36971490933128948, 4.612181732476346774, 13.92931973828039638 ) ) ;
#34008 = ORIENTED_EDGE ( 'NONE', *, *, #27998, .T. ) ;
#34009 = CARTESIAN_POINT ( 'NONE',  ( -22.69837051162585695, 7.744818927720608315, -13.85387379231857352 ) ) ;
#34010 = DIRECTION ( 'NONE',  ( -0.7431448254773961315, -0.6691306063588561281, 0.000000000000000000 ) ) ;
#34011 = DIRECTION ( 'NONE',  ( -0.000000000000000000, -0.000000000000000000, -1.000000000000000000 ) ) ;
#34012 = CARTESIAN_POINT ( 'NONE',  ( 23.81893702819105485, -26.18960064386696729, -7.628968477593851105 ) ) ;
#34013 = CARTESIAN_POINT ( 'NONE',  ( -9.917741276437942233, 30.52956727630665057, 12.00000000000000000 ) ) ;
#34014 = EDGE_CURVE ( 'NONE', #9003, #39013, #12415, .T. ) ;
#34015 = CARTESIAN_POINT ( 'NONE',  ( 10.77342450413916630, 17.44087877699069367, -30.00000000000000000 ) ) ;
#34016 = ORIENTED_EDGE ( 'NONE', *, *, #30713, .F. ) ;
#34017 = CARTESIAN_POINT ( 'NONE',  ( -16.03826714829968125, 24.67705000163143580, -5.000000000000000000 ) ) ;
#34018 = CARTESIAN_POINT ( 'NONE',  ( -28.21258359973651508, -14.01198379553961537, 20.50957957746028626 ) ) ;
#34019 = ADVANCED_FACE ( 'NONE', ( #31853 ), #2982, .T. ) ;
#34020 = CARTESIAN_POINT ( 'NONE',  ( -0.6057027746881266106, 27.44183462127829642, 13.00000000000000178 ) ) ;
#34021 = CARTESIAN_POINT ( 'NONE',  ( 15.03218564788412515, 25.92419391550620844, -9.238870818048370737 ) ) ;
#34022 = EDGE_LOOP ( 'NONE', ( #15592, #21984, #26839, #2191 ) ) ;
#34023 = CARTESIAN_POINT ( 'NONE',  ( 12.39463915635820612, 18.33192650902018883, 13.00000000000000178 ) ) ;
#34024 = VERTEX_POINT ( 'NONE', #19457 ) ;
#34026 = CARTESIAN_POINT ( 'NONE',  ( 13.30736791475921699, 15.68301270237638967, 10.49999999999999822 ) ) ;
#34025 = CARTESIAN_POINT ( 'NONE',  ( -13.10376629299052098, 22.42928523344748726, -16.41988283430683282 ) ) ;
#34027 = CARTESIAN_POINT ( 'NONE',  ( -9.543759016413366325, -18.14299990126706419, -30.00000000000000000 ) ) ;
#34028 = DIRECTION ( 'NONE',  ( 1.000000000000000000, 0.000000000000000000, 0.000000000000000000 ) ) ;
#34029 = ORIENTED_EDGE ( 'NONE', *, *, #29059, .T. ) ;
#34030 = CARTESIAN_POINT ( 'NONE',  ( -34.32242099319713446, -16.67052798041778772, -6.699077853923277814 ) ) ;
#34031 = AXIS2_PLACEMENT_3D ( 'NONE', #9725, #8567, #20967 ) ;
#34032 = CARTESIAN_POINT ( 'NONE',  ( -12.95816149891683011, -24.84176018504629369, -11.63896638183241983 ) ) ;
#34033 = FACE_OUTER_BOUND ( 'NONE', #8780, .T. ) ;
#34034 = CARTESIAN_POINT ( 'NONE',  ( 16.09876026818504968, 24.41207849431964405, -5.947509210907390376 ) ) ;
#34035 = EDGE_LOOP ( 'NONE', ( #4881, #23467 ) ) ;
#34036 = CARTESIAN_POINT ( 'NONE',  ( 20.29178992508080626, 5.227586473962275271, -25.37103639584170622 ) ) ;
#34037 = DIRECTION ( 'NONE',  ( 0.9510565162951544194, 0.3090169943749450643, 0.000000000000000000 ) ) ;
#34038 = CARTESIAN_POINT ( 'NONE',  ( -13.24038105676664401, 15.43301270189234486, 10.49999999999999822 ) ) ;
#34039 = CARTESIAN_POINT ( 'NONE',  ( -18.54826649988357090, -24.72227203017434150, -12.26027863146039820 ) ) ;
#34040 = ORIENTED_EDGE ( 'NONE', *, *, #7128, .F. ) ;
#34041 = CARTESIAN_POINT ( 'NONE',  ( -28.92430414141464468, -0.6002475978605696927, -12.47730999436802790 ) ) ;
#34042 = CARTESIAN_POINT ( 'NONE',  ( 20.49022872340270851, 0.6388713974194968337, -29.34434107258899971 ) ) ;
#34043 = CARTESIAN_POINT ( 'NONE',  ( -29.22587408525591712, -28.78382723770691243, 11.00000000000000000 ) ) ;
#34044 = CARTESIAN_POINT ( 'NONE',  ( 26.76156665933390499, -9.514918190647627227, 20.82122704794079837 ) ) ;
#34045 = ORIENTED_EDGE ( 'NONE', *, *, #29264, .T. ) ;
#34046 = CARTESIAN_POINT ( 'NONE',  ( 19.54664213359407654, -11.28525909758385914, -30.00000000000003908 ) ) ;
#34047 = CARTESIAN_POINT ( 'NONE',  ( 0.6666666666666681840, 37.00000000000000711, 10.83333333333333215 ) ) ;
#34048 = VECTOR ( 'NONE', #915, 1000.000000000000114 ) ;
#34049 = ORIENTED_EDGE ( 'NONE', *, *, #32821, .F. ) ;
#34050 = EDGE_CURVE ( 'NONE', #30652, #21181, #35104, .T. ) ;
#34051 = DIRECTION ( 'NONE',  ( -0.3090169943749465631, 0.9510565162951538642, 0.000000000000000000 ) ) ;
#34052 = FACE_OUTER_BOUND ( 'NONE', #2938, .T. ) ;
#34053 = DIRECTION ( 'NONE',  ( -1.000000000000000000, 0.000000000000000000, 0.000000000000000000 ) ) ;
#34054 = CARTESIAN_POINT ( 'NONE',  ( 2.387565118073518011, 23.58149098553560563, -21.87002398248182899 ) ) ;
#34055 = PLANE ( 'NONE',  #17903 ) ;
#34056 = CARTESIAN_POINT ( 'NONE',  ( 14.46041492111391236, 20.47739500831021076, 10.99387789255783687 ) ) ;
#34057 = DIRECTION ( 'NONE',  ( 0.000000000000000000, 0.000000000000000000, -1.000000000000000000 ) ) ;
#34058 = CARTESIAN_POINT ( 'NONE',  ( -4.476907992048016816, 18.63850621467409496, 12.00000000000000000 ) ) ;
#34059 = CARTESIAN_POINT ( 'NONE',  ( -8.007761790012255076, 9.776959832083379709, 10.50000000000000000 ) ) ;
#34060 = CARTESIAN_POINT ( 'NONE',  ( -0.6057027746881266106, 27.44183462127829642, 6.000000000000000000 ) ) ;
#34061 = VECTOR ( 'NONE', #26367, 1000.000000000000000 ) ;
#34062 = CARTESIAN_POINT ( 'NONE',  ( 14.69102536304534112, 26.94039611839157899, -9.191466769791299285 ) ) ;
#34063 = DIRECTION ( 'NONE',  ( 0.4999999999999930056, -0.8660254037844428154, 0.000000000000000000 ) ) ;
#34064 = VERTEX_POINT ( 'NONE', #21559 ) ;
#34066 = CARTESIAN_POINT ( 'NONE',  ( 12.14070168820766149, 14.52831216351291133, 10.66666666666666430 ) ) ;
#34065 = CARTESIAN_POINT ( 'NONE',  ( -15.31736683468135141, 14.60021943509330100, -24.29952530214165662 ) ) ;
#34067 = CARTESIAN_POINT ( 'NONE',  ( -3.853172919594720192, 21.57294901687549427, 6.000000000000000000 ) ) ;
#34068 = CARTESIAN_POINT ( 'NONE',  ( 11.55613727932546730, -20.97541504343049823, -19.49553383130734474 ) ) ;
#34069 = CARTESIAN_POINT ( 'NONE',  ( -12.75218288797893074, -16.30376047647427029, -27.89448312604282165 ) ) ;
#34070 = CARTESIAN_POINT ( 'NONE',  ( 19.48557158514988075, -11.24999999999998224, 6.000000000000000000 ) ) ;
#34071 = CARTESIAN_POINT ( 'NONE',  ( 15.33017556631518552, 26.64601132140138517, -6.887373872617191140 ) ) ;
#34072 = ORIENTED_EDGE ( 'NONE', *, *, #14187, .T. ) ;
#34073 = AXIS2_PLACEMENT_3D ( 'NONE', #24910, #10070, #27956 ) ;
#34074 = CARTESIAN_POINT ( 'NONE',  ( -3.992867117591420545, 8.524771480177605554, 10.50000000000000533 ) ) ;
#34075 = CARTESIAN_POINT ( 'NONE',  ( -13.94116916282742302, -24.59632506325680978, -12.55420017537907817 ) ) ;
#34076 = CARTESIAN_POINT ( 'NONE',  ( -26.00889624226697805, -26.79364542773710767, 15.13084544680213561 ) ) ;
#34077 = AXIS2_PLACEMENT_3D ( 'NONE', #14011, #6064, #2625 ) ;
#34078 = CARTESIAN_POINT ( 'NONE',  ( -16.53721940376430055, -12.13086247549455443, -30.00000000000000355 ) ) ;
#34079 = CARTESIAN_POINT ( 'NONE',  ( -2.588656999911660428, -24.74688003723862195, -6.453009911337188598 ) ) ;
#34080 = CARTESIAN_POINT ( 'NONE',  ( 11.35289046387891609, 17.31125046002085099, -27.46915152833578233 ) ) ;
#34081 = CARTESIAN_POINT ( 'NONE',  ( 21.45236543604948309, 10.76621870831805339, -11.87856902876374576 ) ) ;
#34082 = DIRECTION ( 'NONE',  ( -0.000000000000000000, -0.000000000000000000, -1.000000000000000000 ) ) ;
#34083 = EDGE_CURVE ( 'NONE', #25600, #19954, #23099, .T. ) ;
#34084 = CARTESIAN_POINT ( 'NONE',  ( -4.502816615928998623, 26.15216069617400763, -18.69540600892100812 ) ) ;
#34085 = ORIENTED_EDGE ( 'NONE', *, *, #28381, .T. ) ;
#34086 = CARTESIAN_POINT ( 'NONE',  ( -22.76661381573873300, -4.191030258134940567, -22.19333013853839986 ) ) ;
#34087 = CARTESIAN_POINT ( 'NONE',  ( -20.66414367076832903, 17.76245163069107491, 10.99999999999809219 ) ) ;
#34088 = ORIENTED_EDGE ( 'NONE', *, *, #35457, .F. ) ;
#34089 = DIRECTION ( 'NONE',  ( 1.000000000000000000, 0.000000000000000000, 0.000000000000000000 ) ) ;
#34090 = CARTESIAN_POINT ( 'NONE',  ( 5.167086843766644400, 44.40436517110171621, 11.00000000000000000 ) ) ;
#34091 = CARTESIAN_POINT ( 'NONE',  ( -20.58891407026878895, 1.184266961143116470, -28.09387474696538689 ) ) ;
#34092 = CARTESIAN_POINT ( 'NONE',  ( 35.19885548643981821, -12.96001660873345251, -6.713464945328998290 ) ) ;
#34093 = VECTOR ( 'NONE', #33139, 1000.000000000000000 ) ;
#34094 = EDGE_CURVE ( 'NONE', #28626, #26207, #38005, .T. ) ;
#34095 = ORIENTED_EDGE ( 'NONE', *, *, #3274, .F. ) ;
#34096 = CYLINDRICAL_SURFACE ( 'NONE', #6397, 6.000000000000008882 ) ;
#34097 = ORIENTED_EDGE ( 'NONE', *, *, #38799, .F. ) ;
#34098 = DIRECTION ( 'NONE',  ( -1.000000000000000000, 0.000000000000000000, 0.000000000000000000 ) ) ;
#34099 = CIRCLE ( 'NONE', #37977, 15.00000000000000000 ) ;
#34100 = CARTESIAN_POINT ( 'NONE',  ( -2.525645716490710679, 8.212903943950959018, 7.000000000000000000 ) ) ;
#34101 = VECTOR ( 'NONE', #37100, 1000.000000000000000 ) ;
#34102 = AXIS2_PLACEMENT_3D ( 'NONE', #27625, #2058, #12386 ) ;
#34103 = FACE_OUTER_BOUND ( 'NONE', #16693, .T. ) ;
#34104 = ORIENTED_EDGE ( 'NONE', *, *, #34105, .T. ) ;
#34105 = EDGE_CURVE ( 'NONE', #31246, #33136, #4222, .T. ) ;
#34106 = CARTESIAN_POINT ( 'NONE',  ( -1.922249852543706616, 38.37524763245696846, -5.856172595693201366 ) ) ;
#34107 = CARTESIAN_POINT ( 'NONE',  ( -32.35383858704948778, -1.519079388896815930, -4.999999999999999112 ) ) ;
#34108 = CARTESIAN_POINT ( 'NONE',  ( 8.935770203493859754, 22.34671014717335780, 6.000000000000000000 ) ) ;
#34109 = EDGE_CURVE ( 'NONE', #37387, #21382, #26327, .T. ) ;
#34110 = DIRECTION ( 'NONE',  ( 0.000000000000000000, 0.000000000000000000, 1.000000000000000000 ) ) ;
#34111 = CARTESIAN_POINT ( 'NONE',  ( 23.89493199558969039, -19.57224858292615366, -14.78313763251888879 ) ) ;
#34112 = CARTESIAN_POINT ( 'NONE',  ( 20.04635827611367205, 14.95022894506133859, -4.999999999999998224 ) ) ;
#34113 = CARTESIAN_POINT ( 'NONE',  ( 13.65686006951314369, 30.58359301831817589, -6.811602640649293328 ) ) ;
#34114 = ORIENTED_EDGE ( 'NONE', *, *, #17474, .F. ) ;
#34115 = CARTESIAN_POINT ( 'NONE',  ( -20.47881545949457660, 13.50965256804138370, -8.899456932346438975 ) ) ;
#34116 = CARTESIAN_POINT ( 'NONE',  ( 19.26948696230205371, 27.85601271560038938, 22.99999999999999289 ) ) ;
#34117 = CARTESIAN_POINT ( 'NONE',  ( 15.66152395236884054, -26.76027550630084662, -5.944054962524266905 ) ) ;
#34118 = DIRECTION ( 'NONE',  ( -0.000000000000000000, -0.000000000000000000, -1.000000000000000000 ) ) ;
#34119 = CARTESIAN_POINT ( 'NONE',  ( 20.55563217186196212, -29.52600041847795254, -13.99876745781546994 ) ) ;
#34120 = DIRECTION ( 'NONE',  ( -0.9781476007338042455, 0.2079116908177663647, -0.000000000000000000 ) ) ;
#34121 = CARTESIAN_POINT ( 'NONE',  ( -14.01594577761574101, 23.96872618684867007, -13.51011200901672105 ) ) ;
#34122 = CARTESIAN_POINT ( 'NONE',  ( -20.99987834568138823, -24.96315251019730397, -11.24918557064901847 ) ) ;
#34123 = CARTESIAN_POINT ( 'NONE',  ( 9.433270209358736835, -23.35418427748271242, -14.68531594918982819 ) ) ;
#34124 = EDGE_CURVE ( 'NONE', #3294, #6531, #31655, .T. ) ;
#34125 = EDGE_CURVE ( 'NONE', #33096, #648, #13363, .T. ) ;
#34126 = CARTESIAN_POINT ( 'NONE',  ( 11.11016527260166953, 31.83082137946472656, 11.00000000000000000 ) ) ;
#34127 = ADVANCED_FACE ( 'NONE', ( #21365 ), #24806, .T. ) ;
#34128 = VERTEX_POINT ( 'NONE', #8975 ) ;
#34129 = CARTESIAN_POINT ( 'NONE',  ( -10.29501812418428308, 34.74514102979851060, -5.879665602947800274 ) ) ;
#34130 = AXIS2_PLACEMENT_3D ( 'NONE', #39659, #8986, #2690 ) ;
#34131 = DIRECTION ( 'NONE',  ( 0.000000000000000000, 0.000000000000000000, 1.000000000000000000 ) ) ;
#34132 = DIRECTION ( 'NONE',  ( 1.000000000000000000, 0.000000000000000000, 0.000000000000000000 ) ) ;
#34133 = AXIS2_PLACEMENT_3D ( 'NONE', #30910, #4015, #28805 ) ;
#34134 = AXIS2_PLACEMENT_3D ( 'NONE', #21475, #24720, #27573 ) ;
#34135 = CARTESIAN_POINT ( 'NONE',  ( -9.126688212161006675, 10.78884215935646829, 10.87262190629280134 ) ) ;
#34136 = ORIENTED_EDGE ( 'NONE', *, *, #37633, .F. ) ;
#34137 = CARTESIAN_POINT ( 'NONE',  ( 30.31434325333418300, 0.03612907296712006971, -8.298080414836505270 ) ) ;
#34138 = CARTESIAN_POINT ( 'NONE',  ( 6.749995343096087730, 37.10960504752365807, -5.000000000000000888 ) ) ;
#34139 = AXIS2_PLACEMENT_3D ( 'NONE', #19260, #13161, #25554 ) ;
#34140 = CARTESIAN_POINT ( 'NONE',  ( -12.64211604268330724, 20.79918788657763429, 6.000000000000000000 ) ) ;
#34141 = ORIENTED_EDGE ( 'NONE', *, *, #11500, .F. ) ;
#34142 = CARTESIAN_POINT ( 'NONE',  ( -20.81343797531129880, 0.8557099860676852243, -26.83253627507455974 ) ) ;
#34143 = CARTESIAN_POINT ( 'NONE',  ( 12.19134295108989718, 16.61602540378438775, 10.50000000000000000 ) ) ;
#34144 = ORIENTED_EDGE ( 'NONE', *, *, #14106, .T. ) ;
#34145 = CARTESIAN_POINT ( 'NONE',  ( 34.51621760006609207, -7.217447013052957772, -7.634130922725350210 ) ) ;
#34146 = EDGE_LOOP ( 'NONE', ( #13241, #8704, #32851 ) ) ;
#34147 = CARTESIAN_POINT ( 'NONE',  ( -17.15083734909590163, 27.26712758905546252, 12.73282698324853257 ) ) ;
#34148 = CARTESIAN_POINT ( 'NONE',  ( -1.871208588069141143, 13.69667159339610762, 6.000000000000000000 ) ) ;
#34149 = CARTESIAN_POINT ( 'NONE',  ( 0.5000000000000012212, 31.00000000000000355, 7.000000000000000000 ) ) ;
#34150 = ADVANCED_FACE ( 'NONE', ( #9173 ), #33958, .F. ) ;
#34151 = CARTESIAN_POINT ( 'NONE',  ( -8.129960429723110135E-14, 32.41755745572908864, 20.25080042701565830 ) ) ;
#34152 = CARTESIAN_POINT ( 'NONE',  ( 2.525645716490518833, 8.212903943950921715, 7.000000000000000000 ) ) ;
#34153 = EDGE_LOOP ( 'NONE', ( #36436, #6675, #2479, #17359 ) ) ;
#34154 = CARTESIAN_POINT ( 'NONE',  ( 1.872892888448897120, -2.256054360071899634, 7.000000000000000000 ) ) ;
#34155 = CARTESIAN_POINT ( 'NONE',  ( 9.183240348400453001, 28.21559575157615996, 12.00000000000000000 ) ) ;
#34156 = CARTESIAN_POINT ( 'NONE',  ( 6.151085731882510288, 35.08626808545850650, 7.500000000000000000 ) ) ;
#34157 = B_SPLINE_CURVE_WITH_KNOTS ( 'NONE', 3,
 ( #8318, #17477, #27396, #14208, #20720, #21306 ),
 .UNSPECIFIED., .F., .F.,
 ( 4, 2, 4 ),
 ( 0.000000000000000000, 0.5000000000000000000, 1.000000000000000000 ),
 .UNSPECIFIED. ) ;
#34158 = AXIS2_PLACEMENT_3D ( 'NONE', #11984, #27619, #11591 ) ;
#34159 = CARTESIAN_POINT ( 'NONE',  ( 12.74038105676654453, 14.56698729810772264, 10.49999999999999822 ) ) ;
#34160 = CARTESIAN_POINT ( 'NONE',  ( 5.122947202949493573, 19.93899402170990953, -28.50457462493328720 ) ) ;
#34161 = AXIS2_PLACEMENT_3D ( 'NONE', #21621, #18780, #31366 ) ;
#34162 = CIRCLE ( 'NONE', #12747, 18.00000000000000000 ) ;
#34163 = CARTESIAN_POINT ( 'NONE',  ( 17.59916522844583753, -27.17459308133313201, -5.464832681431312622 ) ) ;
#34164 =( NAMED_UNIT ( * ) SI_UNIT ( $, .STERADIAN. ) SOLID_ANGLE_UNIT ( ) );
#34165 = CYLINDRICAL_SURFACE ( 'NONE', #38141, 1.000000000000000000 ) ;
#34166 = VERTEX_POINT ( 'NONE', #12019 ) ;
#34167 = CARTESIAN_POINT ( 'NONE',  ( -12.04642914189274094, 19.21860882176112639, -21.64378893228296619 ) ) ;
#34168 = CARTESIAN_POINT ( 'NONE',  ( -25.28418022016644429, -25.06680681775936037, 17.42190598798392998 ) ) ;
#34169 = CARTESIAN_POINT ( 'NONE',  ( 14.61363033921321986, -25.62685285069673924, -10.18295734475554681 ) ) ;
#34170 = CYLINDRICAL_SURFACE ( 'NONE', #10106, 1.000000000000000000 ) ;
#34171 = EDGE_CURVE ( 'NONE', #751, #28389, #5919, .T. ) ;
#34172 = VERTEX_POINT ( 'NONE', #2877 ) ;
#34173 = ORIENTED_EDGE ( 'NONE', *, *, #264, .F. ) ;
#34174 = CARTESIAN_POINT ( 'NONE',  ( -13.68341986734493609, 30.02787314512316641, -7.720655657447415443 ) ) ;
#34175 = CARTESIAN_POINT ( 'NONE',  ( -11.20940000001327341, -17.48797073134899094, -27.33040502637083691 ) ) ;
#34176 = FACE_BOUND ( 'NONE', #2422, .T. ) ;
#34177 = VERTEX_POINT ( 'NONE', #15266 ) ;
#34178 = CARTESIAN_POINT ( 'NONE',  ( -34.53800058995564370, -9.629687233961918835, -8.469964886165900708 ) ) ;
#34179 = CARTESIAN_POINT ( 'NONE',  ( -15.36059797614417022, -26.70982037388659691, -5.474171403654337631 ) ) ;
#34180 = FACE_OUTER_BOUND ( 'NONE', #32412, .T. ) ;
#34181 = EDGE_LOOP ( 'NONE', ( #10926, #5874, #14595, #19888 ) ) ;
#34182 = CARTESIAN_POINT ( 'NONE',  ( 21.99066440368976671, 1.589892210864482847, -22.84507827221558784 ) ) ;
#34183 = CARTESIAN_POINT ( 'NONE',  ( 10.44103466624280507, 32.57396620494213124, 9.500000000000000000 ) ) ;
#34184 = DIRECTION ( 'NONE',  ( 0.000000000000000000, 0.000000000000000000, -1.000000000000000000 ) ) ;
#34185 = ORIENTED_EDGE ( 'NONE', *, *, #15871, .F. ) ;
#34186 = CARTESIAN_POINT ( 'NONE',  ( -30.91582600597228137, -0.05403808547916669897, -5.000000000000000000 ) ) ;
#34187 = EDGE_LOOP ( 'NONE', ( #32039, #17111, #33553, #34821, #18897, #25726, #2458 ) ) ;
#34188 = CARTESIAN_POINT ( 'NONE',  ( 30.72234448700380938, -1.665297440091649372, -10.52892505583194449 ) ) ;
#34189 = AXIS2_PLACEMENT_3D ( 'NONE', #15341, #13078, #34626 ) ;
#34190 = AXIS2_PLACEMENT_3D ( 'NONE', #36029, #8588, #8187 ) ;
#34191 = CARTESIAN_POINT ( 'NONE',  ( 12.20447399291898272, -16.48659499025950836, -29.99999999999999289 ) ) ;
#34192 = CARTESIAN_POINT ( 'NONE',  ( 23.42865034949090841, -24.48547250943625997, 18.42518152272149479 ) ) ;
#34193 = ORIENTED_EDGE ( 'NONE', *, *, #40127, .T. ) ;
#34194 = CARTESIAN_POINT ( 'NONE',  ( -25.22597472235315053, 4.364516542823781542, -12.73472624478601034 ) ) ;
#34195 = LINE ( 'NONE', #12653, #3311 ) ;
#34196 = ADVANCED_FACE ( 'NONE', ( #27656 ), #24611, .T. ) ;
#34197 = CARTESIAN_POINT ( 'NONE',  ( 5.037377569032880587, 36.27272859966225127, 10.49999999999999645 ) ) ;
#34198 = CARTESIAN_POINT ( 'NONE',  ( -19.48557158514988785, -11.24999999999987743, 6.000000000000000000 ) ) ;
#34199 = EDGE_CURVE ( 'NONE', #34486, #38096, #32874, .T. ) ;
#34200 = FACE_OUTER_BOUND ( 'NONE', #32228, .T. ) ;
#34201 = ADVANCED_FACE ( 'NONE', ( #23717 ), #32471, .T. ) ;
#34202 = DIRECTION ( 'NONE',  ( 1.000000000000000000, 0.000000000000000000, 0.000000000000000000 ) ) ;
#34203 = CARTESIAN_POINT ( 'NONE',  ( 18.69515074622676920, 22.45407711375075621, 10.99999999997785771 ) ) ;
#34204 = CARTESIAN_POINT ( 'NONE',  ( -24.56734199138568897, 7.082464585399747214, -8.380301523606016545 ) ) ;
#34205 = CARTESIAN_POINT ( 'NONE',  ( 0.000000000000000000, 22.50000000000000355, 13.00000000000000178 ) ) ;
#34206 = DIRECTION ( 'NONE',  ( 0.6691306063588670083, 0.7431448254773863615, -0.000000000000000000 ) ) ;
#34207 = CARTESIAN_POINT ( 'NONE',  ( 23.08170797751215630, -26.79846190384431992, -5.889568152681599500 ) ) ;
#34208 = DIRECTION ( 'NONE',  ( -0.000000000000000000, -0.000000000000000000, -1.000000000000000000 ) ) ;
#34209 = CARTESIAN_POINT ( 'NONE',  ( 15.19751254492016734, 26.84389974300201587, -7.349166724040926191 ) ) ;
#34210 = VECTOR ( 'NONE', #23186, 1000.000000000000000 ) ;
#34211 = ORIENTED_EDGE ( 'NONE', *, *, #33333, .F. ) ;
#34213 = CIRCLE ( 'NONE', #1773, 1.000000000000014655 ) ;
#34212 = CARTESIAN_POINT ( 'NONE',  ( -15.79715600521433494, 23.30597418570086887, -9.749926740643289236 ) ) ;
#34214 = CARTESIAN_POINT ( 'NONE',  ( -25.50184330511921260, -18.07811769911583255, 20.50957957746029336 ) ) ;
#34215 = CARTESIAN_POINT ( 'NONE',  ( -19.48557158514998022, -11.24999999999982414, 23.00000000000000000 ) ) ;
#34216 = CARTESIAN_POINT ( 'NONE',  ( 13.23037898294574966, 22.19842390109810992, -16.44731654887686290 ) ) ;
#34217 = EDGE_LOOP ( 'NONE', ( #8039, #36177 ) ) ;
#34218 = DIRECTION ( 'NONE',  ( 0.000000000000000000, 0.000000000000000000, 1.000000000000000000 ) ) ;
#34219 = ADVANCED_FACE ( 'NONE', ( #8276 ), #29812, .T. ) ;
#34220 = ORIENTED_EDGE ( 'NONE', *, *, #14977, .T. ) ;
#34222 = FACE_OUTER_BOUND ( 'NONE', #4919, .T. ) ;
#34221 = CARTESIAN_POINT ( 'NONE',  ( -13.64709611685704260, 23.66733992415775845, -14.44796888404773583 ) ) ;
#34223 = EDGE_CURVE ( 'NONE', #12836, #30326, #15969, .T. ) ;
#34224 = CARTESIAN_POINT ( 'NONE',  ( -12.39674543852726174, -22.02096203800932273, -17.42484875458988469 ) ) ;
#34225 = CARTESIAN_POINT ( 'NONE',  ( 12.38757880222261143, 14.77067777473940069, 10.99387789255784220 ) ) ;
#34226 = EDGE_CURVE ( 'NONE', #38194, #9581, #7521, .T. ) ;
#34227 = VERTEX_POINT ( 'NONE', #36116 ) ;
#34228 = CARTESIAN_POINT ( 'NONE',  ( -22.18470991521814994, -10.78957402553765199, -20.70439974414385276 ) ) ;
#34229 = CARTESIAN_POINT ( 'NONE',  ( -8.861892952964076642, -21.31740138737636059, -19.76521263307946441 ) ) ;
#34230 = CARTESIAN_POINT ( 'NONE',  ( -25.19768531712390569, 23.50223830518991619, 7.000000000000000000 ) ) ;
#34231 = CARTESIAN_POINT ( 'NONE',  ( 12.43571604352363380, 16.42874407723720864, -28.15360703238361495 ) ) ;
#34232 = VERTEX_POINT ( 'NONE', #23111 ) ;
#34233 = CARTESIAN_POINT ( 'NONE',  ( 24.67187950889155346, 4.601540168446949686, -13.74189493147921759 ) ) ;
#34234 = FACE_OUTER_BOUND ( 'NONE', #2672, .T. ) ;
#34235 = CARTESIAN_POINT ( 'NONE',  ( -2.629601561899595374, 7.723830143584053509, 7.000000000000000000 ) ) ;
#34236 = CARTESIAN_POINT ( 'NONE',  ( -3.888911272182536294, 9.013845280544513727, 10.50000000000000000 ) ) ;
#34237 = EDGE_LOOP ( 'NONE', ( #9408, #18264, #19299, #27097 ) ) ;
#34238 = CARTESIAN_POINT ( 'NONE',  ( -30.70443338618256490, -0.3849243431390188541, -8.278649579022490101 ) ) ;
#34239 = CARTESIAN_POINT ( 'NONE',  ( 28.53789851150272838, -0.1047529870928948365, -12.52552137319313807 ) ) ;
#34240 = CARTESIAN_POINT ( 'NONE',  ( -22.03614745501234040, -31.14480216356518127, 11.00000000000000000 ) ) ;
#34241 = CARTESIAN_POINT ( 'NONE',  ( 23.91569629078776771, -19.26019901638226273, 20.50957957746005889 ) ) ;
#34242 = EDGE_LOOP ( 'NONE', ( #6924, #3558, #5532, #516 ) ) ;
#34243 = CARTESIAN_POINT ( 'NONE',  ( 20.55563217186196212, -29.52600041847795254, -13.99876745781546994 ) ) ;
#34244 = EDGE_CURVE ( 'NONE', #23135, #10104, #14668, .T. ) ;
#34245 = CARTESIAN_POINT ( 'NONE',  ( 0.8333333333333349247, 37.00000000000000711, 10.66666666666666607 ) ) ;
#34246 = VECTOR ( 'NONE', #25186, 999.9999999999998863 ) ;
#34247 = CONICAL_SURFACE ( 'NONE', #20619, 1.000000000000004441, 0.7853981633974482790 ) ;
#34248 = ADVANCED_FACE ( 'NONE', ( #25950 ), #35510, .F. ) ;
#34249 = ORIENTED_EDGE ( 'NONE', *, *, #12218, .T. ) ;
#34250 = CARTESIAN_POINT ( 'NONE',  ( 14.98890121934609532, -28.67928442654221044, -5.000000000000000000 ) ) ;
#34251 = TOROIDAL_SURFACE ( 'NONE', #16737, 1.000000000000000000, 0.5000000000000000000 ) ;
#34252 = CIRCLE ( 'NONE', #16742, 1.000000000000000000 ) ;
#34253 = CYLINDRICAL_SURFACE ( 'NONE', #9744, 0.5000000000000000000 ) ;
#34254 = CARTESIAN_POINT ( 'NONE',  ( 7.530592408760857559, 11.28437794979193498, 9.500000000000000000 ) ) ;
#34255 = CARTESIAN_POINT ( 'NONE',  ( 2.729340787065954732, 38.05821448855805755, -6.699057688494861829 ) ) ;
#34256 = CARTESIAN_POINT ( 'NONE',  ( -3.295881626406750975, 9.398963235502533209, 7.000000000000000000 ) ) ;
#34257 = CARTESIAN_POINT ( 'NONE',  ( 14.72308455763283064, 20.12562289931477366, 10.49999999999999822 ) ) ;
#34258 = DIRECTION ( 'NONE',  ( 1.000000000000000000, 0.000000000000000000, 0.000000000000000000 ) ) ;
#34259 = LINE ( 'NONE', #9474, #35500 ) ;
#34260 = DIRECTION ( 'NONE',  ( 0.000000000000000000, 0.000000000000000000, 1.000000000000000000 ) ) ;
#34261 = LINE ( 'NONE', #9679, #34004 ) ;
#34262 = CARTESIAN_POINT ( 'NONE',  ( 12.21266005302986279, 21.68539402877682676, -18.35945844235239832 ) ) ;
#34263 = PLANE ( 'NONE',  #17849 ) ;
#34264 = VERTEX_POINT ( 'NONE', #5028 ) ;
#34266 = CARTESIAN_POINT ( 'NONE',  ( -1.871208588069141143, 13.69667159339610762, 12.00000000000000000 ) ) ;
#34265 = CARTESIAN_POINT ( 'NONE',  ( -15.49039487082849220, 13.58517199178181301, -27.69483034437292801 ) ) ;
#34267 = DIRECTION ( 'NONE',  ( 1.000000000000000000, 0.000000000000000000, -0.000000000000000000 ) ) ;
#34268 = CARTESIAN_POINT ( 'NONE',  ( 9.621585592044306523, -18.34052516761964213, -27.44776497733833764 ) ) ;
#34269 = CARTESIAN_POINT ( 'NONE',  ( -22.30837096923181662, -26.42455506716093794, -8.094580056074205388 ) ) ;
#34270 = CARTESIAN_POINT ( 'NONE',  ( 15.40143551928530741, 26.74272614036931373, -5.946164455718055741 ) ) ;
#34271 = CARTESIAN_POINT ( 'NONE',  ( 14.73068410223729607, 25.41701562580275819, -10.65180837224440147 ) ) ;
#34272 = ORIENTED_EDGE ( 'NONE', *, *, #19953, .F. ) ;
#34273 = CARTESIAN_POINT ( 'NONE',  ( -2.871208588069141143, 13.69667159339610762, 12.00000000000000000 ) ) ;
#34274 = CARTESIAN_POINT ( 'NONE',  ( -11.12516049792199269, -20.47921145105273411, -20.54846162138489873 ) ) ;
#34275 = CARTESIAN_POINT ( 'NONE',  ( -33.53883321253935890, -0.1552552779192388210, 12.73282698324824480 ) ) ;
#34276 = AXIS2_PLACEMENT_3D ( 'NONE', #39579, #33896, #15597 ) ;
#34277 = VECTOR ( 'NONE', #30546, 999.9999999999998863 ) ;
#34278 = CARTESIAN_POINT ( 'NONE',  ( -29.47215113446729617, -21.71708447961223598, -9.294057262345292614 ) ) ;
#34279 = CARTESIAN_POINT ( 'NONE',  ( -0.3144284205193551562, -22.16443700259523197, -19.06343410368202385 ) ) ;
#34280 = CARTESIAN_POINT ( 'NONE',  ( 15.55086357314465495, 25.88735796154298541, -6.889558640719104510 ) ) ;
#34281 = CARTESIAN_POINT ( 'NONE',  ( 19.55223183195777281, 9.929862210829575986, -20.11535475670744688 ) ) ;
#34282 = CARTESIAN_POINT ( 'NONE',  ( 18.00000000000000000, 22.50000000000001421, 6.000000000000000000 ) ) ;
#34283 = AXIS2_PLACEMENT_3D ( 'NONE', #4152, #13496, #32196 ) ;
#34284 = VERTEX_POINT ( 'NONE', #1585 ) ;
#34285 = CARTESIAN_POINT ( 'NONE',  ( -33.40104146632486248, -3.480120356603942255, -6.360699399790051167 ) ) ;
#34286 = CIRCLE ( 'NONE', #24539, 1.000000000000000000 ) ;
#34287 = CARTESIAN_POINT ( 'NONE',  ( -23.18043107539034509, 0.3100950997616090943, 19.99202127657445516 ) ) ;
#34288 = VERTEX_POINT ( 'NONE', #10519 ) ;
#34289 = DIRECTION ( 'NONE',  ( 0.000000000000000000, 0.000000000000000000, 1.000000000000000000 ) ) ;
#34290 = DIRECTION ( 'NONE',  ( -0.6916548014802208488, 0.1470157664652026186, -0.7071067811865512365 ) ) ;
#34291 = CARTESIAN_POINT ( 'NONE',  ( -29.02761408569459434, 0.6971569698290208672, -10.19582416827852356 ) ) ;
#34292 = CARTESIAN_POINT ( 'NONE',  ( 20.59519988482301756, -7.609356043779510692, -24.29945422642990849 ) ) ;
#34293 = CARTESIAN_POINT ( 'NONE',  ( 36.22115687806114437, -16.54570019420276594, 13.92931973827800185 ) ) ;
#34294 = ORIENTED_EDGE ( 'NONE', *, *, #34447, .T. ) ;
#34295 = CARTESIAN_POINT ( 'NONE',  ( -15.02235689379176620, 21.92659494635362449, 11.00000000000000000 ) ) ;
#34296 = ORIENTED_EDGE ( 'NONE', *, *, #1577, .F. ) ;
#34297 = CARTESIAN_POINT ( 'NONE',  ( 7.713869163865849643, 10.18146832927074996, 10.49999999999999822 ) ) ;
#34298 = CARTESIAN_POINT ( 'NONE',  ( 12.99038105676654986, 14.99999999999993960, 7.000000000000000000 ) ) ;
#34299 = VECTOR ( 'NONE', #37762, 1000.000000000000000 ) ;
#34300 = AXIS2_PLACEMENT_3D ( 'NONE', #14649, #29683, #23185 ) ;
#34301 = DIRECTION ( 'NONE',  ( -0.4067366430757888840, 0.9135454576426058626, 0.000000000000000000 ) ) ;
#34302 = VERTEX_POINT ( 'NONE', #29610 ) ;
#34303 = CARTESIAN_POINT ( 'NONE',  ( -2.518168780898724979, 31.12813172238224269, -14.74331629931110221 ) ) ;
#34304 = FACE_OUTER_BOUND ( 'NONE', #32935, .T. ) ;
#34305 = DIRECTION ( 'NONE',  ( -0.000000000000000000, -0.000000000000000000, -1.000000000000000000 ) ) ;
#34306 = CONICAL_SURFACE ( 'NONE', #576, 1.000000000000002665, 0.7853981633974548293 ) ;
#34307 = DIRECTION ( 'NONE',  ( -0.000000000000000000, -0.000000000000000000, 1.000000000000000000 ) ) ;
#34308 = LINE ( 'NONE', #39644, #10655 ) ;
#34309 = CARTESIAN_POINT ( 'NONE',  ( -6.935776944912362296, 22.65328985282726393, 13.00000000000000178 ) ) ;
#34310 = CARTESIAN_POINT ( 'NONE',  ( 8.705524501264831017, 18.63857284810273285, -28.61403163583886666 ) ) ;
#34311 = ORIENTED_EDGE ( 'NONE', *, *, #14235, .T. ) ;
#34312 = CARTESIAN_POINT ( 'NONE',  ( -18.40526182805578870, 10.96415812414948299, -22.25133746893234843 ) ) ;
#34313 = DIRECTION ( 'NONE',  ( 1.000000000000000000, 0.000000000000000000, 0.000000000000000000 ) ) ;
#34314 = CARTESIAN_POINT ( 'NONE',  ( 15.45591863128356991, -26.53792291655177138, -7.354334154706036131 ) ) ;
#34315 = DIRECTION ( 'NONE',  ( 1.000000000000000000, 0.000000000000000000, -0.000000000000000000 ) ) ;
#34316 = CARTESIAN_POINT ( 'NONE',  ( 15.07823932231967312, 26.21524158488056244, -8.764214361564787836 ) ) ;
#34317 = CARTESIAN_POINT ( 'NONE',  ( -15.72991998290134141, -16.18894361744923316, -20.11584339644716479 ) ) ;
#34318 = FACE_OUTER_BOUND ( 'NONE', #4932, .T. ) ;
#34319 = CARTESIAN_POINT ( 'NONE',  ( -15.38479227967843244, 26.80208864768298227, -5.945536811150080148 ) ) ;
#34320 = CARTESIAN_POINT ( 'NONE',  ( -14.52190046171712368, -14.48203382165085529, -29.24551301647182910 ) ) ;
#34321 = CARTESIAN_POINT ( 'NONE',  ( 8.048738417910207943, -21.01130598342334466, -20.86836972816746538 ) ) ;
#34322 = CARTESIAN_POINT ( 'NONE',  ( 15.27515461409865338, 26.26107631968810452, -7.828561414818718589 ) ) ;
#34323 = CARTESIAN_POINT ( 'NONE',  ( 16.98753680658756338, -11.47516704400511678, -30.00000000000002842 ) ) ;
#34324 = ADVANCED_FACE ( 'NONE', ( #11129 ), #39150, .F. ) ;
#34325 = CARTESIAN_POINT ( 'NONE',  ( 5.478580155932369244, 36.03438916679310466, 10.99387789255784043 ) ) ;
#34326 = EDGE_LOOP ( 'NONE', ( #26663, #3952, #7330, #22422 ) ) ;
#34327 = CARTESIAN_POINT ( 'NONE',  ( -7.162297359993949897, 23.99211573040527057, -19.88175472533177057 ) ) ;
#34328 = DIRECTION ( 'NONE',  ( -0.000000000000000000, -0.000000000000000000, 1.000000000000000000 ) ) ;
#34329 = LINE ( 'NONE', #9550, #12693 ) ;
#34330 = AXIS2_PLACEMENT_3D ( 'NONE', #21370, #15070, #39847 ) ;
#34331 = CIRCLE ( 'NONE', #26557, 1.000000000000000888 ) ;
#34332 = FACE_OUTER_BOUND ( 'NONE', #31320, .T. ) ;
#34333 = ORIENTED_EDGE ( 'NONE', *, *, #12904, .F. ) ;
#34334 = CARTESIAN_POINT ( 'NONE',  ( 25.19553447042465422, 0.4082270625723977142, -17.44156586897039674 ) ) ;
#34335 = EDGE_CURVE ( 'NONE', #35064, #18367, #15804, .T. ) ;
#34336 = CARTESIAN_POINT ( 'NONE',  ( 14.48316745233715075, 26.40420323494709365, 7.455539900862802050 ) ) ;
#34337 = FACE_OUTER_BOUND ( 'NONE', #29998, .T. ) ;
#34338 = ADVANCED_FACE ( 'NONE', ( #16829 ), #32189, .T. ) ;
#34339 = CIRCLE ( 'NONE', #21346, 1.000000000000000000 ) ;
#34340 = B_SPLINE_SURFACE_WITH_KNOTS ( 'NONE', 1, 3, ( 
 ( #29510, #2089, #1686, #14469, #29311, #26861, #13869, #36015, #23418, #35810 ),
 ( #7965, #11227, #8174, #20578, #17536, #39250, #30718, #27262, #11823, #36609 ) ),
 .UNSPECIFIED., .F., .F., .F.,
 ( 2, 2 ),
 ( 4, 2, 2, 2, 4 ),
 ( 0.000000000000000000, 1.000000000000000000 ),
 ( 4.324792293729522896, 4.717491375428245703, 5.110190457126968511, 5.502889538825691318, 5.895588620524415013 ),
 .UNSPECIFIED. ) ;
#34341 = VERTEX_POINT ( 'NONE', #1381 ) ;
#34342 = CARTESIAN_POINT ( 'NONE',  ( -30.68377196017895514, 0.01256353404212825174, -6.888008929677917003 ) ) ;
#34343 = DIRECTION ( 'NONE',  ( 0.000000000000000000, 0.000000000000000000, -1.000000000000000000 ) ) ;
#34344 = VERTEX_POINT ( 'NONE', #13763 ) ;
#34345 = CARTESIAN_POINT ( 'NONE',  ( 34.68926902183491023, -7.262543041722620885, -7.195073363372168629 ) ) ;
#34346 = ORIENTED_EDGE ( 'NONE', *, *, #35727, .T. ) ;
#34347 = CARTESIAN_POINT ( 'NONE',  ( -1.940950748631915967, 40.43805239114131211, 12.14047268033097460 ) ) ;
#34348 = CARTESIAN_POINT ( 'NONE',  ( -7.713869163866016621, 10.18146832927085121, 7.000000000000000000 ) ) ;
#34349 = CARTESIAN_POINT ( 'NONE',  ( 2.036571916123615100, 8.108948098542045457, 11.00000000000000000 ) ) ;
#34350 = CARTESIAN_POINT ( 'NONE',  ( -11.47663208683763614, 27.06976447313135381, 19.27171037444124835 ) ) ;
#34351 = DIRECTION ( 'NONE',  ( 0.1470157664652248786, 0.6916548014802228472, -0.7071067811865445751 ) ) ;
#34352 = EDGE_LOOP ( 'NONE', ( #18291, #9386, #15132, #39897 ) ) ;
#34353 = LINE ( 'NONE', #9167, #6672 ) ;
#34354 = CARTESIAN_POINT ( 'NONE',  ( -16.15214517906706604, 12.62672657229183493, -30.00000000000001421 ) ) ;
#34355 = EDGE_CURVE ( 'NONE', #10259, #2141, #34647, .T. ) ;
#34356 = CARTESIAN_POINT ( 'NONE',  ( 12.23327497914553597, 13.81973598992451713, 7.000000000000000000 ) ) ;
#34357 = EDGE_CURVE ( 'NONE', #20669, #26489, #26361, .T. ) ;
#34358 = DIRECTION ( 'NONE',  ( -1.000000000000000000, 0.000000000000000000, 0.000000000000000000 ) ) ;
#34359 = CARTESIAN_POINT ( 'NONE',  ( 17.63833218921318036, 18.28698162993199006, -10.81605670618053772 ) ) ;
#34361 = CIRCLE ( 'NONE', #3870, 0.5000000000000004441 ) ;
#34360 = CARTESIAN_POINT ( 'NONE',  ( 9.666666246803703899, 33.51585335600255178, -9.377146499650510947 ) ) ;
#34362 = CARTESIAN_POINT ( 'NONE',  ( 11.46616884858724461, -17.50945150416644580, -26.67433058872985896 ) ) ;
#34363 = CARTESIAN_POINT ( 'NONE',  ( 8.169448529985288587, 9.961039561530309783, 10.49999999999999822 ) ) ;
#34364 = CIRCLE ( 'NONE', #16859, 0.4999999999999998335 ) ;
#34365 = DIRECTION ( 'NONE',  ( -0.000000000000000000, -0.000000000000000000, -1.000000000000000000 ) ) ;
#34366 = ORIENTED_EDGE ( 'NONE', *, *, #23412, .F. ) ;
#34367 = CARTESIAN_POINT ( 'NONE',  ( -11.01126394183691737, 17.29167595606526575, -29.34893377464801034 ) ) ;
#34368 = CARTESIAN_POINT ( 'NONE',  ( -33.86703583613317647, -12.56047426484087914, 17.92354375535250810 ) ) ;
#34369 = CARTESIAN_POINT ( 'NONE',  ( 9.708222066279674323, -18.59847043248773346, -26.23215512439793073 ) ) ;
#34370 = CARTESIAN_POINT ( 'NONE',  ( -13.03641663870442891, 15.85735326529964873, 12.00000000000000000 ) ) ;
#34371 = EDGE_LOOP ( 'NONE', ( #11501, #1354, #14787, #34688 ) ) ;
#34372 = VERTEX_POINT ( 'NONE', #35715 ) ;
#34373 = CARTESIAN_POINT ( 'NONE',  ( -11.31816643715098003, 20.85646170319403225, -20.38269801284040739 ) ) ;
#34374 = CARTESIAN_POINT ( 'NONE',  ( -19.39179092967061280, -27.18907619913308338, -6.364284092723044850 ) ) ;
#34375 = EDGE_CURVE ( 'NONE', #31487, #1365, #37374, .T. ) ;
#34376 = FACE_BOUND ( 'NONE', #20983, .T. ) ;
#34377 = ORIENTED_EDGE ( 'NONE', *, *, #39692, .T. ) ;
#34378 = CARTESIAN_POINT ( 'NONE',  ( -21.76008645254054485, -6.076781144368697873, -23.17579509458892772 ) ) ;
#34379 = CARTESIAN_POINT ( 'NONE',  ( -15.30203309327454697, -26.66931059147099248, -5.946105180059766404 ) ) ;
#34380 = CARTESIAN_POINT ( 'NONE',  ( 34.33271597229082772, -24.82403720151193482, 11.00000000000000000 ) ) ;
#34381 = ORIENTED_EDGE ( 'NONE', *, *, #38997, .F. ) ;
#34382 = CARTESIAN_POINT ( 'NONE',  ( 30.10894569176270963, 0.2553795474248102271, -8.300237564504525878 ) ) ;
#34383 = DIRECTION ( 'NONE',  ( 0.000000000000000000, -0.000000000000000000, 1.000000000000000000 ) ) ;
#34384 = LINE ( 'NONE', #12644, #19949 ) ;
#34385 = ORIENTED_EDGE ( 'NONE', *, *, #16962, .T. ) ;
#34386 = CARTESIAN_POINT ( 'NONE',  ( -20.81963202979064675, 0.7819132637707100209, -26.82682968236362342 ) ) ;
#34387 = VERTEX_POINT ( 'NONE', #33677 ) ;
#34388 = CARTESIAN_POINT ( 'NONE',  ( 20.49417979596975314, -0.6040919881699248206, -30.00000000000000000 ) ) ;
#34389 = CARTESIAN_POINT ( 'NONE',  ( 18.63203339187605323, -8.577389641220674932, -30.00000000000002842 ) ) ;
#34390 = CARTESIAN_POINT ( 'NONE',  ( 30.06723386280229704, -23.25956985441296609, 16.30093088680191471 ) ) ;
#34391 = ORIENTED_EDGE ( 'NONE', *, *, #29746, .F. ) ;
#34392 = CARTESIAN_POINT ( 'NONE',  ( -26.80025940592816980, 4.409708740836313368, -6.908737485017725888 ) ) ;
#34393 = AXIS2_PLACEMENT_3D ( 'NONE', #38745, #29399, #24104 ) ;
#34394 = LINE ( 'NONE', #25240, #17612 ) ;
#34395 = FACE_OUTER_BOUND ( 'NONE', #37676, .T. ) ;
#34396 = LINE ( 'NONE', #34792, #15514 ) ;
#34397 = EDGE_CURVE ( 'NONE', #16754, #2909, #35438, .T. ) ;
#34398 = LINE ( 'NONE', #12853, #24688 ) ;
#34399 = EDGE_CURVE ( 'NONE', #6396, #10818, #9389, .T. ) ;
#34400 = AXIS2_PLACEMENT_3D ( 'NONE', #2424, #39787, #8918 ) ;
#34401 = FACE_BOUND ( 'NONE', #32907, .T. ) ;
#34402 = CARTESIAN_POINT ( 'NONE',  ( 20.16616670141972278, 17.52816929147979508, 13.92931973827773362 ) ) ;
#34403 = CARTESIAN_POINT ( 'NONE',  ( -19.87474022753053760, 5.715682130751402745, -27.09873607923148242 ) ) ;
#34404 = CARTESIAN_POINT ( 'NONE',  ( 10.18324034840045478, 28.21559575157615996, 6.000000000000000000 ) ) ;
#34405 = DIRECTION ( 'NONE',  ( 1.000000000000000000, 0.000000000000000000, 0.000000000000000000 ) ) ;
#34406 = CARTESIAN_POINT ( 'NONE',  ( 22.86001989442993221, -26.57036944630193531, -7.206849629775319066 ) ) ;
#34407 = DIRECTION ( 'NONE',  ( 0.8090169943749430104, -0.5877852522924791323, 0.000000000000000000 ) ) ;
#34408 = CARTESIAN_POINT ( 'NONE',  ( 11.71074545945343459, 19.57405692998802849, -21.58253805519631285 ) ) ;
#34409 = ORIENTED_EDGE ( 'NONE', *, *, #37932, .T. ) ;
#34410 = CARTESIAN_POINT ( 'NONE',  ( -12.32086914825891100, 16.51387112319463668, -28.14762509869785490 ) ) ;
#34411 = CARTESIAN_POINT ( 'NONE',  ( -27.94267546441488648, -5.959640785454821454, 20.25080042701541316 ) ) ;
#34412 = DIRECTION ( 'NONE',  ( 0.1470157664652028962, 0.6916548014802217370, 0.7071067811865503483 ) ) ;
#34413 = CARTESIAN_POINT ( 'NONE',  ( 11.15651162539644758, 17.59102559401446797, -26.83334858599937434 ) ) ;
#34414 = EDGE_LOOP ( 'NONE', ( #15836, #16034, #30698, #23241 ) ) ;
#34415 = CARTESIAN_POINT ( 'NONE',  ( -5.767236651883567156, 13.71142893291686171, 10.50000000000000000 ) ) ;
#34416 = VECTOR ( 'NONE', #26750, 999.9999999999998863 ) ;
#34417 = ORIENTED_EDGE ( 'NONE', *, *, #2689, .T. ) ;
#34419 = CYLINDRICAL_SURFACE ( 'NONE', #10816, 0.4999999999999998335 ) ;
#34418 = CARTESIAN_POINT ( 'NONE',  ( -15.19155625167785217, 26.86276375165831709, -7.348661200013363093 ) ) ;
#34420 = CARTESIAN_POINT ( 'NONE',  ( -9.620588153019252076, -18.24824637790410264, -28.07461452513831901 ) ) ;
#34421 = EDGE_CURVE ( 'NONE', #2164, #35202, #21464, .T. ) ;
#34422 = CARTESIAN_POINT ( 'NONE',  ( 11.89031559783844827, 11.79390851039467236, 12.00000000000000000 ) ) ;
#34423 = ORIENTED_EDGE ( 'NONE', *, *, #36084, .F. ) ;
#34424 = CARTESIAN_POINT ( 'NONE',  ( -19.49766833869776406, -10.22472788658466314, -24.22319853153801716 ) ) ;
#34425 = CARTESIAN_POINT ( 'NONE',  ( -12.59681229544040981, -23.55840868995836246, -14.51872154415304372 ) ) ;
#34426 = CYLINDRICAL_SURFACE ( 'NONE', #37782, 5.999999999999998224 ) ;
#34427 = CARTESIAN_POINT ( 'NONE',  ( 16.14914138567496593, 22.68994970326915706, -9.283840620700846813 ) ) ;
#34428 = ORIENTED_EDGE ( 'NONE', *, *, #10166, .F. ) ;
#34429 = CARTESIAN_POINT ( 'NONE',  ( 19.66799848466891021, 5.910365882540998150, -28.83167407526441295 ) ) ;
#34430 = DIRECTION ( 'NONE',  ( 1.000000000000000000, 0.000000000000000000, 0.000000000000000000 ) ) ;
#34431 = EDGE_CURVE ( 'NONE', #17047, #36571, #30426, .T. ) ;
#34432 = CARTESIAN_POINT ( 'NONE',  ( -9.201548168576545450, 26.54122646004472585, 10.50000000000000533 ) ) ;
#34433 = DIRECTION ( 'NONE',  ( 0.000000000000000000, 0.000000000000000000, 1.000000000000000000 ) ) ;
#34434 = VERTEX_POINT ( 'NONE', #33869 ) ;
#34435 = CARTESIAN_POINT ( 'NONE',  ( -20.55088806256009804, 0.1873367080201817914, -28.68331257151926650 ) ) ;
#34436 = CARTESIAN_POINT ( 'NONE',  ( 29.65834914286953250, -0.2741925911900300328, -10.62574247128935490 ) ) ;
#34437 = VECTOR ( 'NONE', #12060, 1000.000000000000000 ) ;
#34438 = CARTESIAN_POINT ( 'NONE',  ( 18.16616693041810748, -20.30807083247596623, 20.50957957746011573 ) ) ;
#34439 = AXIS2_PLACEMENT_3D ( 'NONE', #35299, #1782, #38546 ) ;
#34440 = ORIENTED_EDGE ( 'NONE', *, *, #33825, .T. ) ;
#34441 = CARTESIAN_POINT ( 'NONE',  ( 15.72991998290128990, -16.18894361744929000, -20.11584339644706887 ) ) ;
#34442 = LINE ( 'NONE', #28140, #12809 ) ;
#34443 = EDGE_LOOP ( 'NONE', ( #20821, #14188, #17471, #27916, #31330, #18539, #1732, #34509, #18906, #949, #24830, #26762, #1321, #21585, #13882, #8602, #28058, #2226, #22702, #37789, #2029, #17965, #14888, #7387, #39750, #2230, #11101, #37658, #10811, #13333, #30289, #39377, #35826, #7530, #13206, #6129, #30496, #965, #19310, #2467, #18460, #40089, #1661, #2889, #3215, #10203, #15249, #25797, #416, #16046, #9646, #23294, #13477, #28774, #29295 ) ) ;
#34444 = AXIS2_PLACEMENT_3D ( 'NONE', #10368, #20319, #4472 ) ;
#34445 = DIRECTION ( 'NONE',  ( 0.000000000000000000, 0.000000000000000000, 1.000000000000000000 ) ) ;
#34446 = EDGE_CURVE ( 'NONE', #15350, #22657, #38684, .T. ) ;
#34447 = EDGE_CURVE ( 'NONE', #16160, #16754, #33480, .T. ) ;
#34448 = DIRECTION ( 'NONE',  ( 0.000000000000000000, 0.000000000000000000, 1.000000000000000000 ) ) ;
#34449 = CARTESIAN_POINT ( 'NONE',  ( -14.97277451176450924, 21.48159783397892397, 10.49999999999999822 ) ) ;
#34450 = CARTESIAN_POINT ( 'NONE',  ( 3.737393764735764012, 36.42673618779068079, -9.293156675928717192 ) ) ;
#34451 = CARTESIAN_POINT ( 'NONE',  ( -13.53280532430055416, 27.77329351534951485, 10.66666666666666963 ) ) ;
#34452 = LINE ( 'NONE', #12705, #14344 ) ;
#34453 = LINE ( 'NONE', #19401, #9067 ) ;
#34454 = DIRECTION ( 'NONE',  ( 0.9135454576426005335, -0.4067366430758009299, 0.000000000000000000 ) ) ;
#34455 = DIRECTION ( 'NONE',  ( -0.6691306063588571273, 0.7431448254773952433, 0.000000000000000000 ) ) ;
#34456 = CARTESIAN_POINT ( 'NONE',  ( -17.34253826607186966, 27.32041144404028188, 11.00000000000000000 ) ) ;
#34457 = CARTESIAN_POINT ( 'NONE',  ( 15.09524128205707072, 27.81033699783984403, -5.469350279337763965 ) ) ;
#34458 = PLANE ( 'NONE',  #34698 ) ;
#34459 = ORIENTED_EDGE ( 'NONE', *, *, #23651, .F. ) ;
#34460 = CONICAL_SURFACE ( 'NONE', #35771, 1.000000000000016431, 0.7853981633974533860 ) ;
#34462 = DIRECTION ( 'NONE',  ( 1.000000000000000000, 0.000000000000000000, 0.000000000000000000 ) ) ;
#34461 = CARTESIAN_POINT ( 'NONE',  ( -15.52769020334683248, 13.63339048884298244, -27.12696093855038626 ) ) ;
#34463 = CARTESIAN_POINT ( 'NONE',  ( -10.10646936306323518, 32.94553861768095970, 11.00000000000000000 ) ) ;
#34464 = VECTOR ( 'NONE', #11617, 1000.000000000000000 ) ;
#34465 = CARTESIAN_POINT ( 'NONE',  ( 9.476873889470034840, -18.17797724348699973, -30.00000000000000000 ) ) ;
#34466 = CARTESIAN_POINT ( 'NONE',  ( -15.52302998078869045, -20.83641103844984244, -18.06021460743331630 ) ) ;
#34467 = CARTESIAN_POINT ( 'NONE',  ( 14.53385677051821290, 24.96618126256258918, -11.59944340942744034 ) ) ;
#34468 = CARTESIAN_POINT ( 'NONE',  ( 15.40885724145108249, 26.80895719503613606, -5.000000000000000000 ) ) ;
#34469 = ORIENTED_EDGE ( 'NONE', *, *, #21090, .T. ) ;
#34470 = DIRECTION ( 'NONE',  ( 1.000000000000000000, 0.000000000000000000, 0.000000000000000000 ) ) ;
#34471 = CARTESIAN_POINT ( 'NONE',  ( -9.450798935534860945, -18.19154675410751310, -29.34931450394937613 ) ) ;
#34472 = EDGE_CURVE ( 'NONE', #1614, #34434, #1678, .T. ) ;
#34473 = CARTESIAN_POINT ( 'NONE',  ( -34.78305373678684731, -20.08200543817108752, 13.32518128616608699 ) ) ;
#34474 = CARTESIAN_POINT ( 'NONE',  ( -31.25384702405562010, -21.56854527912942743, -7.121365677064556365 ) ) ;
#34475 = CARTESIAN_POINT ( 'NONE',  ( -4.767036241218260528, -24.79638281802436595, -7.416925339961604635 ) ) ;
#34476 = CARTESIAN_POINT ( 'NONE',  ( 12.70314503164341957, 20.08029170463875346, -19.55002564702039436 ) ) ;
#34478 = EDGE_CURVE ( 'NONE', #24820, #12832, #29575, .T. ) ;
#34477 = ORIENTED_EDGE ( 'NONE', *, *, #6067, .F. ) ;
#34479 = CARTESIAN_POINT ( 'NONE',  ( 20.48907729733518224, 9.348693102924391596, -18.00296546062092773 ) ) ;
#34480 = CARTESIAN_POINT ( 'NONE',  ( -18.23649648353780961, -16.09146789626143814, 23.00000000000000000 ) ) ;
#34481 = CARTESIAN_POINT ( 'NONE',  ( 6.553841457908355927, 36.68830644081927517, 16.87380292611439003 ) ) ;
#34482 = EDGE_LOOP ( 'NONE', ( #29537, #33380, #4331 ) ) ;
#34483 = CARTESIAN_POINT ( 'NONE',  ( -20.42150163017176467, -2.418834129410442735, -28.59310508139819262 ) ) ;
#34484 = EDGE_CURVE ( 'NONE', #8314, #11507, #8682, .T. ) ;
#34485 = CARTESIAN_POINT ( 'NONE',  ( -30.90861030616023086, -0.03770625498002080217, 16.30093088680190760 ) ) ;
#34486 = VERTEX_POINT ( 'NONE', #30620 ) ;
#34487 = CARTESIAN_POINT ( 'NONE',  ( 14.36830325120613594, 20.48707633493483371, 11.00000000000000000 ) ) ;
#34488 = LINE ( 'NONE', #32241, #31028 ) ;
#34489 = CARTESIAN_POINT ( 'NONE',  ( -30.04950648410215308, 0.8457024189327566610, -5.474049384667112328 ) ) ;
#34490 = CARTESIAN_POINT ( 'NONE',  ( 34.89591069308838911, -14.04604181989983935, -7.131079328635554937 ) ) ;
#34491 = CARTESIAN_POINT ( 'NONE',  ( 16.90387162101912111, -28.96785393638771566, 12.73282698324709372 ) ) ;
#34492 = CIRCLE ( 'NONE', #11783, 1.000000000000000000 ) ;
#34493 = AXIS2_PLACEMENT_3D ( 'NONE', #9763, #37192, #21743 ) ;
#34494 = ORIENTED_EDGE ( 'NONE', *, *, #13823, .T. ) ;
#34495 = LINE ( 'NONE', #35844, #18075 ) ;
#34496 = VERTEX_POINT ( 'NONE', #11729 ) ;
#34497 = LINE ( 'NONE', #9316, #19712 ) ;
#34498 = EDGE_CURVE ( 'NONE', #34284, #29758, #15883, .T. ) ;
#34499 = EDGE_CURVE ( 'NONE', #6918, #31607, #37944, .T. ) ;
#34500 = DIRECTION ( 'NONE',  ( 1.000000000000000000, 0.000000000000000000, 0.000000000000000000 ) ) ;
#34501 = ORIENTED_EDGE ( 'NONE', *, *, #14597, .F. ) ;
#34502 = CARTESIAN_POINT ( 'NONE',  ( -3.913438197523118500, 34.93452689860740179, -11.08172396340525800 ) ) ;
#34503 = LINE ( 'NONE', #37551, #3557 ) ;
#34504 = CARTESIAN_POINT ( 'NONE',  ( -5.440908595777639079, 35.94977745735568675, 11.00000000000000000 ) ) ;
#34505 = LINE ( 'NONE', #28201, #20184 ) ;
#34506 = DIRECTION ( 'NONE',  ( 0.000000000000000000, 0.000000000000000000, 1.000000000000000000 ) ) ;
#34507 = CARTESIAN_POINT ( 'NONE',  ( -2.140527761532693418, 7.619874298175171035, 7.000000000000000000 ) ) ;
#34508 = CARTESIAN_POINT ( 'NONE',  ( 8.682226116870198851, 18.58302833326690262, -29.99999999999999645 ) ) ;
#34509 = ORIENTED_EDGE ( 'NONE', *, *, #3566, .F. ) ;
#34510 = CARTESIAN_POINT ( 'NONE',  ( -19.49730985190667454, 11.63805976899694272, -16.98486636064236066 ) ) ;
#34511 = CARTESIAN_POINT ( 'NONE',  ( 17.76739295965463583, 31.93461338995192378, 11.00000000000000000 ) ) ;
#34512 = CARTESIAN_POINT ( 'NONE',  ( 15.13256764714127200, -26.15839328056117807, -8.765583185149749212 ) ) ;
#34513 = DIRECTION ( 'NONE',  ( 0.000000000000000000, 0.000000000000000000, 1.000000000000000000 ) ) ;
#34514 = CARTESIAN_POINT ( 'NONE',  ( 12.89912295072652171, 21.70184657798560934, -17.43093282895208418 ) ) ;
#34515 = CARTESIAN_POINT ( 'NONE',  ( -3.859759734048395785E-14, -22.74351282448223799, -21.56489709563626533 ) ) ;
#34516 = FACE_OUTER_BOUND ( 'NONE', #1954, .T. ) ;
#34517 =( REPRESENTATION_RELATIONSHIP ('NONE','NONE', #15382, #8618 ) REPRESENTATION_RELATIONSHIP_WITH_TRANSFORMATION ( #14203 )SHAPE_REPRESENTATION_RELATIONSHIP( ) );
#34518 = CARTESIAN_POINT ( 'NONE',  ( -14.07208788724811477, -14.92005942896404669, -30.00000000000001421 ) ) ;
#34519 = CARTESIAN_POINT ( 'NONE',  ( 9.624070444996608131, -20.74343144170484621, -20.71045537718826424 ) ) ;
#34520 = CARTESIAN_POINT ( 'NONE',  ( 11.17775020265387553, 17.43158091459943293, -27.45587064061833615 ) ) ;
#34521 = EDGE_CURVE ( 'NONE', #27468, #6833, #28200, .T. ) ;
#34522 = CARTESIAN_POINT ( 'NONE',  ( 16.98753680658756338, -11.47516704400511500, -29.21470985754709915 ) ) ;
#34523 = CARTESIAN_POINT ( 'NONE',  ( 8.145563986382251542, 10.43794218875012270, 11.00000000000000000 ) ) ;
#34524 = CARTESIAN_POINT ( 'NONE',  ( 5.558911028763954931, 36.44455752850700492, 10.49999999999999822 ) ) ;
#34525 = ORIENTED_EDGE ( 'NONE', *, *, #9229, .F. ) ;
#34526 = CARTESIAN_POINT ( 'NONE',  ( -7.450067287675317118, 31.53556863671898824, -12.97597155326280749 ) ) ;
#34527 = DIRECTION ( 'NONE',  ( 0.000000000000000000, 0.000000000000000000, 1.000000000000000000 ) ) ;
#34528 = CARTESIAN_POINT ( 'NONE',  ( -12.30736835487442704, 14.81698729810789672, 7.000000000000000000 ) ) ;
#34529 = ORIENTED_EDGE ( 'NONE', *, *, #27200, .T. ) ;
#34530 = CARTESIAN_POINT ( 'NONE',  ( 23.92490223308770680, 0.5234191831326777677, -19.50078697197409383 ) ) ;
#34531 = DIRECTION ( 'NONE',  ( 1.000000000000000000, 0.000000000000000000, 0.000000000000000000 ) ) ;
#34532 = CIRCLE ( 'NONE', #26736, 1.000000000000000888 ) ;
#34533 = DIRECTION ( 'NONE',  ( 0.6729908358753983189, 0.000000000000000000, -0.7396508195275205422 ) ) ;
#34534 = ORIENTED_EDGE ( 'NONE', *, *, #27851, .F. ) ;
#34535 = CARTESIAN_POINT ( 'NONE',  ( -24.54231522334037408, 0.4673129468823389310, -18.45614678722852275 ) ) ;
#34536 = LINE ( 'NONE', #35136, #22856 ) ;
#34537 = ORIENTED_EDGE ( 'NONE', *, *, #30104, .F. ) ;
#34538 = CARTESIAN_POINT ( 'NONE',  ( 34.82172620998498047, -7.298527031968996326, -6.759101599951145012 ) ) ;
#34539 = AXIS2_PLACEMENT_3D ( 'NONE', #12583, #38167, #12780 ) ;
#34540 = VERTEX_POINT ( 'NONE', #27562 ) ;
#34541 = CARTESIAN_POINT ( 'NONE',  ( 17.28285333400958734, 27.30382183500221061, 12.14047268033097460 ) ) ;
#34542 = CYLINDRICAL_SURFACE ( 'NONE', #2178, 1.000000000000000000 ) ;
#34543 = CARTESIAN_POINT ( 'NONE',  ( -15.01937947523880545, 1.539368754276113638, 22.99999999999999289 ) ) ;
#34544 = CARTESIAN_POINT ( 'NONE',  ( 11.47663208683638025, 27.06976447313250489, 19.27171037444299984 ) ) ;
#34545 = DIRECTION ( 'NONE',  ( -0.000000000000000000, -0.000000000000000000, -1.000000000000000000 ) ) ;
#34546 = EDGE_LOOP ( 'NONE', ( #4372, #3901, #26145, #20553 ) ) ;
#34547 = VECTOR ( 'NONE', #33820, 1000.000000000000000 ) ;
#34548 = CARTESIAN_POINT ( 'NONE',  ( 4.002483478063409095, 8.479530061156575371, 10.49999999999999822 ) ) ;
#34549 = CARTESIAN_POINT ( 'NONE',  ( -19.64406637653126353, -6.006936621460132741, -30.00000000000001066 ) ) ;
#34550 = CARTESIAN_POINT ( 'NONE',  ( -2.605702774688126500, 27.44183462127829642, 13.00000000000000178 ) ) ;
#34551 = EDGE_CURVE ( 'NONE', #39411, #39304, #36715, .T. ) ;
#34552 = CARTESIAN_POINT ( 'NONE',  ( 7.530592408760857559, 11.28437794979193498, 9.500000000000000000 ) ) ;
#34553 = CARTESIAN_POINT ( 'NONE',  ( 14.66009104707607769, 15.34232611559405335, -24.24183191570947216 ) ) ;
#34554 = CARTESIAN_POINT ( 'NONE',  ( 9.894829114067803744, 34.42816785295285342, -7.613440901748822931 ) ) ;
#34555 = VECTOR ( 'NONE', #37184, 1000.000000000000114 ) ;
#34556 = EDGE_CURVE ( 'NONE', #17440, #20104, #10699, .T. ) ;
#34557 = CARTESIAN_POINT ( 'NONE',  ( 16.47043538305651467, -24.28946016894538573, -13.29763944434255230 ) ) ;
#34558 = CARTESIAN_POINT ( 'NONE',  ( 5.187504188494417079, 36.60991850771481637, 7.000000000000000000 ) ) ;
#34559 = DIRECTION ( 'NONE',  ( 0.8090169943749497827, 0.5877852522924698064, 0.000000000000000000 ) ) ;
#34560 = ORIENTED_EDGE ( 'NONE', *, *, #17836, .T. ) ;
#34561 = CARTESIAN_POINT ( 'NONE',  ( -12.40803774861176301, 20.46798912209962396, -19.49944249956930875 ) ) ;
#34562 = AXIS2_PLACEMENT_3D ( 'NONE', #32128, #4292, #453 ) ;
#34563 = CARTESIAN_POINT ( 'NONE',  ( -25.04152548477492957, -24.48861404543249165, 17.92354375535250810 ) ) ;
#34564 = CARTESIAN_POINT ( 'NONE',  ( 9.617438996837455178, -18.47535938133117739, -26.83658795940344177 ) ) ;
#34565 = LINE ( 'NONE', #16075, #17291 ) ;
#34566 = EDGE_LOOP ( 'NONE', ( #3768, #28680 ) ) ;
#34567 = ORIENTED_EDGE ( 'NONE', *, *, #31491, .F. ) ;
#34568 = CARTESIAN_POINT ( 'NONE',  ( -10.16947320689176060, 18.25185904155808103, -26.74100241956728397 ) ) ;
#34569 = CARTESIAN_POINT ( 'NONE',  ( -6.557822374958138134, 35.99981354310120452, 10.49999999999999822 ) ) ;
#34570 = FACE_BOUND ( 'NONE', #1226, .T. ) ;
#34571 = CARTESIAN_POINT ( 'NONE',  ( -34.54759111898754753, -10.75241469091295166, -8.455612022062105382 ) ) ;
#34572 = CARTESIAN_POINT ( 'NONE',  ( -15.32303194119059420, -26.70022385808693954, -5.000000000000000888 ) ) ;
#34573 = VECTOR ( 'NONE', #33572, 1000.000000000000000 ) ;
#34574 = LINE ( 'NONE', #26021, #28728 ) ;
#34575 = ORIENTED_EDGE ( 'NONE', *, *, #38359, .T. ) ;
#34576 = CARTESIAN_POINT ( 'NONE',  ( 30.70345270623383627, 0.1631843812369964675, -5.000000000000000000 ) ) ;
#34577 = CARTESIAN_POINT ( 'NONE',  ( 12.65336495406848627, 21.05333586960627557, -18.45227025400517462 ) ) ;
#34578 = CARTESIAN_POINT ( 'NONE',  ( 5.440908595777814050, 35.94977745735560859, 7.000000000000000000 ) ) ;
#34579 = EDGE_CURVE ( 'NONE', #24416, #38300, #38537, .T. ) ;
#34580 = EDGE_LOOP ( 'NONE', ( #18803, #29429, #36147, #22429, #5652, #22369 ) ) ;
#34581 = CARTESIAN_POINT ( 'NONE',  ( -22.73727917875568494, 0.5890566990126905322, -21.61446420491581577 ) ) ;
#34582 = ORIENTED_EDGE ( 'NONE', *, *, #38667, .F. ) ;
#34583 = CARTESIAN_POINT ( 'NONE',  ( 32.55122689258003987, -2.282376514339032436, -6.834113689379055501 ) ) ;
#34584 = CIRCLE ( 'NONE', #9303, 1.000000000000001110 ) ;
#34585 = DIRECTION ( 'NONE',  ( 1.000000000000000000, 0.000000000000000000, 0.000000000000000000 ) ) ;
#34586 = CARTESIAN_POINT ( 'NONE',  ( 34.35058160601991517, -9.363338975648222373, 17.42190598798392642 ) ) ;
#34587 = ORIENTED_EDGE ( 'NONE', *, *, #38286, .T. ) ;
#34588 = LINE ( 'NONE', #19146, #33842 ) ;
#34589 = CARTESIAN_POINT ( 'NONE',  ( 1.254079983865269199, 28.18681535329830368, 21.00000000000000355 ) ) ;
#34590 = CIRCLE ( 'NONE', #3445, 1.000000000000000000 ) ;
#34591 = ADVANCED_FACE ( 'NONE', ( #5432 ), #29509, .T. ) ;
#34592 = DIRECTION ( 'NONE',  ( -0.5720614028176770338, 0.4156269377774552409, -0.7071067811865524577 ) ) ;
#34593 = AXIS2_PLACEMENT_3D ( 'NONE', #23512, #27163, #17434 ) ;
#34594 = CARTESIAN_POINT ( 'NONE',  ( -11.48173768534023154, 32.16538668264431777, 10.49999999999999822 ) ) ;
#34595 = VECTOR ( 'NONE', #34843, 1000.000000000000000 ) ;
#34596 = EDGE_CURVE ( 'NONE', #17719, #4586, #31275, .T. ) ;
#34597 = CARTESIAN_POINT ( 'NONE',  ( 18.69515074622073314, 22.45407711374831194, 11.55979286841757414 ) ) ;
#34598 = CARTESIAN_POINT ( 'NONE',  ( -18.95922262551748361, 7.795319610833783663, -29.42417138239890306 ) ) ;
#34599 = EDGE_CURVE ( 'NONE', #13849, #26235, #12631, .T. ) ;
#34600 = CARTESIAN_POINT ( 'NONE',  ( 24.04485151285368616, -26.41317262118404940, -6.755592305404338305 ) ) ;
#34601 = CARTESIAN_POINT ( 'NONE',  ( -20.71631403513654845, -29.20819834831656436, -13.99845199583660182 ) ) ;
#34602 = CARTESIAN_POINT ( 'NONE',  ( 12.54609464142508735, 21.21266715414756732, -18.42867748839541875 ) ) ;
#34603 = AXIS2_PLACEMENT_3D ( 'NONE', #4476, #4677, #16881 ) ;
#34604 = ORIENTED_EDGE ( 'NONE', *, *, #24651, .T. ) ;
#34605 = CARTESIAN_POINT ( 'NONE',  ( -15.92491312827927885, 24.45805589641368982, -7.366686510344703898 ) ) ;
#34606 = CARTESIAN_POINT ( 'NONE',  ( -24.31339772227793716, -19.97941014234552881, 20.25080042701540961 ) ) ;
#34607 = STYLED_ITEM ( 'NONE', ( #13199 ), #36190 ) ;
#34608 = DIRECTION ( 'NONE',  ( 1.000000000000000000, 0.000000000000000000, 0.000000000000000000 ) ) ;
#34609 = CARTESIAN_POINT ( 'NONE',  ( 14.04669866214605456, 23.89545579451645452, -13.51503478317237317 ) ) ;
#34610 = ORIENTED_EDGE ( 'NONE', *, *, #35998, .T. ) ;
#34611 = DIRECTION ( 'NONE',  ( 0.000000000000000000, 0.000000000000000000, 1.000000000000000000 ) ) ;
#34612 = EDGE_LOOP ( 'NONE', ( #24225, #8316, #34377, #460 ) ) ;
#34614 = DIRECTION ( 'NONE',  ( 1.000000000000000000, 0.000000000000000000, 0.000000000000000000 ) ) ;
#34613 = CARTESIAN_POINT ( 'NONE',  ( -13.07870427894834719, 22.47409269205623161, -16.41433171529514112 ) ) ;
#34615 = CARTESIAN_POINT ( 'NONE',  ( -15.70264670462719714, -26.79635097760029794, -5.473156990174284253 ) ) ;
#34616 = CARTESIAN_POINT ( 'NONE',  ( 37.48557158514988430, -11.25000000000009237, 6.000000000000000000 ) ) ;
#34617 = EDGE_LOOP ( 'NONE', ( #39835, #26724, #8760, #13336 ) ) ;
#34618 = CARTESIAN_POINT ( 'NONE',  ( -32.79891082816697434, -15.91098148179321115, -9.730420382999001916 ) ) ;
#34619 = CARTESIAN_POINT ( 'NONE',  ( -10.37379948539326513, -20.61367283351156487, -20.63258827435396014 ) ) ;
#34620 = LINE ( 'NONE', #26070, #29991 ) ;
#34621 = CARTESIAN_POINT ( 'NONE',  ( 13.66197743094250328, 18.08662167453329062, -20.78650099872353962 ) ) ;
#34622 = ORIENTED_EDGE ( 'NONE', *, *, #19795, .T. ) ;
#34623 = CARTESIAN_POINT ( 'NONE',  ( 20.11222822097500540, 5.219997522146664792, -26.51068987014358669 ) ) ;
#34624 = CARTESIAN_POINT ( 'NONE',  ( -13.63581098909220479, 27.45627467658446008, 11.00000000000000000 ) ) ;
#34625 = EDGE_CURVE ( 'NONE', #11714, #1404, #25701, .T. ) ;
#34626 = DIRECTION ( 'NONE',  ( 1.000000000000000000, 0.000000000000000000, 0.000000000000000000 ) ) ;
#34627 = ADVANCED_FACE ( 'NONE', ( #38095 ), #34458, .F. ) ;
#34628 = CARTESIAN_POINT ( 'NONE',  ( -12.11431921870781281, -16.53859995802357474, -30.00000000000001066 ) ) ;
#34629 = ORIENTED_EDGE ( 'NONE', *, *, #957, .F. ) ;
#34630 = CARTESIAN_POINT ( 'NONE',  ( -31.23446777708887367, -0.4277017081496246598, -5.940776528115775612 ) ) ;
#34631 = CARTESIAN_POINT ( 'NONE',  ( 20.98375128680927659, 0.6676899881307120088, -26.21249548520855299 ) ) ;
#34632 = AXIS2_PLACEMENT_3D ( 'NONE', #4157, #16562, #6597 ) ;
#34633 = CARTESIAN_POINT ( 'NONE',  ( 16.80389827882015297, -21.64427909825937490, 19.99202127657103389 ) ) ;
#34634 = ORIENTED_EDGE ( 'NONE', *, *, #2395, .T. ) ;
#34635 = CARTESIAN_POINT ( 'NONE',  ( -19.54664213359414404, -11.28525909758381651, -19.69475445967427163 ) ) ;
#34636 = PRESENTATION_LAYER_ASSIGNMENT (  '', '', ( #9960 ) ) ;
#34637 = CARTESIAN_POINT ( 'NONE',  ( 9.819582157326484761, 24.63911342745429778, 10.50000000000000533 ) ) ;
#34638 = ORIENTED_EDGE ( 'NONE', *, *, #5247, .F. ) ;
#34639 = DIRECTION ( 'NONE',  ( -0.9510565162951538642, -0.3090169943749466186, -0.000000000000000000 ) ) ;
#34640 = EDGE_CURVE ( 'NONE', #25412, #29091, #8105, .T. ) ;
#34641 = CIRCLE ( 'NONE', #17151, 1.000000000000000000 ) ;
#34642 = CARTESIAN_POINT ( 'NONE',  ( -75.15099915297791711, 43.38844959084113384, 23.00000000000000000 ) ) ;
#34643 = DIRECTION ( 'NONE',  ( -0.4067366430757884399, 0.9135454576426061957, 1.040834085586084414E-14 ) ) ;
#34644 = CARTESIAN_POINT ( 'NONE',  ( 4.827317721685941976, 36.15751965146608171, -9.299952781395255386 ) ) ;
#34645 = CARTESIAN_POINT ( 'NONE',  ( 0.000000000000000000, 22.50000000000000355, 10.00000000000000000 ) ) ;
#34646 = CARTESIAN_POINT ( 'NONE',  ( 3.597409820281487480, 14.42008525284347087, 9.000000000000001776 ) ) ;
#34647 = B_SPLINE_CURVE_WITH_KNOTS ( 'NONE', 3,
 ( #35912, #20075, #26155, #17029, #29409, #13969 ),
 .UNSPECIFIED., .F., .F.,
 ( 4, 2, 4 ),
 ( 0.000000000000000000, 0.5000000000000000000, 1.000000000000000000 ),
 .UNSPECIFIED. ) ;
#34648 = CARTESIAN_POINT ( 'NONE',  ( 0.6417673702184640838, 33.31072022568110924, 12.00000000000000000 ) ) ;
#34649 = CARTESIAN_POINT ( 'NONE',  ( 14.36830325120613594, 20.48707633493483371, 7.000000000000000000 ) ) ;
#34650 = CARTESIAN_POINT ( 'NONE',  ( -8.505700342264141511, 22.10876900990917804, 9.000000000000001776 ) ) ;
#34651 = CARTESIAN_POINT ( 'NONE',  ( -24.90379269097766368, 23.90674680237738770, 9.500000000000000000 ) ) ;
#34652 = CARTESIAN_POINT ( 'NONE',  ( 14.27905419341862192, 25.65267611664213732, -11.54866840426435992 ) ) ;
#34653 = CARTESIAN_POINT ( 'NONE',  ( -6.972208014302417212, 35.78128242463058228, 7.339470489435489853 ) ) ;
#34654 = ORIENTED_EDGE ( 'NONE', *, *, #28957, .T. ) ;
#34656 = LINE ( 'NONE', #11228, #27194 ) ;
#34655 = CARTESIAN_POINT ( 'NONE',  ( -18.21453708440813912, 18.61006694202274403, -6.921138814994913346 ) ) ;
#34657 = CIRCLE ( 'NONE', #32045, 0.5000000000000004441 ) ;
#34658 = CARTESIAN_POINT ( 'NONE',  ( 13.30786737960926480, 15.60542992190359435, 10.49999999999999822 ) ) ;
#34659 = CARTESIAN_POINT ( 'NONE',  ( 14.03725205635479512, -24.61054561307185296, -12.55068749160697017 ) ) ;
#34660 = DIRECTION ( 'NONE',  ( -1.000000000000000000, 0.000000000000000000, 0.000000000000000000 ) ) ;
#34661 = CARTESIAN_POINT ( 'NONE',  ( 11.69083868191524544, 18.90691405789837276, -22.73601728422654844 ) ) ;
#34662 = ORIENTED_EDGE ( 'NONE', *, *, #6198, .T. ) ;
#34663 = CARTESIAN_POINT ( 'NONE',  ( 15.39245740739416668, 26.77485551171135114, -5.945824311378989258 ) ) ;
#34664 = B_SPLINE_SURFACE_WITH_KNOTS ( 'NONE', 3, 3, ( 
 ( #20053, #28785, #7038, #7237, #31830, #960, #558, #22680, #13337, #25731, #10299, #16603, #13542, #1359, #13743, #4202, #7650, #25331, #35083, #32448, #19637, #12940, #29588, #4808, #5605 ),
 ( #39130, #1766, #17623, #17213, #38735, #27148, #8253, #11511, #14553, #30199, #14150, #17822, #32854, #29387, #8662, #5006, #26341, #36096, #39533, #32652, #17419, #14353, #20662, #11110, #26549 ),
 ( #39334, #33061, #11710, #26947, #5210, #38935, #2372, #8049, #10915, #14757, #26743, #29794, #23299, #23896, #35692, #1977, #24097, #36492, #20254, #35891, #21054, #7847, #5410, #23494, #20459 ),
 ( #11314, #23697, #33463, #29993, #2169, #36299, #8461, #1563, #13947, #20860, #33262, #33658, #11907, #28135, #12303, #21838, #30798, #3353, #8861, #34044, #18210, #27543, #21445, #24490, #30991 ),
 ( #33851, #9460, #6203, #15153, #3160, #2760, #5809, #24690, #6395, #39928, #27938, #9060, #12105, #25088, #37087, #12498, #312, #36890, #24890, #22040, #37284, #37485, #36696, #9256, #21641 ),
 ( #30602, #34438, #112, #5999, #27738, #21248, #18406, #34241, #2962, #18802, #15349, #31187, #15745, #9662, #40125, #12694, #15551, #18606, #18013, #30405, #39732, #2570, #14955, #27343, #24298 ),
 ( #19796, #16757, #22833, #16551, #38074, #29138, #4146, #13285, #22228, #32191, #25475, #3551, #7391, #3947, #10049, #15950, #28933, #28330, #22427, #4350, #1311, #37682, #13085, #35233, #510 ),
 ( #34633, #1112, #12894, #34832, #25287, #10656, #706, #28730, #28533, #37874, #13692, #26080, #38481, #22631, #6784, #9850, #23037, #909, #10450, #19387, #6588, #19190, #35038, #31578, #16148 ),
 ( #3744, #6981, #18995, #31784, #38281, #7190, #16346, #19589, #25681, #10246, #31980, #31384, #13489, #25881, #26494, #32600, #2318, #14301, #29939, #17771, #1720, #2119, #39485, #14501, #14707 ),
 ( #26291, #10859, #35643, #26892, #29742, #7999, #38888, #23448, #29541, #35838, #20203, #1924, #4555, #35440, #30147, #39081, #36250, #20001, #39281, #38686, #27096, #11664, #33010, #26692, #23248 ),
 ( #23648, #7802, #36044, #11460, #20808, #7597, #32401, #16958, #20409, #4759, #17166, #29339, #14097, #11063, #23847, #1511, #32804, #17567, #13901, #4962, #17370, #11259, #8206, #20611, #5159 ),
 ( #8414, #5357, #33208, #39684, #17962, #34192, #18353, #27889, #36837, #9407, #14908, #40075, #24246, #33605, #27490, #30553, #37037, #36441, #2711, #30749, #15102, #6345, #11855, #15503, #39875 ),
 ( #12449, #21200, #33994, #12051, #5756, #31142, #2908, #18552, #18752, #24442, #30944, #28084, #3109, #3305, #2519, #15299, #27687, #27296, #18162, #36642, #263, #5952, #8811, #9007, #21397 ),
 ( #9207, #6151, #12251, #24840, #8607, #33803, #61, #30351, #24049, #24641, #21591, #21004, #37238, #21787, #15695, #33410, #5553, #22585, #34586, #31931, #31536, #7141, #13442, #19748, #25238 ),
 ( #12650, #32141, #16099, #9609, #19343, #22783, #15900, #28484, #37826, #31735, #6737, #28287, #19144, #37435, #16297, #6541, #38235, #7341, #29089, #25038, #13040, #37638, #464, #18946, #12848 ),
 ( #28886, #9805, #3702, #28684, #4303, #16706, #25836, #22184, #658, #34390, #21990, #25429, #10000, #10406, #22378, #34785, #31334, #6936, #1062, #859, #3900, #3505, #13239, #35185, #25630 ),
 ( #38028, #10202, #34992, #19541, #4100, #16504, #32553, #23795, #16911, #32955, #20154, #17718, #4711, #20558, #26642, #11412, #5111, #36196, #29889, #23600, #39031, #7949, #11209, #1264, #20359 ),
 ( #19952, #32754, #4909, #32349, #38635, #4508, #5308, #23398, #1464, #29293, #10810, #17317, #1875, #14251, #35997, #29691, #2071, #26035, #13848, #17518, #7550, #13647, #26240, #23196, #38434 ),
 ( #11013, #35594, #8153, #7751, #10607, #39233, #14447, #26842, #8362, #20762, #17115, #33156, #29491, #22988, #35392, #1667, #14047, #26439, #38838, #35793, #33555, #15049, #9509, #11806, #33358 ),
 ( #364, #21889, #12945, #28187, #37338, #5501, #3605, #8759, #27046, #31439, #27987, #9713, #37736, #8556, #34293, #6447, #20951, #27242, #17914, #34686, #12551, #30298, #2469, #39630, #18851 ),
 ( #39431, #30094, #25336, #31241, #16001, #14656, #22093, #14857, #9905, #12745, #2268, #6641, #11612, #161, #24192, #3403, #36589, #23995, #28386, #15798, #25139, #37539, #562, #21148, #19047 ),
 ( #5704, #34491, #36392, #18114, #30502, #22286, #2662, #24942, #6839, #32452, #29392, #35495, #29195, #10504, #1568, #16811, #25933, #34889, #4613, #38130, #16201, #20059, #16606, #22683, #28587 ),
 ( #31635, #19641, #3999, #7041, #13141, #19440, #31834, #38533, #13951, #16399, #1364, #25531, #35087, #759, #23303, #13343, #1164, #963, #25734, #17013, #26346, #38739, #35289, #28789, #37933 ),
 ( #7447, #10302, #10102, #38333, #10920, #22482, #7240, #13546, #32036, #4205, #28989, #35699, #22884, #10709, #19855, #32244, #4409, #13747, #26138, #23093, #7655, #19240, #3803, #39134, #5009 ),
 ( #30201, #33264, #14558, #5413, #7852, #26951, #14957, #17218, #32858, #32657, #21056, #18016, #24100, #17825, #39338, #30409, #2375, #11514, #23498, #33466, #26746, #4812, #8664, #5214, #11318 ) ),
 .UNSPECIFIED., .F., .F., .F.,
 ( 4, 3, 3, 3, 3, 3, 3, 3, 4 ),
 ( 4, 3, 3, 3, 3, 3, 3, 3, 4 ),
 ( 0.000000000000000000, 0.1250000000000000000, 0.2500000000000000000, 0.3750000000000000000, 0.5000000000000000000, 0.6250000000000000000, 0.7500000000000000000, 0.8750000000000000000, 1.000000000000000000 ),
 ( 4.459899766721566294, 4.784821457936500266, 5.109743149151433350, 5.434664840366366434, 5.759586531581300406, 6.084508222796233490, 6.409429914011166574, 6.734351605226100546, 7.059273296441033629 ),
 .UNSPECIFIED. ) ;
#34665 = ORIENTED_EDGE ( 'NONE', *, *, #39973, .T. ) ;
#34666 = CARTESIAN_POINT ( 'NONE',  ( -8.339609403135950672, 11.87216320208450959, 10.00000000000000000 ) ) ;
#34667 = CARTESIAN_POINT ( 'NONE',  ( -10.17999638199554191, -19.18007577932459284, -23.85944600179882258 ) ) ;
#34668 = CARTESIAN_POINT ( 'NONE',  ( -18.85268948302541148, -29.14375172063097352, 12.73282698324892692 ) ) ;
#34669 = CIRCLE ( 'NONE', #5464, 1.000000000000000000 ) ;
#34670 = CARTESIAN_POINT ( 'NONE',  ( -24.19767885117807538, -17.81929995649669252, -15.70298923897014198 ) ) ;
#34671 = CARTESIAN_POINT ( 'NONE',  ( -2.147850760800578129, -22.42921841763291724, -18.01282657023325484 ) ) ;
#34672 = CARTESIAN_POINT ( 'NONE',  ( 14.82034775369615964, 24.19848967327653000, -11.62209634349768628 ) ) ;
#34673 = VERTEX_POINT ( 'NONE', #9682 ) ;
#34674 = CARTESIAN_POINT ( 'NONE',  ( 22.00908396029312541, 11.01115965060166246, -8.406495840388641838 ) ) ;
#34675 = LINE ( 'NONE', #3001, #30334 ) ;
#34676 = CARTESIAN_POINT ( 'NONE',  ( 14.00263291006742605, 28.07534605034063446, 17.42190598798543633 ) ) ;
#34677 = ORIENTED_EDGE ( 'NONE', *, *, #3423, .F. ) ;
#34678 = CARTESIAN_POINT ( 'NONE',  ( -22.05094372219451415, -2.678342847933831816, -23.46479902602865053 ) ) ;
#34679 = EDGE_CURVE ( 'NONE', #1586, #3451, #23690, .T. ) ;
#34680 = CIRCLE ( 'NONE', #8082, 1.000000000000000000 ) ;
#34681 = CARTESIAN_POINT ( 'NONE',  ( -15.26743640742121677, 21.18345451744725594, 17.92354375535531830 ) ) ;
#34682 = ORIENTED_EDGE ( 'NONE', *, *, #26974, .T. ) ;
#34683 = DIRECTION ( 'NONE',  ( 0.000000000000000000, 0.000000000000000000, 1.000000000000000000 ) ) ;
#34684 = CARTESIAN_POINT ( 'NONE',  ( -20.39124144463984223, 2.214395427629727298, -29.37149834407417259 ) ) ;
#34685 = CARTESIAN_POINT ( 'NONE',  ( 19.34370528778291742, -8.503836621211386060, -26.28178913655981930 ) ) ;
#34686 = CARTESIAN_POINT ( 'NONE',  ( 36.56052011373606092, -7.179325806536988708, 13.92931973827813330 ) ) ;
#34687 = ORIENTED_EDGE ( 'NONE', *, *, #28780, .F. ) ;
#34688 = ORIENTED_EDGE ( 'NONE', *, *, #20961, .F. ) ;
#34689 = FACE_OUTER_BOUND ( 'NONE', #36092, .T. ) ;
#34690 = CARTESIAN_POINT ( 'NONE',  ( -0.8333333333333351467, 37.00000000000000711, 10.66666666666666607 ) ) ;
#34691 = ADVANCED_FACE ( 'NONE', ( #13107 ), #129, .T. ) ;
#34692 = FACE_OUTER_BOUND ( 'NONE', #22016, .T. ) ;
#34693 = ORIENTED_EDGE ( 'NONE', *, *, #34881, .T. ) ;
#34694 = ADVANCED_FACE ( 'NONE', ( #18626 ), #34263, .T. ) ;
#34695 = CARTESIAN_POINT ( 'NONE',  ( -0.6184052358777115677, 31.36018214284430528, -14.72953287677156098 ) ) ;
#34696 = DIRECTION ( 'NONE',  ( 0.2079116908177532363, -0.9781476007338070211, 0.000000000000000000 ) ) ;
#34697 = CARTESIAN_POINT ( 'NONE',  ( -12.30736835487442882, 14.81698729810789672, 7.000000000000000000 ) ) ;
#34698 = AXIS2_PLACEMENT_3D ( 'NONE', #6606, #3573, #19209 ) ;
#34699 = DIRECTION ( 'NONE',  ( 0.000000000000000000, 0.000000000000000000, 1.000000000000000000 ) ) ;
#34700 = FACE_OUTER_BOUND ( 'NONE', #16989, .T. ) ;
#34701 = DIRECTION ( 'NONE',  ( 0.000000000000000000, 0.000000000000000000, 1.000000000000000000 ) ) ;
#34702 = CARTESIAN_POINT ( 'NONE',  ( 10.70304607406188957, 23.48154281829076595, -18.10851452067850786 ) ) ;
#34704 = AXIS2_PLACEMENT_3D ( 'NONE', #35504, #10717, #1576 ) ;
#34703 = LINE ( 'NONE', #6856, #21793 ) ;
#34705 = ORIENTED_EDGE ( 'NONE', *, *, #24763, .F. ) ;
#34706 = ADVANCED_FACE ( 'NONE', ( #35054 ), #31598, .T. ) ;
#34708 = CARTESIAN_POINT ( 'NONE',  ( 7.419976537719617404, 10.58597682645822324, 10.50000000000000000 ) ) ;
#34707 = CARTESIAN_POINT ( 'NONE',  ( -18.03820307373585763, 9.850268257550711226, -28.29906855951537992 ) ) ;
#34709 = DIRECTION ( 'NONE',  ( 1.000000000000000000, 0.000000000000000000, 0.000000000000000000 ) ) ;
#34710 = CARTESIAN_POINT ( 'NONE',  ( 14.68418499867856752, -25.47351336547173162, -10.64941713223110220 ) ) ;
#34711 = DIRECTION ( 'NONE',  ( 0.3090169943749448977, -0.9510565162951543083, 0.000000000000000000 ) ) ;
#34712 = CARTESIAN_POINT ( 'NONE',  ( 15.39300221565557436, 26.86528302342467001, -5.000000000000000000 ) ) ;
#34713 = CARTESIAN_POINT ( 'NONE',  ( 12.33616729053617966, -27.99489201236593416, -13.58461195433497437 ) ) ;
#34714 = CARTESIAN_POINT ( 'NONE',  ( 9.427394962683440127, 11.06314620782477753, 10.49999999999999822 ) ) ;
#34715 = CARTESIAN_POINT ( 'NONE',  ( -16.01205366299697630, -16.95014973935591485, -22.09595210912920749 ) ) ;
#34716 = CARTESIAN_POINT ( 'NONE',  ( 7.804347359704323139, -23.94321386332827117, -12.77188294322276718 ) ) ;
#34717 = CARTESIAN_POINT ( 'NONE',  ( 11.11086231965098037, 17.28031181392691806, -28.71129638840202247 ) ) ;
#34718 = CARTESIAN_POINT ( 'NONE',  ( 17.15651132827482073, -12.35653875792482381, -26.27594141802030236 ) ) ;
#34719 = CARTESIAN_POINT ( 'NONE',  ( -13.36146265112639675, 15.68301270189280672, 7.445905703748357141 ) ) ;
#34720 = CARTESIAN_POINT ( 'NONE',  ( 5.537830610278449583, 36.16746786612485920, 10.94387467463502439 ) ) ;
#34722 = ORIENTED_EDGE ( 'NONE', *, *, #189, .T. ) ;
#34721 = EDGE_CURVE ( 'NONE', #10357, #32704, #3180, .T. ) ;
#34723 = CARTESIAN_POINT ( 'NONE',  ( -8.445470182190037534, 36.08267608658951531, -5.870491325241125935 ) ) ;
#34724 = ADVANCED_FACE ( 'NONE', ( #15968 ), #16169, .F. ) ;
#34725 = EDGE_CURVE ( 'NONE', #15697, #28039, #15570, .T. ) ;
#34726 = VECTOR ( 'NONE', #31265, 1000.000000000000114 ) ;
#34727 = DIRECTION ( 'NONE',  ( -0.000000000000000000, -0.000000000000000000, -1.000000000000000000 ) ) ;
#34728 = VERTEX_POINT ( 'NONE', #25307 ) ;
#34729 = CARTESIAN_POINT ( 'NONE',  ( 30.92038317698504457, -0.05869178374276581150, -5.474212382471533189 ) ) ;
#34730 = CARTESIAN_POINT ( 'NONE',  ( 6.354454053420411697, 35.54304081427980577, 11.00000000000000000 ) ) ;
#34731 = CARTESIAN_POINT ( 'NONE',  ( -7.577547685840081648, 11.84256962714647798, 13.00000000000000178 ) ) ;
#34732 = B_SPLINE_CURVE_WITH_KNOTS ( 'NONE', 3,
 ( #22240, #21850, #9674, #3757, #16359, #15757 ),
 .UNSPECIFIED., .F., .F.,
 ( 4, 2, 4 ),
 ( 0.000000000000000000, 0.5000000000000000000, 1.000000000000000000 ),
 .UNSPECIFIED. ) ;
#34733 = ORIENTED_EDGE ( 'NONE', *, *, #1611, .F. ) ;
#34734 = CARTESIAN_POINT ( 'NONE',  ( -30.67041884990485912, 0.02637635525178676568, -6.888046746717600755 ) ) ;
#34735 = FACE_OUTER_BOUND ( 'NONE', #8233, .T. ) ;
#34736 = ORIENTED_EDGE ( 'NONE', *, *, #25148, .F. ) ;
#34737 = CARTESIAN_POINT ( 'NONE',  ( 24.34023952209733110, -5.793758624890436693, -19.88440862677620657 ) ) ;
#34738 = AXIS2_PLACEMENT_3D ( 'NONE', #33071, #39544, #30006 ) ;
#34739 = AXIS2_PLACEMENT_3D ( 'NONE', #20937, #15036, #39616 ) ;
#34740 = EDGE_LOOP ( 'NONE', ( #26440, #32947, #7017 ) ) ;
#34741 = CARTESIAN_POINT ( 'NONE',  ( 10.89111091687317234, 36.83121428896964744, 10.99999999999999822 ) ) ;
#34742 = CARTESIAN_POINT ( 'NONE',  ( -1.829593030691901284E-15, 22.50000000000001066, 2.999999999999999112 ) ) ;
#34743 = CARTESIAN_POINT ( 'NONE',  ( 6.677405195727081022, 35.94657184102473479, 10.49999999999999645 ) ) ;
#34744 = EDGE_CURVE ( 'NONE', #16887, #15951, #8466, .T. ) ;
#34745 = CARTESIAN_POINT ( 'NONE',  ( -1.015221176887233153E-13, 34.78122644969442945, 19.27171037444156454 ) ) ;
#34746 = FACE_OUTER_BOUND ( 'NONE', #15525, .T. ) ;
#34747 = ORIENTED_EDGE ( 'NONE', *, *, #21043, .T. ) ;
#34748 = EDGE_CURVE ( 'NONE', #28039, #6207, #24956, .T. ) ;
#34749 = DIRECTION ( 'NONE',  ( 1.000000000000000000, 0.000000000000000000, 0.000000000000000000 ) ) ;
#34750 = CARTESIAN_POINT ( 'NONE',  ( -20.49397253890219162, -0.8422648960003168428, -30.00000000000000000 ) ) ;
#34751 = CARTESIAN_POINT ( 'NONE',  ( 12.47908909340999273, 14.17675236482283907, 7.338691926023210854 ) ) ;
#34752 = DIRECTION ( 'NONE',  ( 0.000000000000000000, 0.000000000000000000, 1.000000000000000000 ) ) ;
#34753 = CARTESIAN_POINT ( 'NONE',  ( 17.78493189837258370, 18.49202968733743546, -9.833181245109440027 ) ) ;
#34754 = CARTESIAN_POINT ( 'NONE',  ( 5.827110988097120803, 22.69265212915571439, -22.03187520749546735 ) ) ;
#34755 = ORIENTED_EDGE ( 'NONE', *, *, #6937, .T. ) ;
#34756 = CARTESIAN_POINT ( 'NONE',  ( 13.87211275201727112, -23.13071640756154679, -15.36481742136717266 ) ) ;
#34757 = CARTESIAN_POINT ( 'NONE',  ( -1.082972213713691678, 27.41125570341915818, 20.99999999999999645 ) ) ;
#34758 = VECTOR ( 'NONE', #6321, 1000.000000000000000 ) ;
#34759 = DIRECTION ( 'NONE',  ( -1.000000000000000000, 0.000000000000000000, 0.000000000000000000 ) ) ;
#34760 = ORIENTED_EDGE ( 'NONE', *, *, #4912, .F. ) ;
#34761 = AXIS2_PLACEMENT_3D ( 'NONE', #19658, #6116, #981 ) ;
#34762 = CARTESIAN_POINT ( 'NONE',  ( -12.94403022599198572, 21.62758146855915342, -17.44036610145013810 ) ) ;
#34763 = AXIS2_PLACEMENT_3D ( 'NONE', #11979, #27022, #23574 ) ;
#34764 = CARTESIAN_POINT ( 'NONE',  ( -17.31264644459998792, -26.16430884515780164, 17.42190598798388379 ) ) ;
#34765 = CARTESIAN_POINT ( 'NONE',  ( 9.645968088698525733, -18.94145075774736853, -25.05036544634032936 ) ) ;
#34766 = CIRCLE ( 'NONE', #34139, 0.5000000000000004441 ) ;
#34767 = DIRECTION ( 'NONE',  ( 0.000000000000000000, 0.000000000000000000, 1.000000000000000000 ) ) ;
#34768 = ORIENTED_EDGE ( 'NONE', *, *, #39580, .F. ) ;
#34769 = VERTEX_POINT ( 'NONE', #15765 ) ;
#34770 = CARTESIAN_POINT ( 'NONE',  ( -9.094450958252869199, 19.08085575228837882, -26.00957991712340700 ) ) ;
#34771 = CARTESIAN_POINT ( 'NONE',  ( -18.54826655067808261, -24.72227202651984967, -12.26027862526460233 ) ) ;
#34772 = FACE_BOUND ( 'NONE', #21005, .T. ) ;
#34773 = CARTESIAN_POINT ( 'NONE',  ( -34.72733857347371611, -7.593160847666269753, -7.191374443180106546 ) ) ;
#34774 = DIRECTION ( 'NONE',  ( 1.000000000000000000, 0.000000000000000000, 0.000000000000000000 ) ) ;
#34775 = ORIENTED_EDGE ( 'NONE', *, *, #26727, .F. ) ;
#34776 = CARTESIAN_POINT ( 'NONE',  ( 26.38915501620417459, 0.4550379995760640561, -15.46437747621563119 ) ) ;
#34777 = DIRECTION ( 'NONE',  ( 0.000000000000000000, 0.000000000000000000, 1.000000000000000000 ) ) ;
#34778 = CARTESIAN_POINT ( 'NONE',  ( 15.00000000000000000, 22.50000000000000711, 7.000000000000000000 ) ) ;
#34779 = EDGE_CURVE ( 'NONE', #19849, #23702, #27572, .T. ) ;
#34780 = ORIENTED_EDGE ( 'NONE', *, *, #18060, .T. ) ;
#34781 = CARTESIAN_POINT ( 'NONE',  ( -30.74697722743434980, -0.05262810487881691701, -6.887199586812257301 ) ) ;
#34782 = ORIENTED_EDGE ( 'NONE', *, *, #17564, .T. ) ;
#34783 = CARTESIAN_POINT ( 'NONE',  ( 29.91755462158655732, -1.203610591981010947, -11.48839126716891990 ) ) ;
#34784 = CARTESIAN_POINT ( 'NONE',  ( -2.118678732975735279, 7.827785988993307242, 6.000000000000000000 ) ) ;
#34785 = CARTESIAN_POINT ( 'NONE',  ( 35.17699530642156702, -14.40920341950727668, 16.30093088680190760 ) ) ;
#34786 = ORIENTED_EDGE ( 'NONE', *, *, #3206, .F. ) ;
#34787 = CARTESIAN_POINT ( 'NONE',  ( 14.95773623273977293, 28.45553334945067903, 16.30093088680319369 ) ) ;
#34788 = AXIS2_PLACEMENT_3D ( 'NONE', #9980, #638, #22561 ) ;
#34789 = DIRECTION ( 'NONE',  ( -0.3090169943749448977, 0.9510565162951543083, 0.000000000000000000 ) ) ;
#34790 = CARTESIAN_POINT ( 'NONE',  ( -0.7155976380802748782, 29.10878045366047928, 20.94377226548378346 ) ) ;
#34791 = CIRCLE ( 'NONE', #3012, 1.000000000000007772 ) ;
#34792 = CARTESIAN_POINT ( 'NONE',  ( -13.53057405073934838, 22.08338764125508291, 10.00000000000000000 ) ) ;
#34793 = VECTOR ( 'NONE', #22705, 1000.000000000000000 ) ;
#34794 = CARTESIAN_POINT ( 'NONE',  ( 13.62967667376826419, 40.40898974728997217, 11.00000000000000000 ) ) ;
#34795 = FACE_BOUND ( 'NONE', #17817, .T. ) ;
#34796 = CARTESIAN_POINT ( 'NONE',  ( 20.57776646309868340, 11.88057900679090473, 17.42190598798392998 ) ) ;
#34797 = CARTESIAN_POINT ( 'NONE',  ( -22.33456346850416452, 9.678077167578175377, -10.87421464888676148 ) ) ;
#34798 = CARTESIAN_POINT ( 'NONE',  ( 16.51057184612255213, -20.52216718775187942, -17.97160528296034698 ) ) ;
#34799 = DIRECTION ( 'NONE',  ( 1.000000000000000000, 0.000000000000000000, 0.000000000000000000 ) ) ;
#34800 = CARTESIAN_POINT ( 'NONE',  ( 13.69960780509116915, 23.55256641442795384, -14.45987690255760505 ) ) ;
#34801 = ORIENTED_EDGE ( 'NONE', *, *, #14799, .T. ) ;
#34802 = CARTESIAN_POINT ( 'NONE',  ( -11.71642904664754070, 16.82516707186347915, -29.99999999999999645 ) ) ;
#34803 = CARTESIAN_POINT ( 'NONE',  ( -28.87886496472023623, -7.891943102185759784, 20.25080042701591765 ) ) ;
#34804 = CARTESIAN_POINT ( 'NONE',  ( 10.69300419909370525, 32.80084059136112984, 10.87262190629272318 ) ) ;
#34805 = CARTESIAN_POINT ( 'NONE',  ( 13.23742591511837396, 22.18590334729812241, -16.44840566425442319 ) ) ;
#34806 = ORIENTED_EDGE ( 'NONE', *, *, #26846, .T. ) ;
#34807 = CARTESIAN_POINT ( 'NONE',  ( 33.16930538569719999, -19.62507065308114917, -4.999999999999998224 ) ) ;
#34808 = PLANE ( 'NONE',  #21593 ) ;
#34809 = ORIENTED_EDGE ( 'NONE', *, *, #34478, .F. ) ;
#34811 = CARTESIAN_POINT ( 'NONE',  ( -9.608347198026816471, 2.148595524579384186, 11.00000000000000000 ) ) ;
#34810 = CARTESIAN_POINT ( 'NONE',  ( -14.91983404371026012, 26.71086695692340740, -8.742635573326502652 ) ) ;
#34812 = CARTESIAN_POINT ( 'NONE',  ( -16.73104734145491079, -26.99160526830743123, -5.933635577335993894 ) ) ;
#34813 = CARTESIAN_POINT ( 'NONE',  ( 12.64565515434632559, 14.62167732336930648, 10.82238861112336892 ) ) ;
#34814 = AXIS2_PLACEMENT_3D ( 'NONE', #9654, #28325, #21633 ) ;
#34815 = AXIS2_PLACEMENT_3D ( 'NONE', #1292, #28712, #12874 ) ;
#34816 = VERTEX_POINT ( 'NONE', #22060 ) ;
#34817 = CARTESIAN_POINT ( 'NONE',  ( -18.51592210607118716, -9.711178581313356872, -26.96926714808659042 ) ) ;
#34818 = CARTESIAN_POINT ( 'NONE',  ( -13.21459172491393552, -24.49299878754191795, -12.58080149311899198 ) ) ;
#34819 = CARTESIAN_POINT ( 'NONE',  ( 8.927394655428274817, 11.06314620770945290, 11.00000000000000000 ) ) ;
#34820 = CARTESIAN_POINT ( 'NONE',  ( 15.73060052599727499, 21.93190910970603369, -11.69130784369475151 ) ) ;
#34821 = ORIENTED_EDGE ( 'NONE', *, *, #11909, .T. ) ;
#34822 = CARTESIAN_POINT ( 'NONE',  ( 28.06893040263355132, 2.889919344811102686, -6.900211441879279484 ) ) ;
#34823 = EDGE_CURVE ( 'NONE', #27435, #38149, #14586, .T. ) ;
#34824 = CARTESIAN_POINT ( 'NONE',  ( 13.28401428810676066, 15.50858767547181394, 10.49999999999999822 ) ) ;
#34825 = CARTESIAN_POINT ( 'NONE',  ( 3.992867117591230919, 8.524771480177550487, 7.000000000000000000 ) ) ;
#34826 = CARTESIAN_POINT ( 'NONE',  ( -10.10646936306323518, 32.94553861768095970, 10.49999999999999822 ) ) ;
#34827 = B_SPLINE_CURVE_WITH_KNOTS ( 'NONE', 3,
 ( #16494, #19738, #22774, #38424, #25422, #26025, #10597, #16288, #34577, #22979, #34984, #849, #6727, #32132, #19136, #13229 ),
 .UNSPECIFIED., .F., .F.,
 ( 4, 2, 2, 2, 2, 2, 2, 4 ),
 ( 0.000000000000000000, 0.1249999999374999671, 0.2499999998749999341, 0.4999999997500000903, 0.6249999996875000852, 0.7499999996249999690, 0.8749999995624999638, 0.9999999994999999586 ),
 .UNSPECIFIED. ) ;
#34828 = VERTEX_POINT ( 'NONE', #29160 ) ;
#34829 = CARTESIAN_POINT ( 'NONE',  ( -30.75436569807116172, -0.2981417031064238499, -7.815382463431599369 ) ) ;
#34830 = CARTESIAN_POINT ( 'NONE',  ( 30.72321469840077057, -0.2642282358989092028, -7.816807012777728936 ) ) ;
#34831 = ADVANCED_FACE ( 'NONE', ( #4981 ), #4371, .F. ) ;
#34832 = CARTESIAN_POINT ( 'NONE',  ( 20.26242815737391822, -21.95648885305471865, 19.99202127657103034 ) ) ;
#34833 = EDGE_CURVE ( 'NONE', #33301, #30382, #35462, .T. ) ;
#34834 = EDGE_LOOP ( 'NONE', ( #20804, #26568, #9110, #27227 ) ) ;
#34835 = ADVANCED_FACE ( 'NONE', ( #14120 ), #13941, .T. ) ;
#34836 = CARTESIAN_POINT ( 'NONE',  ( 1.354211015180573125E-14, -26.63027081345975589, -13.39439507595156265 ) ) ;
#34837 = CARTESIAN_POINT ( 'NONE',  ( -14.47283171447380035, 21.48159823030330884, 11.00000000000000000 ) ) ;
#34838 = VERTEX_POINT ( 'NONE', #35860 ) ;
#34839 = LINE ( 'NONE', #2277, #22340 ) ;
#34840 = VECTOR ( 'NONE', #15689, 1000.000000000000114 ) ;
#34841 = VECTOR ( 'NONE', #31228, 1000.000000000000000 ) ;
#34842 = CARTESIAN_POINT ( 'NONE',  ( -11.47910261372038399, 31.49019768869758806, 10.49999999999999822 ) ) ;
#34843 = DIRECTION ( 'NONE',  ( 0.000000000000000000, 0.000000000000000000, 1.000000000000000000 ) ) ;
#34844 = CARTESIAN_POINT ( 'NONE',  ( 4.962866441237491877, 37.35289340691882387, -7.129294914047508591 ) ) ;
#34845 = CARTESIAN_POINT ( 'NONE',  ( 5.330070799514983193, 27.28854476845134513, 13.00000000000000178 ) ) ;
#34846 = VERTEX_POINT ( 'NONE', #32003 ) ;
#34847 = EDGE_CURVE ( 'NONE', #34128, #15652, #10051, .T. ) ;
#34848 = CARTESIAN_POINT ( 'NONE',  ( -6.807850151676340111, 35.76876263333496553, 10.49999999999999822 ) ) ;
#34849 = EDGE_CURVE ( 'NONE', #172, #25521, #7208, .T. ) ;
#34850 = CARTESIAN_POINT ( 'NONE',  ( 10.49474413300069386, 21.89971208337373554, 10.50000000000000000 ) ) ;
#34851 = CARTESIAN_POINT ( 'NONE',  ( 23.06200705786680416, -18.88129698918507415, -15.73662040745943003 ) ) ;
#34852 = AXIS2_PLACEMENT_3D ( 'NONE', #24938, #3601, #37331 ) ;
#34853 = PLANE ( 'NONE',  #10857 ) ;
#34854 = DIRECTION ( 'NONE',  ( -0.6691306063588671194, -0.7431448254773862505, 0.000000000000000000 ) ) ;
#34855 = LINE ( 'NONE', #7004, #10660 ) ;
#34856 = CARTESIAN_POINT ( 'NONE',  ( 15.22299664760056537, 27.42699395385487904, -5.471105699861996463 ) ) ;
#34857 = VECTOR ( 'NONE', #18622, 1000.000000000000000 ) ;
#34858 = CARTESIAN_POINT ( 'NONE',  ( 4.458865582155095986, 18.48521636184714012, 6.000000000000000000 ) ) ;
#34859 = ORIENTED_EDGE ( 'NONE', *, *, #10015, .T. ) ;
#34861 = DIRECTION ( 'NONE',  ( 1.000000000000000000, 0.000000000000000000, 0.000000000000000000 ) ) ;
#34860 = CARTESIAN_POINT ( 'NONE',  ( -14.82391975563179720, 16.62805930398341658, -20.93744056305393286 ) ) ;
#34862 = CARTESIAN_POINT ( 'NONE',  ( -13.64211604268330724, 20.79918788657763429, 6.000000000000000000 ) ) ;
#34863 = CARTESIAN_POINT ( 'NONE',  ( 9.503358897673383154, -18.21462823815905452, -28.70764644545398880 ) ) ;
#34864 = CARTESIAN_POINT ( 'NONE',  ( -19.48557158514988785, -11.24999999999987743, 10.00000000000000000 ) ) ;
#34865 = CARTESIAN_POINT ( 'NONE',  ( 13.77319500370393435, 23.38836931657196772, -14.47646253997055332 ) ) ;
#34866 = EDGE_LOOP ( 'NONE', ( #37739, #6717 ) ) ;
#34867 = CARTESIAN_POINT ( 'NONE',  ( 10.98205083975412322, 17.31024513893945382, -30.00000000000000000 ) ) ;
#34868 = ORIENTED_EDGE ( 'NONE', *, *, #22527, .T. ) ;
#34869 = CARTESIAN_POINT ( 'NONE',  ( 14.30862178846744825, 26.15670448022654782, 10.49999999999999822 ) ) ;
#34870 = CARTESIAN_POINT ( 'NONE',  ( -11.89641196761903963, -21.48543073582372998, -18.45346097597589718 ) ) ;
#34871 = CARTESIAN_POINT ( 'NONE',  ( -37.28086807198960884, -8.991428209509251701, 12.14047268033097282 ) ) ;
#34872 = CARTESIAN_POINT ( 'NONE',  ( -22.05632830934130340, -15.21062374720687060, -18.62788710975480200 ) ) ;
#34873 = CARTESIAN_POINT ( 'NONE',  ( -3.305456868217321986, -20.38071200921649861, -27.71575502845627170 ) ) ;
#34874 = CARTESIAN_POINT ( 'NONE',  ( 11.81735879387240828, 18.14739419313247382, -23.90372284723114049 ) ) ;
#34875 = ORIENTED_EDGE ( 'NONE', *, *, #27246, .F. ) ;
#34876 = CARTESIAN_POINT ( 'NONE',  ( 20.53826766272770143, 10.36318479709787077, -15.94093620634325070 ) ) ;
#34877 = DIRECTION ( 'NONE',  ( -0.000000000000000000, -0.000000000000000000, -1.000000000000000000 ) ) ;
#34878 = CARTESIAN_POINT ( 'NONE',  ( -14.52022913577126317, 28.28138333486104017, 16.87380292611391042 ) ) ;
#34879 = EDGE_LOOP ( 'NONE', ( #23338, #20602, #36143, #20639 ) ) ;
#34880 = CARTESIAN_POINT ( 'NONE',  ( -33.49006840691916409, -4.412792004044882255, -7.689682260392150859 ) ) ;
#34881 = EDGE_CURVE ( 'NONE', #18776, #11714, #20023, .T. ) ;
#34882 = CIRCLE ( 'NONE', #32272, 1.000000000000000000 ) ;
#34883 = CARTESIAN_POINT ( 'NONE',  ( -14.67741354589487734, 20.96472719010613872, 18.42518152272275955 ) ) ;
#34884 = ORIENTED_EDGE ( 'NONE', *, *, #36199, .F. ) ;
#34885 = DIRECTION ( 'NONE',  ( -0.000000000000000000, -0.000000000000000000, -1.000000000000000000 ) ) ;
#34886 = DIRECTION ( 'NONE',  ( -0.000000000000000000, -0.000000000000000000, -1.000000000000000000 ) ) ;
#34887 = CIRCLE ( 'NONE', #25136, 6.000000000000000000 ) ;
#34888 = CARTESIAN_POINT ( 'NONE',  ( 18.76590878806661067, -8.252041909800052366, -30.00000000000001421 ) ) ;
#34890 = CIRCLE ( 'NONE', #23203, 6.000000000000000000 ) ;
#34889 = CARTESIAN_POINT ( 'NONE',  ( 37.38745755834691664, -10.91949489986236799, 12.73282698324846862 ) ) ;
#34891 = EDGE_LOOP ( 'NONE', ( #10402, #15071, #1280, #31977 ) ) ;
#34892 = EDGE_LOOP ( 'NONE', ( #22082, #13712 ) ) ;
#34893 = DIRECTION ( 'NONE',  ( 0.000000000000000000, 0.000000000000000000, 1.000000000000000000 ) ) ;
#34894 = PLANE ( 'NONE',  #3909 ) ;
#34895 = FACE_OUTER_BOUND ( 'NONE', #14606, .T. ) ;
#34896 = ORIENTED_EDGE ( 'NONE', *, *, #29113, .T. ) ;
#34897 = CARTESIAN_POINT ( 'NONE',  ( -1.178190889608008218, 23.73120932599768551, -21.84293309001832739 ) ) ;
#34898 = CARTESIAN_POINT ( 'NONE',  ( -13.96115708084650464, 27.98552962950150302, 7.381627713044564665 ) ) ;
#34899 = PLANE ( 'NONE',  #4000 ) ;
#34900 = EDGE_CURVE ( 'NONE', #12932, #3455, #314, .T. ) ;
#34901 = VECTOR ( 'NONE', #9580, 1000.000000000000227 ) ;
#34902 = DIRECTION ( 'NONE',  ( 0.000000000000000000, 0.000000000000000000, 1.000000000000000000 ) ) ;
#34903 = CARTESIAN_POINT ( 'NONE',  ( -13.94482798346716201, 26.50521816028930644, 9.000000000000001776 ) ) ;
#34904 = CARTESIAN_POINT ( 'NONE',  ( -3.503793317224518145, 8.420815634768723967, 7.499999999999997335 ) ) ;
#34905 = VECTOR ( 'NONE', #25377, 1000.000000000000114 ) ;
#34906 = CARTESIAN_POINT ( 'NONE',  ( 13.56803016854205168, 27.21220305392325400, -11.44257138522273287 ) ) ;
#34907 = DIRECTION ( 'NONE',  ( 1.000000000000000000, 0.000000000000000000, 0.000000000000000000 ) ) ;
#34908 = VECTOR ( 'NONE', #23840, 1000.000000000000000 ) ;
#34909 = ORIENTED_EDGE ( 'NONE', *, *, #24863, .F. ) ;
#34911 = DIRECTION ( 'NONE',  ( 0.000000000000000000, 0.000000000000000000, 1.000000000000000000 ) ) ;
#34910 = CARTESIAN_POINT ( 'NONE',  ( -19.69150485828470920, 15.64879689043717192, -5.481634527261435075 ) ) ;
#34912 = CARTESIAN_POINT ( 'NONE',  ( 3.357189294653307954, 32.49896394832310165, 10.50000000000000000 ) ) ;
#34913 = CARTESIAN_POINT ( 'NONE',  ( 13.06130030674361819, -23.09502941311707147, -15.44577141088513272 ) ) ;
#34914 = CARTESIAN_POINT ( 'NONE',  ( 3.057264508911339274, 12.92643568347968674, 10.49999999999999467 ) ) ;
#34915 = CARTESIAN_POINT ( 'NONE',  ( 11.14895963631104969, 17.78189646060649309, -26.22104407627368161 ) ) ;
#34916 = VECTOR ( 'NONE', #29944, 1000.000000000000000 ) ;
#34917 = CARTESIAN_POINT ( 'NONE',  ( -11.10756861982300947, 19.59949212537556562, -29.99999999999999645 ) ) ;
#34918 = DIRECTION ( 'NONE',  ( -0.000000000000000000, 1.000000000000000000, -0.000000000000000000 ) ) ;
#34919 = AXIS2_PLACEMENT_3D ( 'NONE', #31879, #10547, #35331 ) ;
#34920 = CARTESIAN_POINT ( 'NONE',  ( -16.57717488103276438, -16.52257091567909342, -22.04563894478580721 ) ) ;
#34921 = CARTESIAN_POINT ( 'NONE',  ( 7.020580985973422727, -19.34222023316537786, -28.79039117229796219 ) ) ;
#34922 = CARTESIAN_POINT ( 'NONE',  ( 15.47833181635298772, 26.56067009156167558, -5.474148242754607985 ) ) ;
#34923 = CARTESIAN_POINT ( 'NONE',  ( 30.14705489269769956, -20.42482444568447519, -9.731448662954948148 ) ) ;
#34924 = CARTESIAN_POINT ( 'NONE',  ( 13.67111072870491206, 27.95752071293676266, 10.49999999999999822 ) ) ;
#34925 = DIRECTION ( 'NONE',  ( -0.8090169943749426773, 0.5877852522924797984, 0.000000000000000000 ) ) ;
#34926 = ORIENTED_EDGE ( 'NONE', *, *, #37728, .F. ) ;
#34927 = CARTESIAN_POINT ( 'NONE',  ( -5.778086282686619946, 24.63158676520072987, -19.78736581433748398 ) ) ;
#34928 = EDGE_CURVE ( 'NONE', #9701, #13281, #35255, .T. ) ;
#34929 = CARTESIAN_POINT ( 'NONE',  ( 14.31603901957230462, 19.98981538725069740, 7.500000000000010658 ) ) ;
#34930 = EDGE_LOOP ( 'NONE', ( #20206, #8782 ) ) ;
#34931 = CARTESIAN_POINT ( 'NONE',  ( 29.62952841301010665, 0.01294893774858196268, -10.17754520856805911 ) ) ;
#34932 = EDGE_CURVE ( 'NONE', #11008, #21646, #15245, .T. ) ;
#34933 = CARTESIAN_POINT ( 'NONE',  ( -0.5000000000000004441, 37.00000000000000711, 7.000000000000000000 ) ) ;
#34934 = DIRECTION ( 'NONE',  ( -0.000000000000000000, -0.000000000000000000, -1.000000000000000000 ) ) ;
#34935 = VERTEX_POINT ( 'NONE', #1132 ) ;
#34936 = CARTESIAN_POINT ( 'NONE',  ( -21.70210997138368469, 0.7650954235519592528, -23.85841552861994330 ) ) ;
#34937 = CARTESIAN_POINT ( 'NONE',  ( -18.98517864320375281, -25.27528660476427547, -11.33194675972254650 ) ) ;
#34938 = ORIENTED_EDGE ( 'NONE', *, *, #6213, .F. ) ;
#34939 = CARTESIAN_POINT ( 'NONE',  ( 25.27050923793063220, -6.013975129722774149, -18.85480297636462055 ) ) ;
#34940 = AXIS2_PLACEMENT_3D ( 'NONE', #10151, #22523, #12987 ) ;
#34941 = ADVANCED_FACE ( 'NONE', ( #26102 ), #38299, .F. ) ;
#34942 = ORIENTED_EDGE ( 'NONE', *, *, #36169, .T. ) ;
#34943 = CARTESIAN_POINT ( 'NONE',  ( 7.591957726968737497, 38.93640765974105733, 11.55979286843916576 ) ) ;
#34944 = AXIS2_PLACEMENT_3D ( 'NONE', #33514, #12749, #18459 ) ;
#34945 = CYLINDRICAL_SURFACE ( 'NONE', #29398, 1.000000000000000000 ) ;
#34946 = CARTESIAN_POINT ( 'NONE',  ( -10.49474413300070097, 21.89971208337388120, 10.50000000000000000 ) ) ;
#34947 = CARTESIAN_POINT ( 'NONE',  ( -4.864422697792210926, 33.03032433378080412, 19.66345542862530849 ) ) ;
#34948 = CIRCLE ( 'NONE', #34852, 0.5000000000000004441 ) ;
#34949 = CARTESIAN_POINT ( 'NONE',  ( 3.503793317224329851, 8.420815634768676006, 7.000000000000000000 ) ) ;
#34950 = EDGE_LOOP ( 'NONE', ( #7813, #34782, #15642 ) ) ;
#34951 = CARTESIAN_POINT ( 'NONE',  ( 7.782590637173006698, 18.96886919491949897, -30.00000000000000355 ) ) ;
#34952 = MANIFOLD_SOLID_BREP ( 'Fill Pattern1', #7328 ) ;
#34953 = CYLINDRICAL_SURFACE ( 'NONE', #8507, 0.4999999999999995559 ) ;
#34954 = ADVANCED_FACE ( 'NONE', ( #1946 ), #9019, .F. ) ;
#34955 = EDGE_CURVE ( 'NONE', #6691, #4778, #26941, .T. ) ;
#34956 = CARTESIAN_POINT ( 'NONE',  ( -13.63581098909220479, 27.45627467658446008, 9.000000000000001776 ) ) ;
#34957 = EDGE_CURVE ( 'NONE', #7636, #22687, #2272, .T. ) ;
#34958 = CARTESIAN_POINT ( 'NONE',  ( 14.82374459613959949, 15.60418353992821849, -23.14626635614779460 ) ) ;
#34959 = CARTESIAN_POINT ( 'NONE',  ( 10.43807493394656660, 32.55179874717006783, -9.848587368490356653 ) ) ;
#34960 = ORIENTED_EDGE ( 'NONE', *, *, #20306, .F. ) ;
#34961 = CARTESIAN_POINT ( 'NONE',  ( 10.08241157172804670, -17.84938614438609505, -29.33613610785861781 ) ) ;
#34962 = CARTESIAN_POINT ( 'NONE',  ( 13.22516817658079802, 40.70288237343621063, 7.000000000000000000 ) ) ;
#34963 = CARTESIAN_POINT ( 'NONE',  ( 0.000000000000000000, 22.50000000000000355, 10.00000000000000000 ) ) ;
#34964 = AXIS2_PLACEMENT_3D ( 'NONE', #33993, #40074, #6150 ) ;
#34965 = ORIENTED_EDGE ( 'NONE', *, *, #11864, .T. ) ;
#34967 = VECTOR ( 'NONE', #12316, 1000.000000000000000 ) ;
#34966 = CARTESIAN_POINT ( 'NONE',  ( -10.99360060711668474, 17.30291464612033181, -29.99999999999999289 ) ) ;
#34968 = CARTESIAN_POINT ( 'NONE',  ( -17.09641143070615499, -27.64751350299154353, 15.72805884748921379 ) ) ;
#34969 = CARTESIAN_POINT ( 'NONE',  ( 15.01751060382407310, -26.59764153146664256, -5.946174819114761867 ) ) ;
#34970 = DIRECTION ( 'NONE',  ( -1.000000000000000000, 0.000000000000000000, 0.000000000000000000 ) ) ;
#34971 = ORIENTED_EDGE ( 'NONE', *, *, #22945, .T. ) ;
#34972 = ORIENTED_EDGE ( 'NONE', *, *, #22246, .T. ) ;
#34973 = CIRCLE ( 'NONE', #27176, 15.00000000000000000 ) ;
#34974 = CARTESIAN_POINT ( 'NONE',  ( -9.456804962331334607, 19.97028186113128356, -23.55775169706302208 ) ) ;
#34975 = CARTESIAN_POINT ( 'NONE',  ( 5.184280209938516570, 31.68549066217151733, 11.00000000000000000 ) ) ;
#34976 = EDGE_CURVE ( 'NONE', #35589, #12341, #5495, .T. ) ;
#34977 = LINE ( 'NONE', #32330, #19152 ) ;
#34978 = EDGE_CURVE ( 'NONE', #33679, #113, #5504, .T. ) ;
#34979 = CARTESIAN_POINT ( 'NONE',  ( -29.13564390960204165, -7.175030889379423016, -14.89359602007027483 ) ) ;
#34980 = CYLINDRICAL_SURFACE ( 'NONE', #20938, 0.5000000000000007772 ) ;
#34981 = ORIENTED_EDGE ( 'NONE', *, *, #35003, .F. ) ;
#34982 = CARTESIAN_POINT ( 'NONE',  ( 20.60096619578946076, 1.002830394841245587, -28.08503524805096063 ) ) ;
#34983 = EDGE_CURVE ( 'NONE', #747, #3751, #19604, .T. ) ;
#34984 = CARTESIAN_POINT ( 'NONE',  ( 11.89393184406004877, 19.38028971260454369, -21.61737903493217416 ) ) ;
#34985 = CARTESIAN_POINT ( 'NONE',  ( -5.767236651883568044, 13.71142893291686171, 10.00000000000000000 ) ) ;
#34986 = VERTEX_POINT ( 'NONE', #25906 ) ;
#34987 = CARTESIAN_POINT ( 'NONE',  ( -22.22060807504403002, 0.6658104290297893746, -22.73532940052641038 ) ) ;
#34988 = LINE ( 'NONE', #38429, #11161 ) ;
#34989 = ORIENTED_EDGE ( 'NONE', *, *, #29167, .T. ) ;
#34990 = CARTESIAN_POINT ( 'NONE',  ( 31.53325577840491434, -2.954393997327824817, -10.45565772087099710 ) ) ;
#34991 = CARTESIAN_POINT ( 'NONE',  ( 20.22742541439770392, -3.352094935268329134, -29.99999999999998579 ) ) ;
#34992 = CARTESIAN_POINT ( 'NONE',  ( 18.89973329987769901, -27.81027420697393993, 15.72805884748954064 ) ) ;
#34993 = ORIENTED_EDGE ( 'NONE', *, *, #18589, .F. ) ;
#34994 = CARTESIAN_POINT ( 'NONE',  ( 6.751265526280336715, 37.11581529111865763, 16.30093088680186497 ) ) ;
#34995 = B_SPLINE_CURVE_WITH_KNOTS ( 'NONE', 3,
 ( #9054, #37080, #40118, #21438, #12297, #9250, #34039, #6195, #18601, #15546, #25084, #10799, #9655, #31574, #14039, #38827, #18990, #34628 ),
 .UNSPECIFIED., .F., .F.,
 ( 4, 2, 2, 2, 2, 2, 2, 2, 4 ),
 ( 5.000000244656254402E-10, 0.1250000003749999478, 0.2500000002499999097, 0.3750000001249998438, 0.4999999999999997780, 0.6249999998749997676, 0.7499999997499998683, 0.8749999996249998580, 0.9999999994999999586 ),
 .UNSPECIFIED. ) ;
#34996 = LINE ( 'NONE', #28290, #13693 ) ;
#34997 = CARTESIAN_POINT ( 'NONE',  ( -5.870940266647052930, 25.61771140527362434, 20.94377226548378701 ) ) ;
#34998 = VECTOR ( 'NONE', #39499, 1000.000000000000000 ) ;
#34999 = LINE ( 'NONE', #38242, #9018 ) ;
#35000 = DIRECTION ( 'NONE',  ( 1.000000000000000000, 0.000000000000000000, 0.000000000000000000 ) ) ;
#35001 = CIRCLE ( 'NONE', #31747, 0.5000000000000005551 ) ;
#35002 = PRODUCT_DEFINITION_SHAPE ( 'NONE', 'NONE',  #40202 ) ;
#35003 = EDGE_CURVE ( 'NONE', #39848, #20455, #10719, .T. ) ;
#35004 = FACE_BOUND ( 'NONE', #8943, .T. ) ;
#35005 = CARTESIAN_POINT ( 'NONE',  ( 27.91036560780102604, 4.231346453961702281, 15.13084544680861221 ) ) ;
#35006 = CARTESIAN_POINT ( 'NONE',  ( -19.01510071548347369, 7.808900211911244504, -28.28496368704278652 ) ) ;
#35007 = CARTESIAN_POINT ( 'NONE',  ( 13.09734119108189532, -16.42133399325533105, -26.53413149736031684 ) ) ;
#35008 = CARTESIAN_POINT ( 'NONE',  ( -14.45127508551987994, 26.52006039836903284, 7.493552897947291846 ) ) ;
#35009 = ORIENTED_EDGE ( 'NONE', *, *, #13084, .F. ) ;
#35010 = CARTESIAN_POINT ( 'NONE',  ( 15.36061443993781062, 26.97785078317152596, -5.000000000000000888 ) ) ;
#35011 = ORIENTED_EDGE ( 'NONE', *, *, #33465, .F. ) ;
#35012 = CARTESIAN_POINT ( 'NONE',  ( -14.35436364106707607, 23.18990942748935069, -13.54973528055356624 ) ) ;
#35013 = CARTESIAN_POINT ( 'NONE',  ( -31.03731131718960157, -12.30244853585585041, 19.66345542862529783 ) ) ;
#35014 = FACE_OUTER_BOUND ( 'NONE', #28974, .T. ) ;
#35015 = CARTESIAN_POINT ( 'NONE',  ( 11.72828249552547142, 18.87102642502439664, -22.74204984032840926 ) ) ;
#35016 = EDGE_LOOP ( 'NONE', ( #35186, #15371, #9520 ) ) ;
#35017 = CARTESIAN_POINT ( 'NONE',  ( 18.24555790293216972, -9.366475481951450632, -30.00000000000002842 ) ) ;
#35018 = DIRECTION ( 'NONE',  ( 0.000000000000000000, 0.000000000000000000, 1.000000000000000000 ) ) ;
#35019 = EDGE_LOOP ( 'NONE', ( #14205, #11645, #7837, #19602, #15746 ) ) ;
#35021 = DIRECTION ( 'NONE',  ( 0.000000000000000000, 0.000000000000000000, 1.000000000000000000 ) ) ;
#35020 = CARTESIAN_POINT ( 'NONE',  ( -14.13481689797295715, 24.87588527889338863, -12.51643896934201372 ) ) ;
#35022 = CARTESIAN_POINT ( 'NONE',  ( -16.57759486525810999, -26.77642802984841808, -7.325415354228808518 ) ) ;
#35023 = DIRECTION ( 'NONE',  ( 0.000000000000000000, 0.000000000000000000, 1.000000000000000000 ) ) ;
#35024 = CIRCLE ( 'NONE', #24001, 1.000000000000004441 ) ;
#35025 = EDGE_LOOP ( 'NONE', ( #15938, #18053, #25611 ) ) ;
#35026 = CARTESIAN_POINT ( 'NONE',  ( -34.92155312733419237, -14.43004807528053135, -6.706874702558842216 ) ) ;
#35027 = CARTESIAN_POINT ( 'NONE',  ( -14.23983225781402595, -26.43328798539083735, -4.999999999999999112 ) ) ;
#35028 = DIRECTION ( 'NONE',  ( 0.000000000000000000, 0.000000000000000000, 1.000000000000000000 ) ) ;
#35029 = CARTESIAN_POINT ( 'NONE',  ( 16.28234317699659783, 22.93167278076970561, -8.327167766279165662 ) ) ;
#35030 = ORIENTED_EDGE ( 'NONE', *, *, #29476, .F. ) ;
#35031 = CARTESIAN_POINT ( 'NONE',  ( 28.20661398414674537, 2.887420757311715658, -5.000000000000000000 ) ) ;
#35032 = EDGE_CURVE ( 'NONE', #1897, #1674, #35262, .T. ) ;
#35033 = CYLINDRICAL_SURFACE ( 'NONE', #14170, 1.000000000000000000 ) ;
#35034 = CARTESIAN_POINT ( 'NONE',  ( -23.74914942275209384, -8.582573258223623824, 23.00000000000000000 ) ) ;
#35035 = ORIENTED_EDGE ( 'NONE', *, *, #5916, .T. ) ;
#35036 = CARTESIAN_POINT ( 'NONE',  ( -20.49328727640310888, 0.5260942599782587603, -29.34226995137056448 ) ) ;
#35037 = CARTESIAN_POINT ( 'NONE',  ( 31.56176620184661274, -0.7927402297087241534, -5.936147513203532178 ) ) ;
#35038 = CARTESIAN_POINT ( 'NONE',  ( 28.63944909880341072, -5.523819906327855911, 19.99202127657133232 ) ) ;
#35039 = EDGE_LOOP ( 'NONE', ( #26520, #21827, #6649, #22289 ) ) ;
#35040 = CARTESIAN_POINT ( 'NONE',  ( 13.28992586503610340, -18.25382200079949513, -29.99999999999999289 ) ) ;
#35041 = DIRECTION ( 'NONE',  ( 1.000000000000000000, 0.000000000000000000, 0.000000000000000000 ) ) ;
#35042 = DIRECTION ( 'NONE',  ( 1.000000000000000000, 0.000000000000000000, 0.000000000000000000 ) ) ;
#35043 = CARTESIAN_POINT ( 'NONE',  ( 0.000000000000000000, 22.50000000000000355, 7.000000000000000000 ) ) ;
#35044 = CARTESIAN_POINT ( 'NONE',  ( 3.211395437248501850, 12.61633075744433796, 6.000000000000000000 ) ) ;
#35045 = DIRECTION ( 'NONE',  ( -0.7431448254773862505, 0.6691306063588670083, 0.000000000000000000 ) ) ;
#35046 = EDGE_CURVE ( 'NONE', #6333, #3736, #19799, .T. ) ;
#35047 = ORIENTED_EDGE ( 'NONE', *, *, #29221, .T. ) ;
#35048 = DIRECTION ( 'NONE',  ( 1.000000000000000000, 0.000000000000000000, 0.000000000000000000 ) ) ;
#35049 = CARTESIAN_POINT ( 'NONE',  ( 3.992867117591230919, 8.524771480177550487, 10.49999999999999289 ) ) ;
#35050 = CARTESIAN_POINT ( 'NONE',  ( 16.18705333424930970, -13.20565027319068996, -27.01267265381389393 ) ) ;
#35051 = DIRECTION ( 'NONE',  ( 0.9135454576426059736, 0.4067366430757889395, -0.000000000000000000 ) ) ;
#35052 = FACE_OUTER_BOUND ( 'NONE', #10967, .T. ) ;
#35053 = CARTESIAN_POINT ( 'NONE',  ( 10.63119325176788088, 18.14365359947311873, -26.16532366619414418 ) ) ;
#35054 = FACE_OUTER_BOUND ( 'NONE', #3028, .T. ) ;
#35055 = ORIENTED_EDGE ( 'NONE', *, *, #19233, .T. ) ;
#35056 = CARTESIAN_POINT ( 'NONE',  ( -14.29743425985715355, 15.73966817516812888, -24.20757674709752649 ) ) ;
#35057 = DIRECTION ( 'NONE',  ( 1.000000000000000000, 0.000000000000000000, 0.000000000000000000 ) ) ;
#35058 = CARTESIAN_POINT ( 'NONE',  ( 14.58890700129304463, -25.45407539014443898, -10.65398993192215293 ) ) ;
#35059 = ADVANCED_FACE ( 'NONE', ( #4175 ), #38103, .T. ) ;
#35060 = CARTESIAN_POINT ( 'NONE',  ( 14.86556419889027048, 20.43481210330100240, 7.000000000000000000 ) ) ;
#35061 = CARTESIAN_POINT ( 'NONE',  ( 15.23445058273096464, 26.39864931307285900, -7.828033204951921675 ) ) ;
#35062 = ORIENTED_EDGE ( 'NONE', *, *, #2965, .F. ) ;
#35063 = CARTESIAN_POINT ( 'NONE',  ( 11.06818295498493576, 17.50574775501806357, -27.44742483198325189 ) ) ;
#35064 = VERTEX_POINT ( 'NONE', #19826 ) ;
#35066 = CARTESIAN_POINT ( 'NONE',  ( 14.03291393139918597, 26.53383901973350589, 10.99387789255784220 ) ) ;
#35065 = CARTESIAN_POINT ( 'NONE',  ( -11.42130609047572065, 18.49161963548644394, -23.84395533656347865 ) ) ;
#35067 = CARTESIAN_POINT ( 'NONE',  ( -9.469408548107701051, -18.18187935292228019, -30.00000000000000000 ) ) ;
#35068 = CARTESIAN_POINT ( 'NONE',  ( -22.67025966227462419, -28.72937007811335874, 13.32518128616567132 ) ) ;
#35069 = AXIS2_PLACEMENT_3D ( 'NONE', #8617, #15110, #24056 ) ;
#35070 = CARTESIAN_POINT ( 'NONE',  ( -22.98950691836191496, -13.88151727732919838, -18.61066130745788882 ) ) ;
#35071 = CARTESIAN_POINT ( 'NONE',  ( -3.533336070225259196, -21.04848782586652689, -23.28608928280259960 ) ) ;
#35072 = CARTESIAN_POINT ( 'NONE',  ( 14.58699662364080929, 23.73430093865497170, -12.57910105661215638 ) ) ;
#35073 = VERTEX_POINT ( 'NONE', #22459 ) ;
#35074 = CARTESIAN_POINT ( 'NONE',  ( 21.05083558980209801, 7.683405658820698036, -18.99948416535620765 ) ) ;
#35075 = AXIS2_PLACEMENT_3D ( 'NONE', #31847, #4009, #32048 ) ;
#35076 = CARTESIAN_POINT ( 'NONE',  ( 15.33540831873581212, 35.51988610398912272, 11.00000000000000000 ) ) ;
#35077 = CARTESIAN_POINT ( 'NONE',  ( -15.18941732005890266, -26.66619070650552459, -5.000000000000001776 ) ) ;
#35078 = CARTESIAN_POINT ( 'NONE',  ( 9.066401385853238182, 34.43014579340820092, 17.42190598798392998 ) ) ;
#35079 = ORIENTED_EDGE ( 'NONE', *, *, #6496, .F. ) ;
#35080 = CARTESIAN_POINT ( 'NONE',  ( -32.65566155904921430, -4.264910902414662530, -9.490589700126765393 ) ) ;
#35081 = CARTESIAN_POINT ( 'NONE',  ( -24.07200259734583270, 7.872448391864142359, 16.30093088680252578 ) ) ;
#35082 = ORIENTED_EDGE ( 'NONE', *, *, #34094, .F. ) ;
#35083 = CARTESIAN_POINT ( 'NONE',  ( 24.44578022397283945, -10.62045233751072004, 20.99999999999999645 ) ) ;
#35084 = DIRECTION ( 'NONE',  ( 0.000000000000000000, 0.000000000000000000, 1.000000000000000000 ) ) ;
#35085 = EDGE_CURVE ( 'NONE', #4444, #19049, #2955, .T. ) ;
#35086 = CARTESIAN_POINT ( 'NONE',  ( 34.30740497575424541, -16.27724728724163228, -7.121324501852425826 ) ) ;
#35087 = CARTESIAN_POINT ( 'NONE',  ( 35.02038065029451275, -20.21902619557050684, 12.14047268033097460 ) ) ;
#35088 = ORIENTED_EDGE ( 'NONE', *, *, #32736, .F. ) ;
#35089 = ORIENTED_EDGE ( 'NONE', *, *, #15247, .F. ) ;
#35090 = DIRECTION ( 'NONE',  ( 1.000000000000000000, 0.000000000000000000, 0.000000000000000000 ) ) ;
#35091 = CARTESIAN_POINT ( 'NONE',  ( -30.90412082983564446, -0.04211290444597337590, -5.000000000000000888 ) ) ;
#35092 = VECTOR ( 'NONE', #20371, 999.9999999999998863 ) ;
#35093 = CARTESIAN_POINT ( 'NONE',  ( 5.644276917315719899, 36.40655018617690786, 10.49999999999999822 ) ) ;
#35094 = ORIENTED_EDGE ( 'NONE', *, *, #8676, .F. ) ;
#35095 = CARTESIAN_POINT ( 'NONE',  ( -0.7518768309112285886, 38.37606218726813267, -6.275896992768287497 ) ) ;
#35096 = AXIS2_PLACEMENT_3D ( 'NONE', #31148, #28688, #6740 ) ;
#35097 = CARTESIAN_POINT ( 'NONE',  ( -0.3582326297815359162, 33.31072022568110924, 13.00000000000000178 ) ) ;
#35098 = CARTESIAN_POINT ( 'NONE',  ( 10.36702044712426840, 31.16169077310587809, 9.500000000000000000 ) ) ;
#35099 = CARTESIAN_POINT ( 'NONE',  ( 3.863783140547853712E-14, -86.77689918168233874, 2.999999999999999112 ) ) ;
#35101 = EDGE_CURVE ( 'NONE', #3204, #20104, #16176, .T. ) ;
#35100 = CARTESIAN_POINT ( 'NONE',  ( 2.525645716490518389, 8.212903943950921715, 7.499999999999990230 ) ) ;
#35102 = CARTESIAN_POINT ( 'NONE',  ( 2.629601561899395534, 7.723830143584016206, 10.49999999999999822 ) ) ;
#35103 = CARTESIAN_POINT ( 'NONE',  ( 11.49081439112069702, 22.60309983489513286, -18.22883438010077484 ) ) ;
#35104 = LINE ( 'NONE', #29, #5587 ) ;
#35105 = ORIENTED_EDGE ( 'NONE', *, *, #22999, .T. ) ;
#35107 = PLANE ( 'NONE',  #20039 ) ;
#35106 = CARTESIAN_POINT ( 'NONE',  ( -18.17263180773770159, 11.81850911556306372, -21.17646943544158944 ) ) ;
#35108 = CARTESIAN_POINT ( 'NONE',  ( -18.68934290552931543, 29.94321432092452895, 22.99999999999905853 ) ) ;
#35109 = CARTESIAN_POINT ( 'NONE',  ( 11.94195138395211941, -21.48248341615735768, -18.44782710392617631 ) ) ;
#35110 = ADVANCED_FACE ( 'NONE', ( #35468 ), #7458, .T. ) ;
#35111 = DIRECTION ( 'NONE',  ( -0.000000000000000000, -0.000000000000000000, 1.000000000000000000 ) ) ;
#35112 = CIRCLE ( 'NONE', #26027, 60.00000000000007816 ) ;
#35113 = CARTESIAN_POINT ( 'NONE',  ( 12.91186190338204298, 21.68060954549180863, -17.43383681951817721 ) ) ;
#35114 = CARTESIAN_POINT ( 'NONE',  ( -19.69645987729884595, 11.37175641224114919, -21.56489709563623691 ) ) ;
#35115 = CARTESIAN_POINT ( 'NONE',  ( -23.20062861290008627, -14.64054034232861135, 22.99999999999999645 ) ) ;
#35116 = CARTESIAN_POINT ( 'NONE',  ( -15.10985780742689499, -15.06563729506261851, -25.73346922605977127 ) ) ;
#35117 = CARTESIAN_POINT ( 'NONE',  ( 8.497644768481743327, -25.32189558139016228, -5.477296350422366622 ) ) ;
#35118 = CARTESIAN_POINT ( 'NONE',  ( 13.84574913428668275, 23.23330865849091253, -14.48585008083296266 ) ) ;
#35119 = CARTESIAN_POINT ( 'NONE',  ( 19.90145156205069554, 13.46129076908396627, -11.87680844943539249 ) ) ;
#35120 = CARTESIAN_POINT ( 'NONE',  ( -2.568190708544555445, 12.82247983807085134, 10.50000000000000533 ) ) ;
#35121 = CARTESIAN_POINT ( 'NONE',  ( 3.713592597587208832, 7.966960743906818188, 7.000000000000000000 ) ) ;
#35122 = ORIENTED_EDGE ( 'NONE', *, *, #6094, .T. ) ;
#35123 = CARTESIAN_POINT ( 'NONE',  ( -5.983447258044394701, 19.98291656352506251, -27.11177212607830000 ) ) ;
#35124 = EDGE_LOOP ( 'NONE', ( #22069, #21296 ) ) ;
#35125 = VECTOR ( 'NONE', #3814, 1000.000000000000000 ) ;
#35126 = LINE ( 'NONE', #12982, #114 ) ;
#35127 = ORIENTED_EDGE ( 'NONE', *, *, #1324, .F. ) ;
#35128 = CARTESIAN_POINT ( 'NONE',  ( 22.73483984765169197, 0.5967685963425408691, -21.61569754599228688 ) ) ;
#35129 = AXIS2_PLACEMENT_3D ( 'NONE', #5657, #20517, #30657 ) ;
#35130 = CARTESIAN_POINT ( 'NONE',  ( -14.26377478793851061, 19.49255443956674583, 7.000000000000000000 ) ) ;
#35131 = EDGE_CURVE ( 'NONE', #29462, #33574, #13719, .T. ) ;
#35132 = LINE ( 'NONE', #37776, #34905 ) ;
#35133 = EDGE_CURVE ( 'NONE', #11406, #17826, #15270, .T. ) ;
#35134 = ORIENTED_EDGE ( 'NONE', *, *, #20126, .T. ) ;
#35135 = CARTESIAN_POINT ( 'NONE',  ( -29.66313021947697592, 0.1976963186581543463, -9.712199395440693550 ) ) ;
#35136 = CARTESIAN_POINT ( 'NONE',  ( -4.524139159579198655, 31.43208625488816566, 10.00000000000000000 ) ) ;
#35137 = EDGE_LOOP ( 'NONE', ( #24193, #38180, #28124 ) ) ;
#35138 = CARTESIAN_POINT ( 'NONE',  ( 31.89272422543808361, -8.553727179860587171, -12.07502465680937576 ) ) ;
#35139 = ORIENTED_EDGE ( 'NONE', *, *, #37446, .T. ) ;
#35140 = VECTOR ( 'NONE', #33347, 1000.000000000000114 ) ;
#35141 = CARTESIAN_POINT ( 'NONE',  ( 14.89626057892312616, 32.60452476689637535, 11.00000000000000000 ) ) ;
#35142 = CARTESIAN_POINT ( 'NONE',  ( 9.303655249773155944, 10.73386218874824216, 7.000000000000000000 ) ) ;
#35143 = DIRECTION ( 'NONE',  ( -0.9945218953682730678, 0.1045284632676563991, 0.000000000000000000 ) ) ;
#35144 = CARTESIAN_POINT ( 'NONE',  ( 2.660873612011785294, 34.56296969693364218, 19.27171037444156454 ) ) ;
#35145 = CARTESIAN_POINT ( 'NONE',  ( -1.605702774688126722, 27.44183462127829642, 6.000000000000000000 ) ) ;
#35146 = VERTEX_POINT ( 'NONE', #7416 ) ;
#35147 = CARTESIAN_POINT ( 'NONE',  ( 0.4281292814599761409, 20.49824620653738450, -30.00000000000000000 ) ) ;
#35148 = LINE ( 'NONE', #16667, #2710 ) ;
#35149 = DIRECTION ( 'NONE',  ( -0.2079116908177663092, -0.9781476007338041345, 0.000000000000000000 ) ) ;
#35150 = ADVANCED_FACE ( 'NONE', ( #37904 ), #536, .F. ) ;
#35151 = CARTESIAN_POINT ( 'NONE',  ( 17.69882028648708783, 20.03130879389887298, -5.955324216395004200 ) ) ;
#35152 = CARTESIAN_POINT ( 'NONE',  ( 8.855091917839381210, 30.59299078850003539, -13.02531624040802072 ) ) ;
#35153 = AXIS2_PLACEMENT_3D ( 'NONE', #12758, #3617, #16013 ) ;
#35154 = ORIENTED_EDGE ( 'NONE', *, *, #26694, .F. ) ;
#35155 = DIRECTION ( 'NONE',  ( 0.000000000000000000, 0.000000000000000000, 1.000000000000000000 ) ) ;
#35156 = DIRECTION ( 'NONE',  ( -0.000000000000000000, -0.000000000000000000, -1.000000000000000000 ) ) ;
#35157 = CARTESIAN_POINT ( 'NONE',  ( 10.14866111327665266, -18.21960830426016997, -26.79090690569056221 ) ) ;
#35158 = CARTESIAN_POINT ( 'NONE',  ( -2.525645716490710679, 8.212903943950959018, 7.499999999999997335 ) ) ;
#35159 = DIRECTION ( 'NONE',  ( 1.000000000000000000, 0.000000000000000000, 0.000000000000000000 ) ) ;
#35160 = ORIENTED_EDGE ( 'NONE', *, *, #14006, .F. ) ;
#35161 = CARTESIAN_POINT ( 'NONE',  ( -14.29967717032973518, 24.44936570868513215, -12.55117429398542939 ) ) ;
#35162 = CARTESIAN_POINT ( 'NONE',  ( -22.28718831901767317, -26.62569216358780011, 16.87380292611400989 ) ) ;
#35163 = CARTESIAN_POINT ( 'NONE',  ( 14.06663363425422908, -25.35442907823021130, -10.66521829186682702 ) ) ;
#35164 = VECTOR ( 'NONE', #23895, 1000.000000000000000 ) ;
#35165 = DIRECTION ( 'NONE',  ( -0.3583679495453008790, 0.9335804264972015210, 0.000000000000000000 ) ) ;
#35166 = ORIENTED_EDGE ( 'NONE', *, *, #8732, .F. ) ;
#35167 = ORIENTED_EDGE ( 'NONE', *, *, #21207, .T. ) ;
#35168 = CARTESIAN_POINT ( 'NONE',  ( -10.84898765319574743, 23.30394029384613575, -18.13347752456717998 ) ) ;
#35169 = FACE_OUTER_BOUND ( 'NONE', #34612, .T. ) ;
#35170 = DIRECTION ( 'NONE',  ( 0.000000000000000000, 0.000000000000000000, 1.000000000000000000 ) ) ;
#35171 = CIRCLE ( 'NONE', #12457, 6.000000000000001776 ) ;
#35172 = CARTESIAN_POINT ( 'NONE',  ( -32.40829156996449711, -7.016000414201827518, -11.20844734717147162 ) ) ;
#35173 = CARTESIAN_POINT ( 'NONE',  ( 4.524139159579314118, 31.43208625488810171, 10.49999999999999822 ) ) ;
#35174 = ORIENTED_EDGE ( 'NONE', *, *, #5073, .T. ) ;
#35175 = CARTESIAN_POINT ( 'NONE',  ( 29.86380350792722282, 0.1690758829598159041, -9.240701576314629406 ) ) ;
#35176 = CARTESIAN_POINT ( 'NONE',  ( 2.871201846650637268, 31.30332840660451765, 6.000000000000000000 ) ) ;
#35177 = DIRECTION ( 'NONE',  ( 1.000000000000000000, 0.000000000000000000, 0.000000000000000000 ) ) ;
#35178 = ORIENTED_EDGE ( 'NONE', *, *, #4712, .T. ) ;
#35179 = CARTESIAN_POINT ( 'NONE',  ( -30.91582600597228137, -0.05403808547916690019, -5.474125485033605187 ) ) ;
#35180 = CYLINDRICAL_SURFACE ( 'NONE', #33901, 6.000000000000000888 ) ;
#35182 = EDGE_CURVE ( 'NONE', #7898, #12750, #26961, .T. ) ;
#35181 = ORIENTED_EDGE ( 'NONE', *, *, #25127, .F. ) ;
#35183 = CARTESIAN_POINT ( 'NONE',  ( 32.52266725778360268, -3.089069589389634274, -8.625450327480431056 ) ) ;
#35184 = CARTESIAN_POINT ( 'NONE',  ( 0.6108529249776364356, 37.48755679569042343, 7.000000000000000000 ) ) ;
#35185 = CARTESIAN_POINT ( 'NONE',  ( 32.12208287522988570, -1.273987114062791859, 16.30093088680380120 ) ) ;
#35186 = ORIENTED_EDGE ( 'NONE', *, *, #1227, .T. ) ;
#35187 = CARTESIAN_POINT ( 'NONE',  ( 15.42165057838460029, 26.78649484830278027, 16.30093088680190050 ) ) ;
#35188 = CARTESIAN_POINT ( 'NONE',  ( -14.81329996725647469, 19.93755115561707569, 10.49999999999999467 ) ) ;
#35189 = CARTESIAN_POINT ( 'NONE',  ( 0.7155976380801669645, 29.10878045366049349, 20.94377226548378346 ) ) ;
#35190 = DIRECTION ( 'NONE',  ( -0.8660254037844432595, -0.4999999999999921729, 0.000000000000000000 ) ) ;
#35191 = CIRCLE ( 'NONE', #8609, 0.5000000000000002220 ) ;
#35192 = DIRECTION ( 'NONE',  ( 1.000000000000000000, 0.000000000000000000, 0.000000000000000000 ) ) ;
#35193 = EDGE_CURVE ( 'NONE', #17610, #29868, #38305, .T. ) ;
#35194 = CONICAL_SURFACE ( 'NONE', #12522, 0.9999999999999991118, 0.7853981633974502774 ) ;
#35195 = FACE_BOUND ( 'NONE', #13380, .T. ) ;
#35196 = EDGE_CURVE ( 'NONE', #25273, #15130, #1009, .T. ) ;
#35197 = CARTESIAN_POINT ( 'NONE',  ( 16.37862447359607287, 21.59537890659658288, 16.87380292610781396 ) ) ;
#35198 = CARTESIAN_POINT ( 'NONE',  ( -19.10455879864122153, 7.830559145427559820, -27.15426290237969198 ) ) ;
#35199 = CARTESIAN_POINT ( 'NONE',  ( 13.39371427707866147, -15.78149709652679533, -27.86034563683584508 ) ) ;
#35200 = DIRECTION ( 'NONE',  ( -0.000000000000000000, -0.000000000000000000, -1.000000000000000000 ) ) ;
#35201 = CARTESIAN_POINT ( 'NONE',  ( 14.78333195896292729, 25.78429753009990577, -10.16969888846196568 ) ) ;
#35202 = VERTEX_POINT ( 'NONE', #31808 ) ;
#35203 = CARTESIAN_POINT ( 'NONE',  ( -12.04424134404128921, 16.72615764091300861, -28.13376640329193634 ) ) ;
#35204 = ADVANCED_FACE ( 'NONE', ( #3974 ), #28760, .F. ) ;
#35205 = CARTESIAN_POINT ( 'NONE',  ( -28.84864528223463864, -18.09713003384587182, 19.66345542862496387 ) ) ;
#35206 = CARTESIAN_POINT ( 'NONE',  ( -10.77091082532341204, 29.60251629318183575, 13.00000000000000178 ) ) ;
#35207 = CARTESIAN_POINT ( 'NONE',  ( 15.36863164365442103, 26.51124612085094867, -6.888122883055683765 ) ) ;
#35208 = VERTEX_POINT ( 'NONE', #10274 ) ;
#35209 = CARTESIAN_POINT ( 'NONE',  ( 18.76822264364483317, -10.35557248195002877, -25.57773590016846654 ) ) ;
#35210 = PLANE ( 'NONE',  #9270 ) ;
#35211 = EDGE_LOOP ( 'NONE', ( #14678, #25160 ) ) ;
#35213 = DIRECTION ( 'NONE',  ( 0.000000000000000000, 0.000000000000000000, 1.000000000000000000 ) ) ;
#35212 = CARTESIAN_POINT ( 'NONE',  ( -15.19876735762676034, 27.08650375569634861, -6.877893297480420109 ) ) ;
#35214 = CARTESIAN_POINT ( 'NONE',  ( -10.41468997611843506, -18.62962352831552693, -24.96183479470249367 ) ) ;
#35215 = LINE ( 'NONE', #23633, #9511 ) ;
#35216 = VECTOR ( 'NONE', #15710, 1000.000000000000000 ) ;
#35217 = VERTEX_POINT ( 'NONE', #35060 ) ;
#35218 = CARTESIAN_POINT ( 'NONE',  ( -35.38382356931356298, -13.39769055746643289, -5.438178884671905244 ) ) ;
#35219 = CARTESIAN_POINT ( 'NONE',  ( -14.09564871292362476, -26.21398149618797291, -7.362640844368039339 ) ) ;
#35220 = FACE_OUTER_BOUND ( 'NONE', #15791, .T. ) ;
#35221 = CARTESIAN_POINT ( 'NONE',  ( 13.32665242662786120, 15.89484158179648610, -27.00953544631929759 ) ) ;
#35222 = ORIENTED_EDGE ( 'NONE', *, *, #11723, .F. ) ;
#35223 = CARTESIAN_POINT ( 'NONE',  ( 28.20661398414674537, 2.887420757311715658, -5.474884631757898745 ) ) ;
#35224 = LINE ( 'NONE', #22828, #21309 ) ;
#35225 = AXIS2_PLACEMENT_3D ( 'NONE', #12474, #24868, #21618 ) ;
#35226 = CARTESIAN_POINT ( 'NONE',  ( 14.42035624161478857, 26.65972665747660031, 10.49999999999999822 ) ) ;
#35227 = EDGE_LOOP ( 'NONE', ( #30047, #19184, #14471, #1895 ) ) ;
#35228 = EDGE_CURVE ( 'NONE', #40197, #13640, #7215, .T. ) ;
#35229 = CARTESIAN_POINT ( 'NONE',  ( -30.99742014632522569, -0.1379718400911541798, -5.473566688364370769 ) ) ;
#35230 = EDGE_CURVE ( 'NONE', #26705, #32832, #36047, .T. ) ;
#35231 = CARTESIAN_POINT ( 'NONE',  ( 31.60127994866165224, -0.7964638025070726046, -5.000000000000000000 ) ) ;
#35232 = CIRCLE ( 'NONE', #20966, 0.5000000000000004441 ) ;
#35233 = CARTESIAN_POINT ( 'NONE',  ( 27.31543141964077037, -5.069059863653875730, 20.25080042701695859 ) ) ;
#35234 = ORIENTED_EDGE ( 'NONE', *, *, #13517, .T. ) ;
#35235 = CARTESIAN_POINT ( 'NONE',  ( -19.69645987729884595, 11.37175641224115097, -29.99999999999998934 ) ) ;
#35236 = AXIS2_PLACEMENT_3D ( 'NONE', #13709, #22446, #28750 ) ;
#35237 = CARTESIAN_POINT ( 'NONE',  ( -14.04783364825881975, 26.18819932152426233, 10.66666666666667140 ) ) ;
#35238 = VECTOR ( 'NONE', #14962, 1000.000000000000000 ) ;
#35239 = FACE_OUTER_BOUND ( 'NONE', #1904, .T. ) ;
#35240 = LINE ( 'NONE', #22435, #34048 ) ;
#35241 = AXIS2_PLACEMENT_3D ( 'NONE', #30556, #6154, #2716 ) ;
#35242 = ADVANCED_FACE ( 'NONE', ( #4584 ), #28896, .T. ) ;
#35243 = AXIS2_PLACEMENT_3D ( 'NONE', #29389, #10707, #26950 ) ;
#35244 = DIRECTION ( 'NONE',  ( -0.000000000000000000, -0.000000000000000000, -1.000000000000000000 ) ) ;
#35245 = DIRECTION ( 'NONE',  ( -0.3090169943749450643, 0.9510565162951544194, -0.000000000000000000 ) ) ;
#35246 = EDGE_CURVE ( 'NONE', #2697, #5248, #6083, .T. ) ;
#35247 = DIRECTION ( 'NONE',  ( -0.8090169943749505599, -0.5877852522924689183, 0.000000000000000000 ) ) ;
#35248 = VERTEX_POINT ( 'NONE', #39307 ) ;
#35249 = CARTESIAN_POINT ( 'NONE',  ( -6.856875760696268252, 35.58019112794178795, 10.49999999999999822 ) ) ;
#35250 = CARTESIAN_POINT ( 'NONE',  ( 10.41267482483262619, 26.20820393249957192, 6.000000000000000000 ) ) ;
#35251 = CARTESIAN_POINT ( 'NONE',  ( 16.57028389081698094, -14.37381587238541059, -24.32133266205364563 ) ) ;
#35252 = CARTESIAN_POINT ( 'NONE',  ( 4.118671991557230072, 37.17221401100731981, 6.000000000000000000 ) ) ;
#35253 = DIRECTION ( 'NONE',  ( -1.224646799147351235E-16, 1.000000000000000000, 0.000000000000000000 ) ) ;
#35254 = CARTESIAN_POINT ( 'NONE',  ( 15.20648748154197882, 27.39160813737696998, -5.939486291738587553 ) ) ;
#35255 = LINE ( 'NONE', #23668, #24328 ) ;
#35256 = B_SPLINE_CURVE_WITH_KNOTS ( 'NONE', 3,
 ( #6753, #34601, #25849, #1279 ),
 .UNSPECIFIED., .F., .F.,
 ( 4, 4 ),
 ( 0.000000000000000000, 1.000000000000000000 ),
 .UNSPECIFIED. ) ;
#35257 = ORIENTED_EDGE ( 'NONE', *, *, #21732, .F. ) ;
#35258 = AXIS2_PLACEMENT_3D ( 'NONE', #6299, #13399, #28841 ) ;
#35259 = CARTESIAN_POINT ( 'NONE',  ( -17.69219503082499756, 19.52419099561771176, -7.880095719941950350 ) ) ;
#35260 = CARTESIAN_POINT ( 'NONE',  ( -23.19735768193461567, -14.64350930037788068, 21.00000000000000000 ) ) ;
#35261 = CARTESIAN_POINT ( 'NONE',  ( 14.32771630080133463, -25.06525504208602939, -11.59986630204942060 ) ) ;
#35262 = LINE ( 'NONE', #13114, #8133 ) ;
#35263 = CARTESIAN_POINT ( 'NONE',  ( 15.18140632243098054, 26.25845010830521531, -8.297908434051732840 ) ) ;
#35264 = ORIENTED_EDGE ( 'NONE', *, *, #1631, .F. ) ;
#35265 = CARTESIAN_POINT ( 'NONE',  ( 14.28858787313288481, 24.47746469342002129, -12.55008231428947596 ) ) ;
#35266 = ORIENTED_EDGE ( 'NONE', *, *, #34679, .T. ) ;
#35268 = CARTESIAN_POINT ( 'NONE',  ( 4.100636323082810009, 29.29593658752792962, 6.000000000000000000 ) ) ;
#35267 = CARTESIAN_POINT ( 'NONE',  ( -10.94041201910780359, 17.33660477453622306, -29.99999999999999645 ) ) ;
#35269 = CARTESIAN_POINT ( 'NONE',  ( -15.47550425816466557, -26.73936689671932143, -5.000000000000000888 ) ) ;
#35270 = CARTESIAN_POINT ( 'NONE',  ( -26.42723928173377246, -27.79046472072431584, 12.14047268033097460 ) ) ;
#35271 = CARTESIAN_POINT ( 'NONE',  ( -32.64518230009728939, -19.71632926622226734, -7.116952983000433441 ) ) ;
#35272 = VECTOR ( 'NONE', #17531, 1000.000000000000114 ) ;
#35273 = CARTESIAN_POINT ( 'NONE',  ( -2.394825184670892781, -23.73107514896808112, -12.88530523879403944 ) ) ;
#35274 = CARTESIAN_POINT ( 'NONE',  ( 11.41005643133681957, 17.03110932016596735, -29.35731938081785941 ) ) ;
#35275 = ORIENTED_EDGE ( 'NONE', *, *, #16116, .F. ) ;
#35276 = CARTESIAN_POINT ( 'NONE',  ( 19.21215415183591446, 7.317176409479575483, -28.27861274171054973 ) ) ;
#35277 = CARTESIAN_POINT ( 'NONE',  ( 34.38704122072325475, -17.20178129237611842, -4.999999999999999112 ) ) ;
#35278 = FACE_OUTER_BOUND ( 'NONE', #23979, .T. ) ;
#35279 = CARTESIAN_POINT ( 'NONE',  ( 4.783493507397931666, 36.70021839994227975, 17.42190598798392998 ) ) ;
#35280 = ORIENTED_EDGE ( 'NONE', *, *, #22114, .F. ) ;
#35281 = CARTESIAN_POINT ( 'NONE',  ( -20.43418187165424982, -1.772479648697218302, -29.30004495981471990 ) ) ;
#35282 = CIRCLE ( 'NONE', #31388, 0.5000000000000004441 ) ;
#35283 = CARTESIAN_POINT ( 'NONE',  ( -8.859192577249674017, 12.20922670551869516, 20.99999999999999645 ) ) ;
#35284 = ORIENTED_EDGE ( 'NONE', *, *, #38192, .T. ) ;
#35285 = DIRECTION ( 'NONE',  ( 0.7431448254773954654, 0.6691306063588569053, -0.000000000000000000 ) ) ;
#35286 = DIRECTION ( 'NONE',  ( -0.2079116908177663092, -0.9781476007338040235, 0.000000000000000000 ) ) ;
#35287 = EDGE_CURVE ( 'NONE', #20607, #39797, #14327, .T. ) ;
#35288 = CARTESIAN_POINT ( 'NONE',  ( 24.72333287932298163, -9.962440173953478251, -18.66584102224920372 ) ) ;
#35289 = CARTESIAN_POINT ( 'NONE',  ( 34.78242786800331743, -1.681962577801997760, 12.14047268033102966 ) ) ;
#35290 =( REPRESENTATION_RELATIONSHIP ('NONE','NONE', #15382, #33787 ) REPRESENTATION_RELATIONSHIP_WITH_TRANSFORMATION ( #2027 )SHAPE_REPRESENTATION_RELATIONSHIP( ) );
#35291 = CIRCLE ( 'NONE', #15160, 1.000000000000000000 ) ;
#35292 = ORIENTED_EDGE ( 'NONE', *, *, #4049, .T. ) ;
#35293 = CARTESIAN_POINT ( 'NONE',  ( 12.49038105676653743, 14.13397459621550745, 11.00000000000000000 ) ) ;
#35294 = DIRECTION ( 'NONE',  ( 0.000000000000000000, -0.000000000000000000, -1.000000000000000000 ) ) ;
#35295 = LINE ( 'NONE', #7453, #36341 ) ;
#35296 = EDGE_LOOP ( 'NONE', ( #21635, #33232, #14696 ) ) ;
#35297 = CARTESIAN_POINT ( 'NONE',  ( -1.339087178513852283, 26.79985410012201541, -18.61668850162147848 ) ) ;
#35298 = DIRECTION ( 'NONE',  ( 1.000000000000000000, -1.734723475976802361E-14, 0.000000000000000000 ) ) ;
#35299 = CARTESIAN_POINT ( 'NONE',  ( -12.68475447279705648, 27.14725768220950286, 9.500000000000000000 ) ) ;
#35300 = DIRECTION ( 'NONE',  ( 1.000000000000000000, 0.000000000000000000, -0.000000000000000000 ) ) ;
#35301 = CYLINDRICAL_SURFACE ( 'NONE', #37900, 6.000000000000001776 ) ;
#35302 = DIRECTION ( 'NONE',  ( -0.6691306063588671194, -0.7431448254773861395, 0.000000000000000000 ) ) ;
#35303 = AXIS2_PLACEMENT_3D ( 'NONE', #22753, #10578, #16067 ) ;
#35304 = CARTESIAN_POINT ( 'NONE',  ( 9.656570333113133842, 18.37762487846717363, -27.33940497250931045 ) ) ;
#35305 = DIRECTION ( 'NONE',  ( 0.000000000000000000, 0.000000000000000000, -1.000000000000000000 ) ) ;
#35306 = ORIENTED_EDGE ( 'NONE', *, *, #11083, .F. ) ;
#35308 = LINE ( 'NONE', #29009, #10283 ) ;
#35307 = CARTESIAN_POINT ( 'NONE',  ( -18.55075427606121252, 13.25029436287058715, -16.96479077551187586 ) ) ;
#35309 = CARTESIAN_POINT ( 'NONE',  ( -18.23649648353780961, -16.09146789626143814, 23.00000000000000000 ) ) ;
#35310 = EDGE_CURVE ( 'NONE', #11163, #21446, #36466, .T. ) ;
#35311 = CARTESIAN_POINT ( 'NONE',  ( 9.569772169525011307, -18.12929409070867948, -29.34686813031393271 ) ) ;
#35312 = DIRECTION ( 'NONE',  ( 1.000000000000000000, 0.000000000000000000, 0.000000000000000000 ) ) ;
#35313 = CARTESIAN_POINT ( 'NONE',  ( 15.40208502184672135, 26.83309954512951023, -5.473965072825944134 ) ) ;
#35314 = CARTESIAN_POINT ( 'NONE',  ( -21.88499642459564853, -5.528038495964381127, -30.00000000000000355 ) ) ;
#35315 = CARTESIAN_POINT ( 'NONE',  ( -21.92386325230624067, -15.64910744109602625, 23.00000000000000355 ) ) ;
#35316 = AXIS2_PLACEMENT_3D ( 'NONE', #13346, #10923, #38134 ) ;
#35317 = CARTESIAN_POINT ( 'NONE',  ( -22.16102929819185974, -19.64143327435995801, -15.76658576923206034 ) ) ;
#35318 = CARTESIAN_POINT ( 'NONE',  ( 7.953009581834296071, -24.24005142096364551, -11.78114088531529191 ) ) ;
#35319 = CARTESIAN_POINT ( 'NONE',  ( 11.61490188824428493, 18.32440375615002282, -23.87370887680063447 ) ) ;
#35320 = CARTESIAN_POINT ( 'NONE',  ( 16.68830378044837914, 11.92867436094057787, -29.99999999999999645 ) ) ;
#35321 = DIRECTION ( 'NONE',  ( 1.000000000000000000, 0.000000000000000000, 0.000000000000000000 ) ) ;
#35322 = CARTESIAN_POINT ( 'NONE',  ( -6.354454053420243831, 35.54304081427989814, 7.000000000000000000 ) ) ;
#35323 = VERTEX_POINT ( 'NONE', #14732 ) ;
#35324 = CARTESIAN_POINT ( 'NONE',  ( -8.157141749000260234, 34.61756633539883410, -9.342187312551713418 ) ) ;
#35325 = ORIENTED_EDGE ( 'NONE', *, *, #33101, .F. ) ;
#35326 = B_SPLINE_CURVE_WITH_KNOTS ( 'NONE', 3,
 ( #15140, #6189, #39912, #5985 ),
 .UNSPECIFIED., .F., .F.,
 ( 4, 4 ),
 ( 8.673617379884035472E-19, 0.0006014480309583149914 ),
 .UNSPECIFIED. ) ;
#35327 = CARTESIAN_POINT ( 'NONE',  ( -9.469853072659795146, -18.32362292512856428, -28.08296521917836941 ) ) ;
#35328 = CARTESIAN_POINT ( 'NONE',  ( -13.97557076678966403, 21.53386246193713305, 9.500000000000000000 ) ) ;
#35329 = EDGE_LOOP ( 'NONE', ( #27504, #30391, #35089 ) ) ;
#35330 = CARTESIAN_POINT ( 'NONE',  ( 30.81126407598692651, -0.05061877264937817561, -6.416964798920022695 ) ) ;
#35331 = DIRECTION ( 'NONE',  ( -1.000000000000000000, 0.000000000000000000, 0.000000000000000000 ) ) ;
#35332 = EDGE_CURVE ( 'NONE', #10420, #20455, #1746, .T. ) ;
#35333 = DIRECTION ( 'NONE',  ( 0.9510565162951543083, 0.3090169943749450088, 0.000000000000000000 ) ) ;
#35334 = PRODUCT_DEFINITION_SHAPE ( 'NONE', 'NONE',  #40205 ) ;
#35335 = ORIENTED_EDGE ( 'NONE', *, *, #29948, .T. ) ;
#35336 = CARTESIAN_POINT ( 'NONE',  ( -22.20966955782450469, 0.7103411302137916383, -22.74070771460645091 ) ) ;
#35337 = ORIENTED_EDGE ( 'NONE', *, *, #23296, .T. ) ;
#35338 = CARTESIAN_POINT ( 'NONE',  ( 19.94806447466153543, -4.723319992639698484, -29.25382421619654849 ) ) ;
#35339 = CIRCLE ( 'NONE', #30795, 6.000000000000005329 ) ;
#35340 = EDGE_CURVE ( 'NONE', #13129, #6246, #36069, .T. ) ;
#35341 = VERTEX_POINT ( 'NONE', #4986 ) ;
#35342 = SHAPE_REPRESENTATION_RELATIONSHIP ( 'NONE' , 'NONE' ,  #33787, #3225 ) ;
#35343 = CARTESIAN_POINT ( 'NONE',  ( 9.340438144417252175, 38.00965938232027952, 11.55979286843940024 ) ) ;
#35344 = EDGE_CURVE ( 'NONE', #25235, #21075, #20233, .T. ) ;
#35345 = DIRECTION ( 'NONE',  ( 0.9135454576426059736, 0.4067366430757889395, -0.000000000000000000 ) ) ;
#35346 = VECTOR ( 'NONE', #23998, 1000.000000000000000 ) ;
#35347 = CARTESIAN_POINT ( 'NONE',  ( 6.953805871968278929, 30.22298757065274444, 12.00000000000000000 ) ) ;
#35348 = CARTESIAN_POINT ( 'NONE',  ( -12.19686730905342209, 28.97781536196876928, 18.42518152272111109 ) ) ;
#35349 = VECTOR ( 'NONE', #28939, 1000.000000000000000 ) ;
#35350 = FACE_OUTER_BOUND ( 'NONE', #20850, .T. ) ;
#35351 = ORIENTED_EDGE ( 'NONE', *, *, #25892, .F. ) ;
#35352 =( LENGTH_UNIT ( ) NAMED_UNIT ( * ) SI_UNIT ( .MILLI., .METRE. ) );
#35353 = CARTESIAN_POINT ( 'NONE',  ( 11.39463915635820612, 18.33192650902018883, 12.00000000000000000 ) ) ;
#35354 = CARTESIAN_POINT ( 'NONE',  ( -8.472151273871419974, 28.78272654129072095, 10.49999999999999822 ) ) ;
#35355 = FACE_OUTER_BOUND ( 'NONE', #18229, .T. ) ;
#35356 = CARTESIAN_POINT ( 'NONE',  ( 15.87504137958280559, 15.79823347536147082, -19.97344786039081654 ) ) ;
#35357 = CARTESIAN_POINT ( 'NONE',  ( 7.777352336794518983, 26.89720915371588816, -16.82449721399039078 ) ) ;
#35358 = ORIENTED_EDGE ( 'NONE', *, *, #30515, .F. ) ;
#35359 = CARTESIAN_POINT ( 'NONE',  ( 6.953805871968278929, 30.22298757065274444, 6.000000000000000000 ) ) ;
#35360 = CARTESIAN_POINT ( 'NONE',  ( -2.036571916123810055, 8.108948098542073879, 10.50000000000000355 ) ) ;
#35361 = EDGE_CURVE ( 'NONE', #36944, #19274, #17397, .T. ) ;
#35362 = EDGE_CURVE ( 'NONE', #17187, #24136, #34099, .T. ) ;
#35363 = CARTESIAN_POINT ( 'NONE',  ( 13.26834981302413752, -22.56586285155463756, -16.37744211164412533 ) ) ;
#35364 = DIRECTION ( 'NONE',  ( 1.000000000000000000, 0.000000000000000000, 0.000000000000000000 ) ) ;
#35365 = DIRECTION ( 'NONE',  ( 1.000000000000000000, 0.000000000000000000, 0.000000000000000000 ) ) ;
#35366 = VERTEX_POINT ( 'NONE', #23872 ) ;
#35367 = CARTESIAN_POINT ( 'NONE',  ( -13.49987786938234535, 22.79920604360487602, -15.45166244955937707 ) ) ;
#35368 = CARTESIAN_POINT ( 'NONE',  ( -31.24272016125062024, 0.2902395683499273682, 15.72805884748940031 ) ) ;
#35369 = CARTESIAN_POINT ( 'NONE',  ( 14.66427835382668299, -26.25532329094042439, -7.831039160053395953 ) ) ;
#35370 = CARTESIAN_POINT ( 'NONE',  ( -9.356056665764020508, 26.06569820189716324, 10.50000000000000533 ) ) ;
#35371 = ORIENTED_EDGE ( 'NONE', *, *, #712, .F. ) ;
#35372 = ORIENTED_EDGE ( 'NONE', *, *, #27047, .F. ) ;
#35373 = CARTESIAN_POINT ( 'NONE',  ( -11.48887937525355341, 24.79999023685312309, -16.14676052428935904 ) ) ;
#35374 = CIRCLE ( 'NONE', #24352, 1.000000000000000000 ) ;
#35375 = CARTESIAN_POINT ( 'NONE',  ( -16.57032934033265192, -22.18377020236782826, -16.08031648850850104 ) ) ;
#35376 = DIRECTION ( 'NONE',  ( 1.000000000000000000, 0.000000000000000000, 0.000000000000000000 ) ) ;
#35377 = AXIS2_PLACEMENT_3D ( 'NONE', #1781, #32865, #14162 ) ;
#35379 = CIRCLE ( 'NONE', #22455, 1.000000000000000888 ) ;
#35378 = CARTESIAN_POINT ( 'NONE',  ( -35.20073123246135083, -8.756190693406901815, -6.311296342382265223 ) ) ;
#35380 = LINE ( 'NONE', #20346, #33217 ) ;
#35381 = VERTEX_POINT ( 'NONE', #21028 ) ;
#35382 = CARTESIAN_POINT ( 'NONE',  ( 22.68044555609654367, 0.7780309201116830664, -21.63808993525804780 ) ) ;
#35383 = DIRECTION ( 'NONE',  ( 0.000000000000000000, 0.000000000000000000, 1.000000000000000000 ) ) ;
#35384 = DIRECTION ( 'NONE',  ( 0.5000000000000039968, 0.8660254037844363761, 0.000000000000000000 ) ) ;
#35385 = ORIENTED_EDGE ( 'NONE', *, *, #35436, .F. ) ;
#35386 = CARTESIAN_POINT ( 'NONE',  ( -22.22324547119116289, 0.6552216296766762982, -22.73395167228940750 ) ) ;
#35387 = EDGE_CURVE ( 'NONE', #20746, #6207, #35868, .T. ) ;
#35388 = FACE_OUTER_BOUND ( 'NONE', #20370, .T. ) ;
#35389 = ORIENTED_EDGE ( 'NONE', *, *, #8508, .T. ) ;
#35390 = CARTESIAN_POINT ( 'NONE',  ( 20.47947323059178260, -0.9304062671392134831, -29.31544170430820628 ) ) ;
#35391 = CARTESIAN_POINT ( 'NONE',  ( -9.038010526469660633, 11.76154733104328010, 10.50000000000000000 ) ) ;
#35392 = CARTESIAN_POINT ( 'NONE',  ( 35.93605200993547300, -16.45551934609908429, 14.53008259254004386 ) ) ;
#35393 = ORIENTED_EDGE ( 'NONE', *, *, #3462, .T. ) ;
#35394 = CARTESIAN_POINT ( 'NONE',  ( 12.92636675529317891, 33.47246997465054363, 15.13084544680219423 ) ) ;
#35395 = CARTESIAN_POINT ( 'NONE',  ( 5.594491472542083343, -20.30912387778604966, 19.66345542862528717 ) ) ;
#35396 = DIRECTION ( 'NONE',  ( 0.5254827454987550661, -0.4731467892558230415, -0.7071067811865451302 ) ) ;
#35397 = CARTESIAN_POINT ( 'NONE',  ( -1.431596709943599777, 28.99142433710769495, 20.94377226548377990 ) ) ;
#35398 = CARTESIAN_POINT ( 'NONE',  ( 13.53057405073934838, 22.08338764125490528, 10.50000000000000000 ) ) ;
#35399 = CARTESIAN_POINT ( 'NONE',  ( 9.331903152615748098, 11.35703883385568780, 10.49999999999999645 ) ) ;
#35400 = AXIS2_PLACEMENT_3D ( 'NONE', #3680, #31911, #4284 ) ;
#35401 = AXIS2_PLACEMENT_3D ( 'NONE', #2530, #39695, #21015 ) ;
#35402 = CIRCLE ( 'NONE', #13972, 1.000000000000000000 ) ;
#35403 = CYLINDRICAL_SURFACE ( 'NONE', #29464, 1.000000000000000000 ) ;
#35404 = CARTESIAN_POINT ( 'NONE',  ( 24.45776404695103778, 8.140618660892668501, 15.72805884748940386 ) ) ;
#35405 = CARTESIAN_POINT ( 'NONE',  ( -22.90242673301339593, 8.786414512089246287, -10.86241974061178972 ) ) ;
#35406 = EDGE_CURVE ( 'NONE', #7, #14009, #32152, .T. ) ;
#35407 = CARTESIAN_POINT ( 'NONE',  ( 20.28942584164974505, -25.11661602538714888, -11.27543687046667387 ) ) ;
#35408 = CARTESIAN_POINT ( 'NONE',  ( -5.082607396026893376, 23.58034083595207875, 6.000000000000000000 ) ) ;
#35409 = EDGE_LOOP ( 'NONE', ( #30564, #8103, #8957 ) ) ;
#35410 = CARTESIAN_POINT ( 'NONE',  ( 14.96161369655125206, 26.15114394812015064, -9.229261913996447575 ) ) ;
#35411 = EDGE_LOOP ( 'NONE', ( #30923, #28182, #118 ) ) ;
#35412 = CARTESIAN_POINT ( 'NONE',  ( -15.03288268948483264, 23.64078904719026042, -11.63896337504832879 ) ) ;
#35413 = CARTESIAN_POINT ( 'NONE',  ( -23.63966112704447298, -21.14828014214127805, 19.99202127657103389 ) ) ;
#35414 = CARTESIAN_POINT ( 'NONE',  ( -13.94482798346716379, 26.50521816028930999, 10.99999999999999289 ) ) ;
#35415 = CARTESIAN_POINT ( 'NONE',  ( 14.56710521870112807, 24.87586913598118343, -11.60179260043244653 ) ) ;
#35416 = EDGE_LOOP ( 'NONE', ( #28666, #34622 ) ) ;
#35417 = CARTESIAN_POINT ( 'NONE',  ( 24.85582250148247496, -12.74015949003176651, -17.59997480698870476 ) ) ;
#35418 = DIRECTION ( 'NONE',  ( 0.000000000000000000, 0.000000000000000000, 1.000000000000000000 ) ) ;
#35419 = VERTEX_POINT ( 'NONE', #29770 ) ;
#35421 = FACE_OUTER_BOUND ( 'NONE', #11834, .T. ) ;
#35420 = CARTESIAN_POINT ( 'NONE',  ( -10.74659509297316440, 17.51247683012617884, -28.69615268264896102 ) ) ;
#35422 = CARTESIAN_POINT ( 'NONE',  ( -16.49457207817568261, -26.65912990296860130, -7.789058334551107521 ) ) ;
#35423 = DIRECTION ( 'NONE',  ( 0.000000000000000000, 0.000000000000000000, 1.000000000000000000 ) ) ;
#35424 = VERTEX_POINT ( 'NONE', #16985 ) ;
#35425 = CARTESIAN_POINT ( 'NONE',  ( -24.63622891667736781, -10.18470011515834095, -18.66157544239288057 ) ) ;
#35426 = CARTESIAN_POINT ( 'NONE',  ( -9.357072968089592990, -18.59482942431551677, -26.85790916864404565 ) ) ;
#35427 = DIRECTION ( 'NONE',  ( -0.000000000000000000, -0.000000000000000000, -1.000000000000000000 ) ) ;
#35428 = CARTESIAN_POINT ( 'NONE',  ( 14.67864225457747906, 16.82336705159722001, -20.92344909559215793 ) ) ;
#35429 = EDGE_LOOP ( 'NONE', ( #9480, #27636, #11700, #35936 ) ) ;
#35430 = CARTESIAN_POINT ( 'NONE',  ( 25.64058186160713859, 3.762799545439524440, -12.71090497642184580 ) ) ;
#35431 = LINE ( 'NONE', #10040, #14148 ) ;
#35432 = DIRECTION ( 'NONE',  ( 1.000000000000000000, 0.000000000000000000, 0.000000000000000000 ) ) ;
#35433 = CIRCLE ( 'NONE', #402, 0.5000000000000000000 ) ;
#35434 = EDGE_LOOP ( 'NONE', ( #25812, #23191 ) ) ;
#35435 = CARTESIAN_POINT ( 'NONE',  ( -20.99434144220187548, 0.5542567078580580286, -26.20245057682946310 ) ) ;
#35436 = EDGE_CURVE ( 'NONE', #24757, #18996, #33036, .T. ) ;
#35437 = CARTESIAN_POINT ( 'NONE',  ( 30.84859707095975878, -0.5449750927740264483, -8.270921991002078144 ) ) ;
#35438 = CIRCLE ( 'NONE', #17926, 1.000000000000004441 ) ;
#35439 = EDGE_CURVE ( 'NONE', #17409, #40053, #35374, .T. ) ;
#35440 = CARTESIAN_POINT ( 'NONE',  ( 30.78606151651052159, -16.23943018785194781, 19.27171037444156454 ) ) ;
#35441 = AXIS2_PLACEMENT_3D ( 'NONE', #28607, #583, #7262 ) ;
#35442 = VERTEX_POINT ( 'NONE', #8438 ) ;
#35443 = ADVANCED_FACE ( 'NONE', ( #4784 ), #33236, .F. ) ;
#35444 = CARTESIAN_POINT ( 'NONE',  ( -28.84245173844059806, 0.9132675324983203780, -10.20106989243743278 ) ) ;
#35445 = CARTESIAN_POINT ( 'NONE',  ( -6.023418944065151770, 39.81932404830322270, -14.45070082761206365 ) ) ;
#35446 = PLANE ( 'NONE',  #33599 ) ;
#35447 = ADVANCED_FACE ( 'NONE', ( #29363 ), #1540, .F. ) ;
#35448 = DIRECTION ( 'NONE',  ( -0.7032331762534009822, 0.07391278520356894810, 0.7071067811865506814 ) ) ;
#35449 = CARTESIAN_POINT ( 'NONE',  ( -2.518583951651248931, 7.712953814960721743, 7.499999999999997335 ) ) ;
#35450 = LINE ( 'NONE', #4768, #21663 ) ;
#35451 = CARTESIAN_POINT ( 'NONE',  ( -0.8712085880691411433, 13.69667159339610762, 13.00000000000000178 ) ) ;
#35452 = EDGE_LOOP ( 'NONE', ( #22727, #11154, #2566, #1008 ) ) ;
#35453 = DIRECTION ( 'NONE',  ( -0.9135454576426005335, 0.4067366430758009299, -0.000000000000000000 ) ) ;
#35454 = CYLINDRICAL_SURFACE ( 'NONE', #25901, 0.4999999999999996669 ) ;
#35455 = CARTESIAN_POINT ( 'NONE',  ( 15.94967524335434739, -13.83360700755901185, -26.33159008689450431 ) ) ;
#35456 = EDGE_CURVE ( 'NONE', #614, #30787, #10081, .T. ) ;
#35457 = EDGE_CURVE ( 'NONE', #38453, #7138, #33456, .T. ) ;
#35458 = DIRECTION ( 'NONE',  ( 0.4156269377774612361, 0.5720614028176856936, -0.7071067811865417996 ) ) ;
#35459 = LINE ( 'NONE', #32417, #5406 ) ;
#35460 = EDGE_CURVE ( 'NONE', #15406, #30242, #18577, .T. ) ;
#35461 = CARTESIAN_POINT ( 'NONE',  ( 10.41696638283783471, 17.65700839937217381, -29.33613504912931091 ) ) ;
#35462 = LINE ( 'NONE', #16978, #8754 ) ;
#35463 = EDGE_LOOP ( 'NONE', ( #5108, #14809, #36231 ) ) ;
#35464 = CARTESIAN_POINT ( 'NONE',  ( -17.64770094672744349, 19.45792562635240230, -8.363180893698942242 ) ) ;
#35465 = CARTESIAN_POINT ( 'NONE',  ( -24.22138565352714323, -9.557272464391497024, 20.99999999999999645 ) ) ;
#35466 = AXIS2_PLACEMENT_3D ( 'NONE', #32212, #7823, #4984 ) ;
#35467 = CARTESIAN_POINT ( 'NONE',  ( 13.32179451523274238, -23.61806545529600143, -14.47902645169415337 ) ) ;
#35468 = FACE_OUTER_BOUND ( 'NONE', #28508, .T. ) ;
#35469 = CARTESIAN_POINT ( 'NONE',  ( 11.69932325419884300, 18.89880935514919713, -22.73734831153147695 ) ) ;
#35470 = EDGE_LOOP ( 'NONE', ( #11107, #24389, #20174, #13175 ) ) ;
#35471 = CARTESIAN_POINT ( 'NONE',  ( 15.36544744475249580, 26.69572735888668902, -6.416978652968691854 ) ) ;
#35472 = ORIENTED_EDGE ( 'NONE', *, *, #3052, .F. ) ;
#35474 = DIRECTION ( 'NONE',  ( 0.000000000000000000, 0.7071067811865500152, -0.7071067811865451302 ) ) ;
#35473 = CARTESIAN_POINT ( 'NONE',  ( -14.81640337485448100, 25.68318687829989599, -10.17575449534364829 ) ) ;
#35475 = CARTESIAN_POINT ( 'NONE',  ( -13.67385565238511269, -24.11288955641917298, -13.51489229801976322 ) ) ;
#35476 = CARTESIAN_POINT ( 'NONE',  ( -35.02038065029437774, -20.21902619557053526, 12.14047268033097282 ) ) ;
#35477 = CARTESIAN_POINT ( 'NONE',  ( -28.90832190807780222, -18.69259600629643714, -11.97739893689305646 ) ) ;
#35478 = CARTESIAN_POINT ( 'NONE',  ( -5.491606936905080616, -21.66488701077363643, -19.98327345564413449 ) ) ;
#35479 = CARTESIAN_POINT ( 'NONE',  ( 14.03912507337044779, 21.76248058076597403, -15.52699132478714894 ) ) ;
#35480 = ORIENTED_EDGE ( 'NONE', *, *, #4069, .F. ) ;
#35481 = CARTESIAN_POINT ( 'NONE',  ( 23.83304178564468501, 8.268703381674290753, -7.903184250208921569 ) ) ;
#35482 = LINE ( 'NONE', #7029, #32273 ) ;
#35483 = CARTESIAN_POINT ( 'NONE',  ( 15.48853125999101898, -26.74269726803731828, -5.000000000000000000 ) ) ;
#35484 = CARTESIAN_POINT ( 'NONE',  ( 1.734965421685031872, 7.600674680189132282, 7.000000000000000000 ) ) ;
#35485 = VERTEX_POINT ( 'NONE', #9035 ) ;
#35486 = CARTESIAN_POINT ( 'NONE',  ( -32.11025114950868442, -1.657766350062749527, -6.846984724189184135 ) ) ;
#35487 = ADVANCED_FACE ( 'NONE', ( #37060 ), #39707, .F. ) ;
#35488 = CARTESIAN_POINT ( 'NONE',  ( -11.08993573050815939, 19.63476728485979095, 20.25080042701544514 ) ) ;
#35489 = ORIENTED_EDGE ( 'NONE', *, *, #19664, .F. ) ;
#35490 = EDGE_CURVE ( 'NONE', #2539, #7713, #6817, .T. ) ;
#35491 = CARTESIAN_POINT ( 'NONE',  ( 14.47283171447379502, 21.48159823030311344, 7.000000000000000000 ) ) ;
#35492 = CARTESIAN_POINT ( 'NONE',  ( 75.15099915297797395, 43.38844959084117647, 3.000000000000000000 ) ) ;
#35493 = DIRECTION ( 'NONE',  ( 0.04273212933193662466, -0.8153776007405469928, 0.5773502691896383876 ) ) ;
#35494 = CARTESIAN_POINT ( 'NONE',  ( 28.51905879638759700, -12.47949435409169539, -14.75475664525949071 ) ) ;
#35495 = CARTESIAN_POINT ( 'NONE',  ( 33.93864557196972243, -21.81860479675949804, 12.73282698324848461 ) ) ;
#35496 = CIRCLE ( 'NONE', #5644, 1.000000000000000000 ) ;
#35497 = VERTEX_POINT ( 'NONE', #5577 ) ;
#35498 = CARTESIAN_POINT ( 'NONE',  ( -32.33143948541789570, 1.358872982501806215, 0.000000000000000000 ) ) ;
#35499 = CARTESIAN_POINT ( 'NONE',  ( 10.18324034840045478, 28.21559575157615996, 12.00000000000000000 ) ) ;
#35500 = VECTOR ( 'NONE', #27952, 1000.000000000000000 ) ;
#35501 = DIRECTION ( 'NONE',  ( 1.000000000000000000, 0.000000000000000000, 0.000000000000000000 ) ) ;
#35502 = EDGE_LOOP ( 'NONE', ( #3528, #35794 ) ) ;
#35503 = CARTESIAN_POINT ( 'NONE',  ( -0.5479328185110891036, 27.95115490892091259, -17.59429925479824064 ) ) ;
#35504 = CARTESIAN_POINT ( 'NONE',  ( 0.000000000000000000, 0.000000000000000000, -30.00000000000000000 ) ) ;
#35505 = DIRECTION ( 'NONE',  ( -1.000000000000000000, 0.000000000000000000, 0.000000000000000000 ) ) ;
#35506 = CARTESIAN_POINT ( 'NONE',  ( 33.75875814100317029, 2.759858869446390361, 11.00000000000000000 ) ) ;
#35507 = DIRECTION ( 'NONE',  ( 0.5000000000000039968, 0.8660254037844363761, 0.000000000000000000 ) ) ;
#35508 = CARTESIAN_POINT ( 'NONE',  ( -20.57924982997939622, -27.21273881503329051, -4.999999999999998224 ) ) ;
#35509 = CARTESIAN_POINT ( 'NONE',  ( 14.05079942517586389, 29.36071225880166580, -7.738770433462001108 ) ) ;
#35510 = CYLINDRICAL_SURFACE ( 'NONE', #12713, 1.000000000000000888 ) ;
#35511 = EDGE_LOOP ( 'NONE', ( #36753, #30258, #34677, #21572 ) ) ;
#35513 = DIRECTION ( 'NONE',  ( 1.000000000000000000, 0.000000000000000000, 0.000000000000000000 ) ) ;
#35512 = CARTESIAN_POINT ( 'NONE',  ( -17.27691955920570877, 11.15657196891051228, -28.29868769472810541 ) ) ;
#35514 = CARTESIAN_POINT ( 'NONE',  ( -0.6830608540011002816, 37.47223625998410057, 10.49999999999999822 ) ) ;
#35515 = CARTESIAN_POINT ( 'NONE',  ( 15.41906236961596655, -26.60135734087577219, -6.887199331419184389 ) ) ;
#35516 = DIRECTION ( 'NONE',  ( 1.000000000000000000, 0.000000000000000000, 0.000000000000000000 ) ) ;
#35517 = CARTESIAN_POINT ( 'NONE',  ( 11.03763599804776341, 17.52625919505898011, -27.44504327041069303 ) ) ;
#35518 = CARTESIAN_POINT ( 'NONE',  ( -33.62187204924172335, 0.04418559750806001774, -13.79123840944734347 ) ) ;
#35519 = CARTESIAN_POINT ( 'NONE',  ( -1.158196024796639412, -0.5060543600718802049, 10.00000000000000000 ) ) ;
#35520 = VECTOR ( 'NONE', #28879, 1000.000000000000227 ) ;
#35521 = CIRCLE ( 'NONE', #16055, 0.4999999999999999445 ) ;
#35522 = CARTESIAN_POINT ( 'NONE',  ( -26.61324971144608043, -23.59943729456863082, -9.772242488793104087 ) ) ;
#35523 = CARTESIAN_POINT ( 'NONE',  ( 7.642913368978748956, -23.62237106133328624, -13.77340500620915620 ) ) ;
#35524 = CARTESIAN_POINT ( 'NONE',  ( 13.35043658488273266, 21.98571059302396336, -16.46575276999205073 ) ) ;
#35525 = CARTESIAN_POINT ( 'NONE',  ( 20.47654757076874787, 13.90376119549317124, -7.426114723384639404 ) ) ;
#35526 = CARTESIAN_POINT ( 'NONE',  ( -2.672146553953452575, 12.33340603770394139, 10.50000000000000000 ) ) ;
#35527 = ORIENTED_EDGE ( 'NONE', *, *, #26789, .T. ) ;
#35528 = CARTESIAN_POINT ( 'NONE',  ( -7.286326729150405690, 35.71687252700443338, -8.445018646286913011 ) ) ;
#35529 = AXIS2_PLACEMENT_3D ( 'NONE', #711, #38486, #35041 ) ;
#35530 = VERTEX_POINT ( 'NONE', #30964 ) ;
#35531 = CARTESIAN_POINT ( 'NONE',  ( -12.52581896409591877, -22.55617444508696678, -16.45362975895816504 ) ) ;
#35532 = AXIS2_PLACEMENT_3D ( 'NONE', #29986, #30192, #8043 ) ;
#35533 = CARTESIAN_POINT ( 'NONE',  ( 5.464578388833499112, 36.46941714767122278, 7.485646746502379933 ) ) ;
#35534 = ORIENTED_EDGE ( 'NONE', *, *, #20636, .F. ) ;
#35535 = DIRECTION ( 'NONE',  ( 0.5000000000000038858, 0.8660254037844364872, -0.000000000000000000 ) ) ;
#35536 = LINE ( 'NONE', #29433, #5726 ) ;
#35537 = ORIENTED_EDGE ( 'NONE', *, *, #18881, .F. ) ;
#35538 = CARTESIAN_POINT ( 'NONE',  ( -30.74131631141073129, 0.1242922002067064352, -5.474147495693744148 ) ) ;
#35539 = EDGE_LOOP ( 'NONE', ( #19890, #15489, #35371, #19106 ) ) ;
#35540 = CARTESIAN_POINT ( 'NONE',  ( 22.59748200846286181, -6.094062071576993311, -22.04567670539332624 ) ) ;
#35541 = EDGE_LOOP ( 'NONE', ( #11825, #33908, #5013 ) ) ;
#35542 = CARTESIAN_POINT ( 'NONE',  ( 0.000000000000000000, 0.000000000000000000, 0.000000000000000000 ) ) ;
#35543 = CARTESIAN_POINT ( 'NONE',  ( -14.89626057892323630, 32.60452476689623325, 11.55979286843934872 ) ) ;
#35544 = AXIS2_PLACEMENT_3D ( 'NONE', #830, #22555, #18525 ) ;
#35545 = FACE_OUTER_BOUND ( 'NONE', #3896, .T. ) ;
#35546 = DIRECTION ( 'NONE',  ( 1.000000000000000000, 0.000000000000000000, 0.000000000000000000 ) ) ;
#35547 = CARTESIAN_POINT ( 'NONE',  ( 9.490716042091355220, 32.53254263376074817, 18.42518152272108622 ) ) ;
#35548 = VECTOR ( 'NONE', #16495, 1000.000000000000000 ) ;
#35549 = CIRCLE ( 'NONE', #36195, 1.000000000000000000 ) ;
#35550 = CYLINDRICAL_SURFACE ( 'NONE', #3849, 6.000000000000005329 ) ;
#35551 = ORIENTED_EDGE ( 'NONE', *, *, #2717, .F. ) ;
#35552 = CARTESIAN_POINT ( 'NONE',  ( 12.53024597560964359, 27.62278594035691626, 10.50000000000000000 ) ) ;
#35553 = FACE_OUTER_BOUND ( 'NONE', #20199, .T. ) ;
#35554 = CARTESIAN_POINT ( 'NONE',  ( 6.811226782241714517, 35.33967249274190436, 11.00000000000000000 ) ) ;
#35555 = CARTESIAN_POINT ( 'NONE',  ( 18.53648777117533442, 17.88871277907829338, -6.924686450352337985 ) ) ;
#35556 = AXIS2_PLACEMENT_3D ( 'NONE', #2258, #36385, #39224 ) ;
#35557 = CARTESIAN_POINT ( 'NONE',  ( 9.323248225502032582, 32.23778593834843065, -11.17991894423324339 ) ) ;
#35558 = ORIENTED_EDGE ( 'NONE', *, *, #10056, .F. ) ;
#35559 = DIRECTION ( 'NONE',  ( 0.8090169943749426773, -0.5877852522924796874, 0.000000000000000000 ) ) ;
#35560 = LINE ( 'NONE', #32924, #27250 ) ;
#35561 = EDGE_CURVE ( 'NONE', #29026, #10996, #17228, .T. ) ;
#35562 = CARTESIAN_POINT ( 'NONE',  ( 14.04058618686241466, -23.68300519570117402, -14.41379008992138822 ) ) ;
#35563 = CARTESIAN_POINT ( 'NONE',  ( 13.63581098909226874, 27.45627467658428955, 7.000000000000000000 ) ) ;
#35564 = CARTESIAN_POINT ( 'NONE',  ( -14.49848586288629271, 20.47339359108951129, 11.00000000000000000 ) ) ;
#35565 = VERTEX_POINT ( 'NONE', #12076 ) ;
#35566 = CARTESIAN_POINT ( 'NONE',  ( -15.10048454435680831, 26.14110364457479818, -8.767509008662626613 ) ) ;
#35567 = CARTESIAN_POINT ( 'NONE',  ( -34.83511892542295385, -16.10726664691095067, 16.30093088680195024 ) ) ;
#35568 = CARTESIAN_POINT ( 'NONE',  ( 14.81091239784893077, -26.28932095263721536, -7.830188071801472915 ) ) ;
#35569 = EDGE_CURVE ( 'NONE', #10001, #8098, #6176, .T. ) ;
#35570 = CARTESIAN_POINT ( 'NONE',  ( -14.57486473880221745, 26.18419839932921533, 11.00000000000000000 ) ) ;
#35571 = EDGE_CURVE ( 'NONE', #9605, #12345, #14931, .T. ) ;
#35572 = ORIENTED_EDGE ( 'NONE', *, *, #21195, .T. ) ;
#35573 = ORIENTED_EDGE ( 'NONE', *, *, #8812, .T. ) ;
#35574 = CARTESIAN_POINT ( 'NONE',  ( -10.30011504994442717, 23.87368139273885248, -18.05724923619832012 ) ) ;
#35575 = CYLINDRICAL_SURFACE ( 'NONE', #17868, 1.000000000000000888 ) ;
#35576 = CARTESIAN_POINT ( 'NONE',  ( -12.74038105676665467, 14.56698729810789850, 10.49999999999999822 ) ) ;
#35577 = B_SPLINE_CURVE_WITH_KNOTS ( 'NONE', 3,
 ( #32908, #26797, #5060, #17472, #29843, #5262 ),
 .UNSPECIFIED., .F., .F.,
 ( 4, 2, 4 ),
 ( 0.000000000000000000, 0.5000000000000000000, 1.000000000000000000 ),
 .UNSPECIFIED. ) ;
#35578 = AXIS2_PLACEMENT_3D ( 'NONE', #1767, #5211, #26342 ) ;
#35579 = AXIS2_PLACEMENT_3D ( 'NONE', #10444, #13686, #16750 ) ;
#35580 = CARTESIAN_POINT ( 'NONE',  ( -32.61466699540454073, -8.035061020377614938, -11.17799411198647164 ) ) ;
#35581 = CARTESIAN_POINT ( 'NONE',  ( -11.66932856646905314, 37.85852258240264234, 10.00000000000000000 ) ) ;
#35582 = ORIENTED_EDGE ( 'NONE', *, *, #27318, .F. ) ;
#35583 = CARTESIAN_POINT ( 'NONE',  ( 30.47622998064611721, 0.1276006758484945214, -7.358534401045794482 ) ) ;
#35584 = CARTESIAN_POINT ( 'NONE',  ( -10.69300419909361466, 32.80084059136108721, 10.87262190629279424 ) ) ;
#35585 = CARTESIAN_POINT ( 'NONE',  ( 6.651296319737278750, 27.81603774131160023, 7.000000000000000000 ) ) ;
#35586 = CARTESIAN_POINT ( 'NONE',  ( -7.312041872459064784, 25.58773265502866678, 12.00000000000000000 ) ) ;
#35587 = UNCERTAINTY_MEASURE_WITH_UNIT (LENGTH_MEASURE( 1.000000000000000082E-05 ), #35664, 'distance_accuracy_value', 'NONE');
#35588 = CIRCLE ( 'NONE', #6361, 1.000000000000000888 ) ;
#35589 = VERTEX_POINT ( 'NONE', #24666 ) ;
#35590 = CARTESIAN_POINT ( 'NONE',  ( -22.73404044138284164, 0.5996816946850819230, -21.61592112696820678 ) ) ;
#35591 = ORIENTED_EDGE ( 'NONE', *, *, #22054, .T. ) ;
#35592 = CARTESIAN_POINT ( 'NONE',  ( 30.45180831424324808, -2.034437368685610981, -11.43179728121123162 ) ) ;
#35593 = CARTESIAN_POINT ( 'NONE',  ( 20.50220473200229065, -0.6271520275686577328, -30.00000000000000711 ) ) ;
#35594 = CARTESIAN_POINT ( 'NONE',  ( 16.99774364072579758, -28.32416636927767328, 14.53008259253903489 ) ) ;
#35595 = EDGE_CURVE ( 'NONE', #23174, #18033, #24272, .T. ) ;
#35596 = EDGE_LOOP ( 'NONE', ( #33689, #16248 ) ) ;
#35597 = CARTESIAN_POINT ( 'NONE',  ( -8.548670570953216696, 36.69528512485481997, 15.72805884748861693 ) ) ;
#35598 = EDGE_CURVE ( 'NONE', #7720, #7701, #18381, .T. ) ;
#35599 = CARTESIAN_POINT ( 'NONE',  ( 5.468510220371463504, -21.80712738496724157, 18.87996532025784902 ) ) ;
#35600 = CARTESIAN_POINT ( 'NONE',  ( 6.385371355716897845, 45.28367711306903942, 10.00000000000000000 ) ) ;
#35601 = CARTESIAN_POINT ( 'NONE',  ( 6.154269285972487680, 26.67460248448178461, 20.82122704794080192 ) ) ;
#35602 = CARTESIAN_POINT ( 'NONE',  ( -12.37435565298220119, 15.93301270189233598, 9.500000000000000000 ) ) ;
#35603 = EDGE_LOOP ( 'NONE', ( #34989, #34085, #30687, #14718 ) ) ;
#35604 = CYLINDRICAL_SURFACE ( 'NONE', #4617, 0.5000000000000004441 ) ;
#35605 = AXIS2_PLACEMENT_3D ( 'NONE', #13979, #23330, #35726 ) ;
#35606 = CARTESIAN_POINT ( 'NONE',  ( 6.092423932518094887, 37.33975570695338320, -5.438183848281402888 ) ) ;
#35607 = LINE ( 'NONE', #20168, #36575 ) ;
#35608 = CARTESIAN_POINT ( 'NONE',  ( 17.61963632522081369, 22.05541241827695842, 15.13084544678993559 ) ) ;
#35609 = CARTESIAN_POINT ( 'NONE',  ( 20.81479864165018512, -27.12526061484643236, -6.349197363260469018 ) ) ;
#35610 = DIRECTION ( 'NONE',  ( -0.9135454576426048634, -0.4067366430757912710, 0.000000000000000000 ) ) ;
#35611 = AXIS2_PLACEMENT_3D ( 'NONE', #38443, #1069, #16918 ) ;
#35612 = DIRECTION ( 'NONE',  ( -0.000000000000000000, -0.000000000000000000, 1.000000000000000000 ) ) ;
#35613 = DIRECTION ( 'NONE',  ( 0.000000000000000000, 0.000000000000000000, 1.000000000000000000 ) ) ;
#35614 = EDGE_CURVE ( 'NONE', #11394, #34302, #32807, .T. ) ;
#35615 = ORIENTED_EDGE ( 'NONE', *, *, #22556, .F. ) ;
#35616 = CARTESIAN_POINT ( 'NONE',  ( 14.80287293261903159, 25.72487161761031516, -10.17325132652339903 ) ) ;
#35617 = EDGE_LOOP ( 'NONE', ( #35551, #20185, #2531, #37875 ) ) ;
#35618 = CARTESIAN_POINT ( 'NONE',  ( -11.56430756512898661, 17.30006398449676297, -26.87031197432354901 ) ) ;
#35619 = CARTESIAN_POINT ( 'NONE',  ( -29.98847540738097806, -8.745685015165189924, 19.99202127657046191 ) ) ;
#35620 = DIRECTION ( 'NONE',  ( -0.4999999999999933942, 0.8660254037844425934, 0.000000000000000000 ) ) ;
#35621 = CARTESIAN_POINT ( 'NONE',  ( 11.03950910960345766, 17.27365618835783678, -30.00000000000000000 ) ) ;
#35622 = ORIENTED_EDGE ( 'NONE', *, *, #16069, .T. ) ;
#35623 = CARTESIAN_POINT ( 'NONE',  ( 21.96604632341627195, -11.26784406932779348, -20.69622655604641537 ) ) ;
#35624 = EDGE_LOOP ( 'NONE', ( #31538, #24190, #3485, #2660, #20757 ) ) ;
#35626 = CARTESIAN_POINT ( 'NONE',  ( 13.05736835487433289, 16.11602540378438420, 7.000000000000000000 ) ) ;
#35625 = CARTESIAN_POINT ( 'NONE',  ( -15.23746052738172096, 27.38211562678985445, -5.471314660788269890 ) ) ;
#35627 = CARTESIAN_POINT ( 'NONE',  ( -15.51450792689023750, -25.25784468116843229, -11.51896233938664693 ) ) ;
#35628 = CARTESIAN_POINT ( 'NONE',  ( -0.5000000000000004441, 36.50000000000000711, 7.000000000000000000 ) ) ;
#35629 = VERTEX_POINT ( 'NONE', #21615 ) ;
#35630 = CARTESIAN_POINT ( 'NONE',  ( -34.21394365919860547, -14.11642697757303644, -8.422019832718921961 ) ) ;
#35631 = CARTESIAN_POINT ( 'NONE',  ( -14.49814074169044709, -25.88491989834313145, -9.244276984472083569 ) ) ;
#35632 = CARTESIAN_POINT ( 'NONE',  ( 18.77248997590692170, -31.35432035706033105, 22.99999999999999289 ) ) ;
#35633 = CARTESIAN_POINT ( 'NONE',  ( 17.24384880539558651, 21.04619446147080097, -6.430924243040796462 ) ) ;
#35634 = VERTEX_POINT ( 'NONE', #34020 ) ;
#35635 = CARTESIAN_POINT ( 'NONE',  ( 20.31991420201310206, 4.509322195999590832, -26.47951906542851930 ) ) ;
#35636 = DIRECTION ( 'NONE',  ( 0.000000000000000000, 0.000000000000000000, 1.000000000000000000 ) ) ;
#35637 = DIRECTION ( 'NONE',  ( 0.000000000000000000, 0.000000000000000000, 1.000000000000000000 ) ) ;
#35638 = EDGE_LOOP ( 'NONE', ( #24025, #23936, #10373, #5813 ) ) ;
#35639 = CARTESIAN_POINT ( 'NONE',  ( -27.27908345015220348, 0.04356745379364866666, -14.45463337275631233 ) ) ;
#35641 = CARTESIAN_POINT ( 'NONE',  ( 24.07089776856416563, 0.1762921601959324680, -19.45410240058878770 ) ) ;
#35640 = AXIS2_PLACEMENT_3D ( 'NONE', #20693, #36522, #23727 ) ;
#35642 = AXIS2_PLACEMENT_3D ( 'NONE', #2583, #2975, #2384 ) ;
#35643 = CARTESIAN_POINT ( 'NONE',  ( 19.04856739887212669, -23.59522229971750917, 19.27171037444155388 ) ) ;
#35644 = ADVANCED_FACE ( 'NONE', ( #88 ), #27319, .T. ) ;
#35645 = ORIENTED_EDGE ( 'NONE', *, *, #10776, .T. ) ;
#35646 = CARTESIAN_POINT ( 'NONE',  ( -20.88993331574549117, 1.492557873551023873, -26.28200927340007809 ) ) ;
#35647 = ADVANCED_FACE ( 'NONE', ( #24865 ), #37259, .T. ) ;
#35648 = CIRCLE ( 'NONE', #36947, 18.00000000000000000 ) ;
#35649 = CARTESIAN_POINT ( 'NONE',  ( -6.155076441694329326, 21.71698211341365692, -29.99999999999997868 ) ) ;
#35650 = DIRECTION ( 'NONE',  ( 0.000000000000000000, 0.000000000000000000, 1.000000000000000000 ) ) ;
#35651 = CARTESIAN_POINT ( 'NONE',  ( -6.348113209407908464, 9.835177808069893501, 12.00000000000000000 ) ) ;
#35652 = CARTESIAN_POINT ( 'NONE',  ( 11.14716901145161643, 12.46304090461738667, 6.000000000000000000 ) ) ;
#35653 = DIRECTION ( 'NONE',  ( 1.000000000000000000, 0.000000000000000000, 0.000000000000000000 ) ) ;
#35654 = FACE_OUTER_BOUND ( 'NONE', #24551, .T. ) ;
#35655 = EDGE_LOOP ( 'NONE', ( #39587, #37038, #12025, #17145, #21577, #7529, #5948 ) ) ;
#35656 = CARTESIAN_POINT ( 'NONE',  ( -26.20904522235016287, 5.310845850833655568, -5.477248126412333384 ) ) ;
#35657 = CARTESIAN_POINT ( 'NONE',  ( -6.513333500388862163, 35.89988989478917603, 10.82238861112326234 ) ) ;
#35658 = DIRECTION ( 'NONE',  ( -0.9510565162951518658, 0.3090169943749528914, 0.000000000000000000 ) ) ;
#35659 = CARTESIAN_POINT ( 'NONE',  ( 26.06425415636434906, -22.71578164446442827, -11.11508149911450793 ) ) ;
#35660 = DIRECTION ( 'NONE',  ( -0.000000000000000000, -0.000000000000000000, -1.000000000000000000 ) ) ;
#35661 = CARTESIAN_POINT ( 'NONE',  ( -14.70550430380713003, 20.45163507617063203, 10.87262190629282799 ) ) ;
#35662 = EDGE_CURVE ( 'NONE', #23702, #33679, #287, .T. ) ;
#35663 = CARTESIAN_POINT ( 'NONE',  ( 10.77401535176683822, 17.85200931278258807, -26.79744273874945293 ) ) ;
#35664 =( LENGTH_UNIT ( ) NAMED_UNIT ( * ) SI_UNIT ( .MILLI., .METRE. ) );
#35665 = AXIS2_PLACEMENT_3D ( 'NONE', #39890, #21411, #30765 ) ;
#35666 = VERTEX_POINT ( 'NONE', #2543 ) ;
#35667 = CARTESIAN_POINT ( 'NONE',  ( -14.81419240842891050, 15.18325971397014307, -24.25831821709929415 ) ) ;
#35668 = CARTESIAN_POINT ( 'NONE',  ( -24.18603102892831913, -14.68777056910904832, 20.99999999999995026 ) ) ;
#35669 = EDGE_CURVE ( 'NONE', #14281, #7759, #38646, .T. ) ;
#35670 = CARTESIAN_POINT ( 'NONE',  ( 15.37571132048090838, -26.71368809714059722, -5.474175248281667017 ) ) ;
#35671 = CARTESIAN_POINT ( 'NONE',  ( -8.118377661053488126, 10.47536095541708967, 7.000000000000000000 ) ) ;
#35672 = CARTESIAN_POINT ( 'NONE',  ( 14.74942196309478604, 25.36140116702692637, -10.65398990804295032 ) ) ;
#35673 = ORIENTED_EDGE ( 'NONE', *, *, #14841, .T. ) ;
#35674 = CARTESIAN_POINT ( 'NONE',  ( 11.67905974016245629, 18.91828259921463129, -22.73395179757990547 ) ) ;
#35675 = ORIENTED_EDGE ( 'NONE', *, *, #851, .T. ) ;
#35677 = DIRECTION ( 'NONE',  ( -0.000000000000000000, -0.000000000000000000, -1.000000000000000000 ) ) ;
#35676 = CARTESIAN_POINT ( 'NONE',  ( -11.13871245836219259, 17.78928257176252359, -26.21993262638637034 ) ) ;
#35678 = CARTESIAN_POINT ( 'NONE',  ( -15.33464666325443559, -26.58010993391619792, -6.888001209383307177 ) ) ;
#35679 = CARTESIAN_POINT ( 'NONE',  ( -36.74707368630860316, -16.71203845619708517, 11.55979286843963649 ) ) ;
#35680 = CARTESIAN_POINT ( 'NONE',  ( -30.32740607997149240, -18.32269088211211994, -11.06668654378994887 ) ) ;
#35681 = CARTESIAN_POINT ( 'NONE',  ( -4.810070356376328071, -20.19244794699170953, -26.53957745834831528 ) ) ;
#35682 = CARTESIAN_POINT ( 'NONE',  ( 15.91914112585197216, 24.98921244238988493, -5.946992071948343117 ) ) ;
#35683 = ORIENTED_EDGE ( 'NONE', *, *, #11866, .T. ) ;
#35684 = CARTESIAN_POINT ( 'NONE',  ( 21.66250921451431921, 7.810554196117029058, -16.92292203280336693 ) ) ;
#35685 = DIRECTION ( 'NONE',  ( -0.7071067811865517916, 0.000000000000000000, -0.7071067811865432429 ) ) ;
#35686 = DIRECTION ( 'NONE',  ( 0.000000000000000000, 0.000000000000000000, 1.000000000000000000 ) ) ;
#35687 = DIRECTION ( 'NONE',  ( 0.8090169943749504489, 0.5877852522924689183, 0.000000000000000000 ) ) ;
#35688 = ORIENTED_EDGE ( 'NONE', *, *, #20615, .F. ) ;
#35689 = CARTESIAN_POINT ( 'NONE',  ( -23.96107556257267746, -1.546995113576812964, -20.27043652965265608 ) ) ;
#35690 = CARTESIAN_POINT ( 'NONE',  ( -19.36000459727014444, -2.857032334443094790, 21.00000000000056133 ) ) ;
#35691 = ORIENTED_EDGE ( 'NONE', *, *, #24693, .T. ) ;
#35692 = CARTESIAN_POINT ( 'NONE',  ( 25.82310832280103341, -13.25591304976875939, 20.94377226548379767 ) ) ;
#35693 = DIRECTION ( 'NONE',  ( 1.000000000000000000, 0.000000000000000000, 0.000000000000000000 ) ) ;
#35694 = B_SPLINE_CURVE_WITH_KNOTS ( 'NONE', 3,
 ( #17892, #35970, #30071, #30274, #14632, #5880 ),
 .UNSPECIFIED., .F., .F.,
 ( 4, 2, 4 ),
 ( 0.000000000000000000, 0.5000000000000000000, 1.000000000000000000 ),
 .UNSPECIFIED. ) ;
#35695 = EDGE_CURVE ( 'NONE', #7177, #22373, #15302, .T. ) ;
#35696 = LINE ( 'NONE', #7850, #10605 ) ;
#35697 = CARTESIAN_POINT ( 'NONE',  ( 33.71607969487701695, -17.27553485048664683, -7.545771892860997809 ) ) ;
#35698 = ADVANCED_FACE ( 'NONE', ( #33635 ), #5782, .T. ) ;
#35699 = CARTESIAN_POINT ( 'NONE',  ( 34.10020663062367419, -21.93670956716277587, 11.55979286843929366 ) ) ;
#35700 = AXIS2_PLACEMENT_3D ( 'NONE', #20125, #14219, #26610 ) ;
#35701 = ORIENTED_EDGE ( 'NONE', *, *, #13218, .F. ) ;
#35702 = AXIS2_PLACEMENT_3D ( 'NONE', #6596, #12901, #25297 ) ;
#35703 = CARTESIAN_POINT ( 'NONE',  ( 5.724371395536106633, 32.23037938972932892, 12.00000000000000000 ) ) ;
#35704 = DIRECTION ( 'NONE',  ( 1.000000000000000000, 0.000000000000000000, 0.000000000000000000 ) ) ;
#35705 = CYLINDRICAL_SURFACE ( 'NONE', #11059, 1.000000000000000888 ) ;
#35706 = ORIENTED_EDGE ( 'NONE', *, *, #6558, .T. ) ;
#35707 = CARTESIAN_POINT ( 'NONE',  ( 1.006457374325394838, 24.67265317861021501, -20.69366133597257118 ) ) ;
#35708 = DIRECTION ( 'NONE',  ( -0.8090169943749430104, 0.5877852522924791323, 0.000000000000000000 ) ) ;
#35709 = DIRECTION ( 'NONE',  ( -0.7071067811865449082, 0.7071067811865501263, 0.000000000000000000 ) ) ;
#35710 = CARTESIAN_POINT ( 'NONE',  ( -13.03641663870442891, 15.85735326529964873, 6.000000000000000000 ) ) ;
#35711 = DIRECTION ( 'NONE',  ( 0.000000000000000000, 0.000000000000000000, 1.000000000000000000 ) ) ;
#35712 = ADVANCED_FACE ( 'NONE', ( #10425 ), #38256, .F. ) ;
#35713 = CARTESIAN_POINT ( 'NONE',  ( 9.284827327736225655, 10.70480225628988791, 10.49999999999999822 ) ) ;
#35714 = CARTESIAN_POINT ( 'NONE',  ( 11.19449165307062266, 21.93316151188967922, -19.27160384251886427 ) ) ;
#35715 = CARTESIAN_POINT ( 'NONE',  ( -39.48531003256149319, -11.24999992065011156, 11.00000000000000000 ) ) ;
#35716 = EDGE_LOOP ( 'NONE', ( #32181, #16403, #15970, #27118 ) ) ;
#35717 = VECTOR ( 'NONE', #20262, 1000.000000000000114 ) ;
#35719 = CARTESIAN_POINT ( 'NONE',  ( 5.348106467989403257, 35.16482219193073178, 12.00000000000000000 ) ) ;
#35718 = CARTESIAN_POINT ( 'NONE',  ( -19.77774007911304821, 14.30023323257737466, -10.37717975262850878 ) ) ;
#35720 = CARTESIAN_POINT ( 'NONE',  ( 6.706335727061685681, 24.35410196624994583, 6.000000000000000000 ) ) ;
#35721 = ADVANCED_FACE ( 'NONE', ( #38457 ), #31360, .T. ) ;
#35722 = CARTESIAN_POINT ( 'NONE',  ( 9.805821007926871502, -18.55489467393325853, -26.22290329400297537 ) ) ;
#35723 = CARTESIAN_POINT ( 'NONE',  ( 14.84160187385922036, 20.32586711126977974, 7.000000000000000000 ) ) ;
#35724 = CARTESIAN_POINT ( 'NONE',  ( 15.35452447619515226, 26.73442772235758014, -6.416210666809704755 ) ) ;
#35725 = CARTESIAN_POINT ( 'NONE',  ( -22.52744239175981278, -0.1803094636421871677, -20.90349153980994501 ) ) ;
#35726 = DIRECTION ( 'NONE',  ( 1.000000000000000000, 0.000000000000000000, 0.000000000000000000 ) ) ;
#35727 = EDGE_CURVE ( 'NONE', #29069, #16528, #15923, .T. ) ;
#35728 = CARTESIAN_POINT ( 'NONE',  ( -15.11226011019654436, -14.18218723851762597, -27.77779782121918473 ) ) ;
#35729 = CARTESIAN_POINT ( 'NONE',  ( 3.028292443394525524, -21.32411716264335766, -22.21865855438248971 ) ) ;
#35730 = CARTESIAN_POINT ( 'NONE',  ( 11.12785985892924678, 17.21691741209329862, -29.99999999999999289 ) ) ;
#35731 = CARTESIAN_POINT ( 'NONE',  ( 17.78979992564072887, 12.92841434147965352, -20.10125189250855726 ) ) ;
#35732 = DIRECTION ( 'NONE',  ( 1.000000000000000000, 0.000000000000000000, 0.000000000000000000 ) ) ;
#35733 = ORIENTED_EDGE ( 'NONE', *, *, #39089, .F. ) ;
#35734 = VECTOR ( 'NONE', #25597, 1000.000000000000000 ) ;
#35735 = CARTESIAN_POINT ( 'NONE',  ( -4.114515543405717679, 20.32799847914411373, -27.75925566174262826 ) ) ;
#35736 = ORIENTED_EDGE ( 'NONE', *, *, #28179, .T. ) ;
#35737 = CARTESIAN_POINT ( 'NONE',  ( 14.70895476143395442, 21.92515157238277013, 10.49999999999999822 ) ) ;
#35738 = ORIENTED_EDGE ( 'NONE', *, *, #37029, .F. ) ;
#35739 = DIRECTION ( 'NONE',  ( 0.000000000000000000, 0.000000000000000000, -1.000000000000000000 ) ) ;
#35740 = CARTESIAN_POINT ( 'NONE',  ( 9.067459072332447079, 10.87036407658120041, 10.94387467463491603 ) ) ;
#35741 = ORIENTED_EDGE ( 'NONE', *, *, #9261, .F. ) ;
#35742 = CARTESIAN_POINT ( 'NONE',  ( -30.19601209477679760, 0.1621268579053716241, -8.299309318683974368 ) ) ;
#35743 = ADVANCED_FACE ( 'NONE', ( #22607 ), #37848, .T. ) ;
#35744 = VERTEX_POINT ( 'NONE', #25855 ) ;
#35745 = CARTESIAN_POINT ( 'NONE',  ( 20.60227848500122860, -5.552195928352420928, -25.73354454585938811 ) ) ;
#35746 = EDGE_CURVE ( 'NONE', #28188, #4088, #36710, .T. ) ;
#35747 = CIRCLE ( 'NONE', #39617, 15.00000000000000000 ) ;
#35748 = ORIENTED_EDGE ( 'NONE', *, *, #1055, .F. ) ;
#35749 = CARTESIAN_POINT ( 'NONE',  ( 0.000000000000000000, 0.000000000000000000, 0.000000000000000000 ) ) ;
#35750 = CARTESIAN_POINT ( 'NONE',  ( 10.67401460142006897, 33.03905331147102231, 7.485646746502373716 ) ) ;
#35751 = ORIENTED_EDGE ( 'NONE', *, *, #36962, .F. ) ;
#35752 = DIRECTION ( 'NONE',  ( 0.000000000000000000, 0.000000000000000000, 1.000000000000000000 ) ) ;
#35753 = CARTESIAN_POINT ( 'NONE',  ( 4.583318357746482441, 36.10598097934258277, 17.92354375535250810 ) ) ;
#35754 = DIRECTION ( 'NONE',  ( 0.000000000000000000, 0.000000000000000000, 1.000000000000000000 ) ) ;
#35755 = ORIENTED_EDGE ( 'NONE', *, *, #2575, .F. ) ;
#35756 = DIRECTION ( 'NONE',  ( 0.000000000000000000, 0.000000000000000000, 1.000000000000000000 ) ) ;
#35757 = CARTESIAN_POINT ( 'NONE',  ( 7.713869163865849643, 10.18146832927074996, 11.00000000000000000 ) ) ;
#35758 = CIRCLE ( 'NONE', #18249, 1.000000000000000000 ) ;
#35759 = DIRECTION ( 'NONE',  ( -1.000000000000000000, 0.000000000000000000, 0.000000000000000000 ) ) ;
#35760 = CARTESIAN_POINT ( 'NONE',  ( 18.93676227246565702, 16.79700351661384161, -7.901259146623853091 ) ) ;
#35761 = CARTESIAN_POINT ( 'NONE',  ( 5.727250998068078580, 19.76148542614543047, -28.52014932781858292 ) ) ;
#35762 = ORIENTED_EDGE ( 'NONE', *, *, #20895, .T. ) ;
#35763 = CARTESIAN_POINT ( 'NONE',  ( -6.143904198944369455, -13.77689918168226413, 20.99999999999999645 ) ) ;
#35764 = LINE ( 'NONE', #13814, #38267 ) ;
#35765 = EDGE_CURVE ( 'NONE', #35530, #25471, #37371, .T. ) ;
#35766 = CARTESIAN_POINT ( 'NONE',  ( 9.819171776840725840, -18.04961070180578986, -28.69512037941552407 ) ) ;
#35767 = CYLINDRICAL_SURFACE ( 'NONE', #19756, 0.5000000000000004441 ) ;
#35768 = DIRECTION ( 'NONE',  ( 0.7032331762533998720, -0.07391278520356875381, -0.7071067811865517916 ) ) ;
#35769 = VERTEX_POINT ( 'NONE', #6761 ) ;
#35770 = CARTESIAN_POINT ( 'NONE',  ( -11.00327412694905860, 17.34993409992508973, -28.70683927363747401 ) ) ;
#35771 = AXIS2_PLACEMENT_3D ( 'NONE', #26247, #38645, #10819 ) ;
#35772 = CARTESIAN_POINT ( 'NONE',  ( -15.48695972777900742, -26.74878859331914072, 16.30093088680190405 ) ) ;
#35773 = CARTESIAN_POINT ( 'NONE',  ( 12.95888722777509727, -25.15559516903838500, -10.68953037264193817 ) ) ;
#35774 = AXIS2_PLACEMENT_3D ( 'NONE', #21355, #15256, #24398 ) ;
#35775 = CARTESIAN_POINT ( 'NONE',  ( -9.705584749708384251, 11.06314620770957013, 7.221809905720049549 ) ) ;
#35776 = ORIENTED_EDGE ( 'NONE', *, *, #33112, .F. ) ;
#35777 = ORIENTED_EDGE ( 'NONE', *, *, #39048, .T. ) ;
#35778 = CARTESIAN_POINT ( 'NONE',  ( -7.247758014959435613, 19.72005091410585464, -26.50610415850021795 ) ) ;
#35779 = LINE ( 'NONE', #20342, #24347 ) ;
#35780 = FACE_BOUND ( 'NONE', #9099, .T. ) ;
#35781 = CARTESIAN_POINT ( 'NONE',  ( -34.24415449774322440, -5.469239270874415304, -6.781267690620076394 ) ) ;
#35782 = DIRECTION ( 'NONE',  ( 0.000000000000000000, 0.000000000000000000, -1.000000000000000000 ) ) ;
#35783 = ORIENTED_EDGE ( 'NONE', *, *, #6545, .F. ) ;
#35784 = CARTESIAN_POINT ( 'NONE',  ( 20.47879743316550005, 0.9320964914785054845, -29.34969434330313831 ) ) ;
#35785 = CARTESIAN_POINT ( 'NONE',  ( -8.294006203984645609, 33.46401007850805343, 12.00000000000000000 ) ) ;
#35786 = DIRECTION ( 'NONE',  ( 0.6037757019622738142, 0.000000000000000000, -0.7971542521494591194 ) ) ;
#35787 = CARTESIAN_POINT ( 'NONE',  ( -31.59094081668067844, -24.64165453824189100, 11.00000000000001776 ) ) ;
#35788 = EDGE_LOOP ( 'NONE', ( #2333, #31520, #531, #39463, #465, #32643, #35582 ) ) ;
#35789 = CARTESIAN_POINT ( 'NONE',  ( -30.00917842038222005, 0.01052955857392639215, -9.237561733509775053 ) ) ;
#35790 = DIRECTION ( 'NONE',  ( -0.000000000000000000, 0.000000000000000000, 1.000000000000000000 ) ) ;
#35791 = ORIENTED_EDGE ( 'NONE', *, *, #24166, .T. ) ;
#35792 = CARTESIAN_POINT ( 'NONE',  ( 29.56647952434581583, -2.710646861654836925, -13.25517925932730456 ) ) ;
#35793 = CARTESIAN_POINT ( 'NONE',  ( 36.26963650278469231, -7.248637393400325202, 14.53008259254015044 ) ) ;
#35794 = ORIENTED_EDGE ( 'NONE', *, *, #33261, .T. ) ;
#35795 = CARTESIAN_POINT ( 'NONE',  ( 14.44241962112810285, 32.29667252612951245, 13.92931973827809600 ) ) ;
#35796 = EDGE_CURVE ( 'NONE', #31499, #37740, #22809, .T. ) ;
#35797 = CARTESIAN_POINT ( 'NONE',  ( 10.35515495761407756, -25.90830221531241406, 15.72805884748740546 ) ) ;
#35798 = CARTESIAN_POINT ( 'NONE',  ( 11.78893975237933134, 23.27376113029817617, 13.00000000000000178 ) ) ;
#35799 = CARTESIAN_POINT ( 'NONE',  ( -7.962467718762158420, 24.71319220551421481, 20.69868183039781329 ) ) ;
#35800 = CYLINDRICAL_SURFACE ( 'NONE', #38856, 1.000000000000000888 ) ;
#35801 = ORIENTED_EDGE ( 'NONE', *, *, #14799, .F. ) ;
#35802 = VECTOR ( 'NONE', #11763, 999.9999999999998863 ) ;
#35803 = DIRECTION ( 'NONE',  ( 1.000000000000000000, 0.000000000000000000, 0.000000000000000000 ) ) ;
#35804 = CARTESIAN_POINT ( 'NONE',  ( 2.680372758886228279, 20.41866721373630966, -28.46039174759823709 ) ) ;
#35805 = CARTESIAN_POINT ( 'NONE',  ( -11.44473057578096764, 31.45924896672619298, 7.000000000000000000 ) ) ;
#35806 = CARTESIAN_POINT ( 'NONE',  ( 18.38177052346872387, 3.916595739918349750, 20.50957957746022586 ) ) ;
#35807 = AXIS2_PLACEMENT_3D ( 'NONE', #3643, #15841, #28423 ) ;
#35808 = CARTESIAN_POINT ( 'NONE',  ( 16.81687198955598461, -22.15028281434977231, -16.05891094166905475 ) ) ;
#35809 = DIRECTION ( 'NONE',  ( -0.000000000000000000, -0.000000000000000000, -1.000000000000000000 ) ) ;
#35810 = CARTESIAN_POINT ( 'NONE',  ( -13.05736835487441994, 16.11602540378456538, 10.49999999999999822 ) ) ;
#35811 = DIRECTION ( 'NONE',  ( 0.000000000000000000, -0.000000000000000000, 1.000000000000000000 ) ) ;
#35812 = CARTESIAN_POINT ( 'NONE',  ( 14.89744943408475564, 25.91887218477155130, -9.702362698303520716 ) ) ;
#35813 = VERTEX_POINT ( 'NONE', #35206 ) ;
#35814 = CARTESIAN_POINT ( 'NONE',  ( -15.12259515852657898, 25.63742652657455778, -9.242452702712727231 ) ) ;
#35815 = CARTESIAN_POINT ( 'NONE',  ( -30.54456991890724638, -14.74984208377938621, 19.66345542862526230 ) ) ;
#35816 = EDGE_CURVE ( 'NONE', #9639, #23635, #19771, .T. ) ;
#35817 = CARTESIAN_POINT ( 'NONE',  ( 4.244284213106223724, 8.112413639933444998, 7.203056206335832989 ) ) ;
#35818 = CARTESIAN_POINT ( 'NONE',  ( 14.56114463551361204, 24.89209121383319001, -11.60131081651779184 ) ) ;
#35819 = VERTEX_POINT ( 'NONE', #4326 ) ;
#35820 = CARTESIAN_POINT ( 'NONE',  ( 17.33150493693412031, -10.96591108411289639, -30.00000000000002842 ) ) ;
#35821 = ORIENTED_EDGE ( 'NONE', *, *, #27780, .F. ) ;
#35823 = DIRECTION ( 'NONE',  ( 1.000000000000000000, 0.000000000000000000, 0.000000000000000000 ) ) ;
#35822 = CARTESIAN_POINT ( 'NONE',  ( -10.60445392351956073, 17.59993408138762661, -28.69024928499496241 ) ) ;
#35824 = CARTESIAN_POINT ( 'NONE',  ( -10.20341636066711288, -17.78360352085077878, -29.33359148140973005 ) ) ;
#35825 = CARTESIAN_POINT ( 'NONE',  ( -7.294006203984644721, 33.46401007850805343, 12.00000000000000000 ) ) ;
#35826 = ORIENTED_EDGE ( 'NONE', *, *, #12614, .F. ) ;
#35827 = CARTESIAN_POINT ( 'NONE',  ( -33.68730855286997183, -13.89000784508904829, -9.301074370182135453 ) ) ;
#35828 = CARTESIAN_POINT ( 'NONE',  ( -9.617329463714023419, -18.95265504179631932, -25.05348104573760537 ) ) ;
#35829 = LINE ( 'NONE', #29531, #11862 ) ;
#35830 = CARTESIAN_POINT ( 'NONE',  ( 14.60200688919959688, 18.24034312353848009, -18.75124519320161554 ) ) ;
#35831 = ORIENTED_EDGE ( 'NONE', *, *, #2684, .T. ) ;
#35832 = CARTESIAN_POINT ( 'NONE',  ( 22.40999101807990712, 3.009793452745128661, -20.80770581881638392 ) ) ;
#35833 = CARTESIAN_POINT ( 'NONE',  ( -1.829593030691901284E-15, 22.50000000000001066, 3.000000000000000000 ) ) ;
#35834 = CARTESIAN_POINT ( 'NONE',  ( -23.09341953181386131, -31.04079623447002234, 22.99999999999905853 ) ) ;
#35835 = ORIENTED_EDGE ( 'NONE', *, *, #19306, .F. ) ;
#35836 = CARTESIAN_POINT ( 'NONE',  ( -25.30972341225729139, 0.2006976411555125572, -17.41501298532444864 ) ) ;
#35837 = CARTESIAN_POINT ( 'NONE',  ( 30.64785752585394718, -0.7125550944224900984, -9.193437879178903316 ) ) ;
#35838 = CARTESIAN_POINT ( 'NONE',  ( 27.60461630348735440, -20.46464247653215551, 19.27171037444157875 ) ) ;
#35839 = ADVANCED_FACE ( 'NONE', ( #16123 ), #19419, .T. ) ;
#35840 = EDGE_LOOP ( 'NONE', ( #21603, #12428 ) ) ;
#35841 = CARTESIAN_POINT ( 'NONE',  ( -28.74177917110700875, 1.753266042911047373, -8.316192635012841450 ) ) ;
#35842 = CARTESIAN_POINT ( 'NONE',  ( -13.47223693944937040, 18.09844039693852125, -21.24786896499725231 ) ) ;
#35843 = CARTESIAN_POINT ( 'NONE',  ( 7.126083911573381613, 10.99048532364570008, 9.500000000000000000 ) ) ;
#35844 = CARTESIAN_POINT ( 'NONE',  ( 7.559505275947156377, 25.28115294937476065, 6.000000000000000000 ) ) ;
#35845 = EDGE_CURVE ( 'NONE', #30103, #488, #372, .T. ) ;
#35846 = ADVANCED_FACE ( 'NONE', ( #35014 ), #27623, .T. ) ;
#35847 = CARTESIAN_POINT ( 'NONE',  ( -4.727507481117091181, 31.88885898370948269, 10.50000000000000000 ) ) ;
#35848 = CARTESIAN_POINT ( 'NONE',  ( -7.559512017365658920, 19.71884705062586107, 12.00000000000000000 ) ) ;
#35849 = CIRCLE ( 'NONE', #23528, 1.000000000000000888 ) ;
#35850 = LINE ( 'NONE', #17176, #14643 ) ;
#35851 = ORIENTED_EDGE ( 'NONE', *, *, #35571, .F. ) ;
#35852 = CARTESIAN_POINT ( 'NONE',  ( -21.24220381125994805, 5.046223848463253780, -22.05423595162513450 ) ) ;
#35853 = CARTESIAN_POINT ( 'NONE',  ( 2.525645716490525494, 8.212903943950921715, 11.00000000000000000 ) ) ;
#35854 = LINE ( 'NONE', #35250, #24639 ) ;
#35855 = CARTESIAN_POINT ( 'NONE',  ( 26.32663925810967953, -25.71384748841218837, -5.442504371432549171 ) ) ;
#35856 = CARTESIAN_POINT ( 'NONE',  ( 10.44103466624280685, 32.57396620494213124, 7.000000000000000000 ) ) ;
#35857 = FACE_OUTER_BOUND ( 'NONE', #9743, .T. ) ;
#35858 = CARTESIAN_POINT ( 'NONE',  ( 11.64919678992194640, 19.63822387691775262, -21.57097631828376194 ) ) ;
#35859 = CIRCLE ( 'NONE', #37794, 15.00000000000000000 ) ;
#35860 = CARTESIAN_POINT ( 'NONE',  ( 13.47830981910552062, 21.58612669357076896, 10.00000000000000000 ) ) ;
#35861 = ORIENTED_EDGE ( 'NONE', *, *, #22246, .F. ) ;
#35862 = CARTESIAN_POINT ( 'NONE',  ( -16.55555455799639830, 22.89925119996338765, -6.424656108638855834 ) ) ;
#35863 = CARTESIAN_POINT ( 'NONE',  ( -24.69586183797187218, -8.725643957992190280, 20.99999999999999645 ) ) ;
#35864 = ADVANCED_FACE ( 'NONE', ( #26668 ), #6095, .T. ) ;
#35865 = AXIS2_PLACEMENT_3D ( 'NONE', #8956, #36987, #24594 ) ;
#35866 = CARTESIAN_POINT ( 'NONE',  ( 14.76729391302192695, -25.81058457567449338, -9.710596626364806028 ) ) ;
#35867 = ADVANCED_FACE ( 'NONE', ( #30123 ), #23821, .T. ) ;
#35868 = LINE ( 'NONE', #11292, #16583 ) ;
#35869 = CARTESIAN_POINT ( 'NONE',  ( 11.04758111719894309, 17.42002116339528683, -28.07786199837244112 ) ) ;
#35870 = ORIENTED_EDGE ( 'NONE', *, *, #37409, .F. ) ;
#35871 = DIRECTION ( 'NONE',  ( 0.5877852522924690293, -0.8090169943749504489, 0.000000000000000000 ) ) ;
#35872 = ORIENTED_EDGE ( 'NONE', *, *, #23047, .T. ) ;
#35874 = FACE_OUTER_BOUND ( 'NONE', #24860, .T. ) ;
#35873 = CARTESIAN_POINT ( 'NONE',  ( -15.38296630468078874, 26.90060637120896558, -5.473630184351862660 ) ) ;
#35875 = CARTESIAN_POINT ( 'NONE',  ( -15.19613505986383473, -26.28779615057171881, -8.296983900613629004 ) ) ;
#35876 = CARTESIAN_POINT ( 'NONE',  ( -36.04785107591563786, -18.56329043283760072, 10.99999999999982592 ) ) ;
#35877 = VECTOR ( 'NONE', #846, 1000.000000000000114 ) ;
#35878 = CARTESIAN_POINT ( 'NONE',  ( -24.91495442474104749, -15.04743612541264852, -16.62452746883704791 ) ) ;
#35879 = CARTESIAN_POINT ( 'NONE',  ( -8.832931388505667059, -24.56742532686079272, -10.78344481105500385 ) ) ;
#35880 = CARTESIAN_POINT ( 'NONE',  ( 15.56695106341455848, 24.30445274633115815, -9.260401158391204035 ) ) ;
#35881 = ORIENTED_EDGE ( 'NONE', *, *, #797, .T. ) ;
#35882 = CARTESIAN_POINT ( 'NONE',  ( 20.64360361735735339, 8.470246920354872699, -19.02919037500957700 ) ) ;
#35883 = CARTESIAN_POINT ( 'NONE',  ( 12.05832241004688399, 18.99596958976722760, -21.04195414767209726 ) ) ;
#35884 = CARTESIAN_POINT ( 'NONE',  ( -12.51665927450813953, 14.23331522619103851, 7.382773698552465014 ) ) ;
#35885 = DIRECTION ( 'NONE',  ( 1.000000000000000000, 0.000000000000000000, 0.000000000000000000 ) ) ;
#35886 = ORIENTED_EDGE ( 'NONE', *, *, #4282, .T. ) ;
#35887 = CARTESIAN_POINT ( 'NONE',  ( -20.74499114794467758, -1.156592509646555689, -27.31797897823820520 ) ) ;
#35888 = CIRCLE ( 'NONE', #37185, 0.5000000000000004441 ) ;
#35889 = CARTESIAN_POINT ( 'NONE',  ( -4.817371740575532080, 23.83900317890012843, 20.99999999999999645 ) ) ;
#35890 = AXIS2_PLACEMENT_3D ( 'NONE', #12419, #12223, #12022 ) ;
#35891 = CARTESIAN_POINT ( 'NONE',  ( 25.95165700074904080, -9.707988825433883306, 20.94377226548378346 ) ) ;
#35892 = CARTESIAN_POINT ( 'NONE',  ( -5.362728154696096539, 13.41753630677062148, 10.50000000000000000 ) ) ;
#35893 = ADVANCED_FACE ( 'NONE', ( #16933 ), #26267, .F. ) ;
#35894 = CARTESIAN_POINT ( 'NONE',  ( -8.910254037844422825, 17.93301270189230223, 10.49999999999999822 ) ) ;
#35895 = CARTESIAN_POINT ( 'NONE',  ( 26.22005807680820766, -12.44079363307010233, -16.63921512830654237 ) ) ;
#35896 = AXIS2_PLACEMENT_3D ( 'NONE', #20324, #32923, #11177 ) ;
#35897 = CARTESIAN_POINT ( 'NONE',  ( 7.133890061153794093, 30.26901619224539886, 10.50000000000000000 ) ) ;
#35898 = ORIENTED_EDGE ( 'NONE', *, *, #17514, .F. ) ;
#35899 = LINE ( 'NONE', #32456, #13887 ) ;
#35900 = EDGE_CURVE ( 'NONE', #12849, #10495, #19183, .T. ) ;
#35901 = VECTOR ( 'NONE', #1221, 1000.000000000000000 ) ;
#35902 = CARTESIAN_POINT ( 'NONE',  ( 6.856644039074955899, 35.52575270032630073, 10.49999999999999822 ) ) ;
#35903 = ORIENTED_EDGE ( 'NONE', *, *, #12815, .T. ) ;
#35904 = CARTESIAN_POINT ( 'NONE',  ( 0.2213127261196708995, 20.90796579412245748, -26.96645221465433551 ) ) ;
#35905 = DIRECTION ( 'NONE',  ( 1.000000000000000000, 0.000000000000000000, 0.000000000000000000 ) ) ;
#35906 = DIRECTION ( 'NONE',  ( 0.2079116908177533751, -0.9781476007338069101, 0.000000000000000000 ) ) ;
#35907 = LINE ( 'NONE', #5225, #40037 ) ;
#35908 = DIRECTION ( 'NONE',  ( 0.000000000000000000, 0.000000000000000000, 1.000000000000000000 ) ) ;
#35909 = VECTOR ( 'NONE', #3764, 1000.000000000000000 ) ;
#35910 = DIRECTION ( 'NONE',  ( 0.000000000000000000, 0.000000000000000000, 1.000000000000000000 ) ) ;
#35911 = CARTESIAN_POINT ( 'NONE',  ( 14.65960527224459931, 28.71189413793838341, -6.386546476000780181 ) ) ;
#35912 = CARTESIAN_POINT ( 'NONE',  ( -12.74038105676665289, 14.56698729810790027, 10.49999999999999822 ) ) ;
#35913 = ORIENTED_EDGE ( 'NONE', *, *, #39393, .F. ) ;
#35915 = DIRECTION ( 'NONE',  ( -0.9135454576426046414, -0.4067366430757919371, 0.000000000000000000 ) ) ;
#35914 = CARTESIAN_POINT ( 'NONE',  ( -18.68060247292710585, 14.65156323798503912, -13.87922052841179799 ) ) ;
#35916 = AXIS2_PLACEMENT_3D ( 'NONE', #32663, #4619, #20470 ) ;
#35917 = DIRECTION ( 'NONE',  ( 0.000000000000000000, 0.000000000000000000, 1.000000000000000000 ) ) ;
#35918 = CARTESIAN_POINT ( 'NONE',  ( 15.26849416126754910, -26.39863181468341580, -7.827248033921830661 ) ) ;
#35919 = CARTESIAN_POINT ( 'NONE',  ( 8.806975420853749625, 31.15003855377755571, 6.000000000000000000 ) ) ;
#35920 = CARTESIAN_POINT ( 'NONE',  ( 15.40660648310854164, 26.81700542816128063, -5.000000000000000000 ) ) ;
#35921 = CARTESIAN_POINT ( 'NONE',  ( 9.163310636333564574, 20.63632441393291117, -20.55760979252978871 ) ) ;
#35922 = CARTESIAN_POINT ( 'NONE',  ( -20.91708001959888108, -16.07177359997633559, 23.00000000000000000 ) ) ;
#35923 = EDGE_CURVE ( 'NONE', #10078, #34816, #39714, .T. ) ;
#35924 = AXIS2_PLACEMENT_3D ( 'NONE', #3765, #329, #6604 ) ;
#35925 = CARTESIAN_POINT ( 'NONE',  ( -14.94827155352230186, -14.02787326271796609, -29.23873448612896553 ) ) ;
#35926 = CARTESIAN_POINT ( 'NONE',  ( 4.439926597751906456, -20.64563978286073365, -24.32161315903661247 ) ) ;
#35927 = CARTESIAN_POINT ( 'NONE',  ( 11.88552478615052976, 18.71945594169985938, -22.76728644064645124 ) ) ;
#35928 = CARTESIAN_POINT ( 'NONE',  ( 19.02469128737116577, 14.03524138465703253, -13.88975380088736955 ) ) ;
#35929 = COLOUR_RGB ( '', 0.66274510, 0.83137255, 0.94901961) ;
#35930 = DIRECTION ( 'NONE',  ( -0.000000000000000000, -0.000000000000000000, -1.000000000000000000 ) ) ;
#35931 = EDGE_LOOP ( 'NONE', ( #34272, #244, #37382, #6418 ) ) ;
#35932 = CARTESIAN_POINT ( 'NONE',  ( -7.388453759928180098, 36.32445320202015893, -7.146513852312973647 ) ) ;
#35933 = ORIENTED_EDGE ( 'NONE', *, *, #18952, .T. ) ;
#35934 = AXIS2_PLACEMENT_3D ( 'NONE', #30852, #8715, #39386 ) ;
#35935 = LINE ( 'NONE', #8092, #18320 ) ;
#35936 = ORIENTED_EDGE ( 'NONE', *, *, #14597, .T. ) ;
#35937 = DIRECTION ( 'NONE',  ( 0.000000000000000000, -0.6729908358753734499, 0.7396508195275431907 ) ) ;
#35938 = CYLINDRICAL_SURFACE ( 'NONE', #16108, 0.4999999999999988898 ) ;
#35939 = EDGE_LOOP ( 'NONE', ( #24741, #18354, #37341 ) ) ;
#35940 = CARTESIAN_POINT ( 'NONE',  ( -29.94001474276964814, 0.4362189444618576606, -8.302034482558056538 ) ) ;
#35941 = EDGE_CURVE ( 'NONE', #24748, #19049, #23069, .T. ) ;
#35942 = ORIENTED_EDGE ( 'NONE', *, *, #36181, .T. ) ;
#35943 = CARTESIAN_POINT ( 'NONE',  ( 31.03616632986720347, -9.319775343359541608, -12.97620689962225704 ) ) ;
#35944 = AXIS2_PLACEMENT_3D ( 'NONE', #31395, #7199, #13702 ) ;
#35945 = EDGE_CURVE ( 'NONE', #34434, #37407, #11236, .T. ) ;
#35946 = ORIENTED_EDGE ( 'NONE', *, *, #36882, .F. ) ;
#35947 = ITEM_DEFINED_TRANSFORMATION ( 'NONE', 'NONE', #7343,  #24238 ) ;
#35948 = CARTESIAN_POINT ( 'NONE',  ( -0.6237384431625470071, 19.56555719779890978, 6.000000000000000000 ) ) ;
#35949 = ORIENTED_EDGE ( 'NONE', *, *, #16305, .T. ) ;
#35950 = CARTESIAN_POINT ( 'NONE',  ( 18.74997338759060028, -3.362744936764432868, 21.00000000000000000 ) ) ;
#35951 = LINE ( 'NONE', #8106, #10474 ) ;
#35952 = CARTESIAN_POINT ( 'NONE',  ( 11.36267260525735878, 30.20759924275323982, 18.42518152272109333 ) ) ;
#35953 = EDGE_CURVE ( 'NONE', #34728, #23552, #1487, .T. ) ;
#35954 = DIRECTION ( 'NONE',  ( 0.000000000000000000, 0.000000000000000000, 1.000000000000000000 ) ) ;
#35955 = VERTEX_POINT ( 'NONE', #5334 ) ;
#35956 =( NAMED_UNIT ( * ) PLANE_ANGLE_UNIT ( ) SI_UNIT ( $, .RADIAN. ) );
#35957 = CARTESIAN_POINT ( 'NONE',  ( -13.18357918683125618, -15.75518424256909888, -30.00000000000001066 ) ) ;
#35958 = DIRECTION ( 'NONE',  ( 0.000000000000000000, 0.000000000000000000, 1.000000000000000000 ) ) ;
#35959 = CARTESIAN_POINT ( 'NONE',  ( -0.5459530983554620187, 27.50006522574757284, 23.00000000000000355 ) ) ;
#35960 = CARTESIAN_POINT ( 'NONE',  ( 19.07008944147191443, 16.95185708702321747, -5.000000000000002665 ) ) ;
#35961 = CARTESIAN_POINT ( 'NONE',  ( 7.014095819933510612, 19.62255229036581738, -27.16548337421515669 ) ) ;
#35962 = VECTOR ( 'NONE', #6595, 1000.000000000000000 ) ;
#35963 = EDGE_LOOP ( 'NONE', ( #20352, #16564, #38810, #19722 ) ) ;
#35964 = DIRECTION ( 'NONE',  ( 0.000000000000000000, 0.000000000000000000, 1.000000000000000000 ) ) ;
#35965 = LINE ( 'NONE', #17487, #5850 ) ;
#35966 = CARTESIAN_POINT ( 'NONE',  ( 13.60193512794777249, -23.64579311371437598, -14.45468143796861327 ) ) ;
#35967 = CARTESIAN_POINT ( 'NONE',  ( -2.494943660522439099, 10.76222879119470832, 13.00000000000000178 ) ) ;
#35968 = ADVANCED_FACE ( 'NONE', ( #14477 ), #7572, .F. ) ;
#35969 = EDGE_CURVE ( 'NONE', #1935, #24077, #8709, .T. ) ;
#35970 = CARTESIAN_POINT ( 'NONE',  ( -9.004335565032201671, 10.95724613078633425, 11.00000000000000000 ) ) ;
#35971 = EDGE_CURVE ( 'NONE', #16598, #7337, #38660, .T. ) ;
#35972 = CARTESIAN_POINT ( 'NONE',  ( -14.93437990693434614, 25.80124217664804931, -9.708838696810092372 ) ) ;
#35973 = AXIS2_PLACEMENT_3D ( 'NONE', #32468, #25947, #10931 ) ;
#35974 = CARTESIAN_POINT ( 'NONE',  ( -33.26300037445958679, -0.3730773600921533650, 13.92931973827787573 ) ) ;
#35975 = CARTESIAN_POINT ( 'NONE',  ( 13.26340735356318135, -25.63066692232520793, -9.260339685793301356 ) ) ;
#35976 = CARTESIAN_POINT ( 'NONE',  ( -9.451751316756979548, 10.85217908230550599, 7.439083675050419231 ) ) ;
#35977 = ORIENTED_EDGE ( 'NONE', *, *, #789, .F. ) ;
#35978 = VERTEX_POINT ( 'NONE', #27666 ) ;
#35979 = CARTESIAN_POINT ( 'NONE',  ( -11.90375846996125020, 33.19065507634929446, -5.449804871099760639 ) ) ;
#35980 = FACE_OUTER_BOUND ( 'NONE', #19475, .T. ) ;
#35981 = CARTESIAN_POINT ( 'NONE',  ( -14.26585111513660031, 17.86474508437623143, 6.000000000000000000 ) ) ;
#35982 = AXIS2_PLACEMENT_3D ( 'NONE', #23971, #20128, #32725 ) ;
#35983 = CARTESIAN_POINT ( 'NONE',  ( -21.43593173410406294, -3.250475320730803031, -24.59978728874802201 ) ) ;
#35984 = CARTESIAN_POINT ( 'NONE',  ( -13.48130249190472796, 27.93180293473203690, 7.499999999999993783 ) ) ;
#35985 = ORIENTED_EDGE ( 'NONE', *, *, #31965, .T. ) ;
#35986 = CARTESIAN_POINT ( 'NONE',  ( 26.47025118594213922, 0.3293273261899055115, -15.45460282459215584 ) ) ;
#35987 = CARTESIAN_POINT ( 'NONE',  ( 9.892954722048902028, 20.95745441963929068, 10.00000000000000000 ) ) ;
#35988 = CARTESIAN_POINT ( 'NONE',  ( -14.09933648065464062, 26.02968990214173317, 10.50000000000000533 ) ) ;
#35989 = CARTESIAN_POINT ( 'NONE',  ( -2.036571916123811388, 8.108948098542073879, 10.49999999999999822 ) ) ;
#35990 = ORIENTED_EDGE ( 'NONE', *, *, #6636, .F. ) ;
#35991 = CARTESIAN_POINT ( 'NONE',  ( -27.13259105340829080, 0.2465074430099665204, -14.47731736851761930 ) ) ;
#35992 = CARTESIAN_POINT ( 'NONE',  ( -5.440908595777636414, 35.94977745735568675, 10.99999999999999289 ) ) ;
#35993 = EDGE_CURVE ( 'NONE', #29721, #33995, #8203, .T. ) ;
#35994 = ORIENTED_EDGE ( 'NONE', *, *, #20742, .T. ) ;
#35995 = CARTESIAN_POINT ( 'NONE',  ( 26.85449993285726578, -3.950704618538266821, -16.99524324133061626 ) ) ;
#35996 = VECTOR ( 'NONE', #28647, 1000.000000000000227 ) ;
#35997 = CARTESIAN_POINT ( 'NONE',  ( 35.65094714180980162, -16.36533849799540263, 15.13084544680208765 ) ) ;
#35998 = EDGE_CURVE ( 'NONE', #20584, #25338, #21133, .T. ) ;
#35999 = EDGE_LOOP ( 'NONE', ( #4542, #26469, #20323 ) ) ;
#36000 = CARTESIAN_POINT ( 'NONE',  ( -7.110004120643877989, 37.89265721834145495, 15.13084544680205923 ) ) ;
#36001 = CARTESIAN_POINT ( 'NONE',  ( -11.18737074829503797, -21.01894785647694519, 19.66345542862620732 ) ) ;
#36002 = CARTESIAN_POINT ( 'NONE',  ( 7.688300058587269170, 16.47782454277055564, 12.00000000000000000 ) ) ;
#36003 = CARTESIAN_POINT ( 'NONE',  ( 6.606253895085748340, 26.00827916197615863, 20.82122704794080548 ) ) ;
#36004 = CARTESIAN_POINT ( 'NONE',  ( -3.596545519285825776, 7.984450832230675310, 10.76099332938163755 ) ) ;
#36005 = ORIENTED_EDGE ( 'NONE', *, *, #37701, .T. ) ;
#36006 = DIRECTION ( 'NONE',  ( 0.000000000000000000, 0.000000000000000000, 1.000000000000000000 ) ) ;
#36007 = DIRECTION ( 'NONE',  ( -1.000000000000000000, 0.000000000000000000, 0.000000000000000000 ) ) ;
#36008 = CIRCLE ( 'NONE', #28225, 1.000000000000000000 ) ;
#36009 = CARTESIAN_POINT ( 'NONE',  ( 2.866343458708493497, 21.79950405809651315, -24.26554964526188840 ) ) ;
#36010 = DIRECTION ( 'NONE',  ( -0.000000000000000000, -0.000000000000000000, -1.000000000000000000 ) ) ;
#36011 = CARTESIAN_POINT ( 'NONE',  ( 23.05386822411319159, -7.747535282638377652, 21.00000000000000000 ) ) ;
#36012 = CARTESIAN_POINT ( 'NONE',  ( 16.47321826383852184, -22.95941082514774578, -15.14534849247683646 ) ) ;
#36013 = CARTESIAN_POINT ( 'NONE',  ( -5.440908595777636414, 35.94977745735568675, 7.000000000000000000 ) ) ;
#36014 = VECTOR ( 'NONE', #4577, 999.9999999999998863 ) ;
#36015 = CARTESIAN_POINT ( 'NONE',  ( -13.13451774850164355, 16.06441397984658792, 10.49999999999999822 ) ) ;
#36016 = LINE ( 'NONE', #3970, #7726 ) ;
#36017 = ORIENTED_EDGE ( 'NONE', *, *, #25880, .T. ) ;
#36018 = CARTESIAN_POINT ( 'NONE',  ( 15.19538877031547308, 26.53216222070651398, -7.823603041336555819 ) ) ;
#36019 = VERTEX_POINT ( 'NONE', #15078 ) ;
#36020 = AXIS2_PLACEMENT_3D ( 'NONE', #1988, #38950, #29204 ) ;
#36021 = CARTESIAN_POINT ( 'NONE',  ( -13.18473458846506396, 21.24086736371716455, -17.47963371193705129 ) ) ;
#36022 = CARTESIAN_POINT ( 'NONE',  ( -31.21198460772095018, -5.568619476415831215, 18.87996532025784902 ) ) ;
#36023 = CARTESIAN_POINT ( 'NONE',  ( -14.09933648065463707, 26.02968990214174028, 10.49999999999999822 ) ) ;
#36024 = CARTESIAN_POINT ( 'NONE',  ( 13.26563377173174096, 22.13583170298742075, -16.45275615339405206 ) ) ;
#36025 = ORIENTED_EDGE ( 'NONE', *, *, #15393, .F. ) ;
#36026 = CARTESIAN_POINT ( 'NONE',  ( 17.65215317207318080, -10.44170805849464401, -30.00000000000002842 ) ) ;
#36027 = ORIENTED_EDGE ( 'NONE', *, *, #4886, .F. ) ;
#36029 = CARTESIAN_POINT ( 'NONE',  ( -12.99377146717201015, 26.19620116591435632, 9.500000000000000000 ) ) ;
#36028 = CARTESIAN_POINT ( 'NONE',  ( -10.79848222091381871, 17.83570280373058026, -26.79973138845655711 ) ) ;
#36030 = CARTESIAN_POINT ( 'NONE',  ( -18.36895873238599108, -27.24750037505589262, -4.999999999999997335 ) ) ;
#36031 = DIRECTION ( 'NONE',  ( -0.000000000000000000, -0.000000000000000000, -1.000000000000000000 ) ) ;
#36032 = ORIENTED_EDGE ( 'NONE', *, *, #15705, .T. ) ;
#36033 = CARTESIAN_POINT ( 'NONE',  ( -20.73329258327116875, -7.162834230695762194, -24.32145964058944188 ) ) ;
#36034 = CARTESIAN_POINT ( 'NONE',  ( -14.77796826032629696, -26.49119245572812531, -6.417790910078942090 ) ) ;
#36035 = DIRECTION ( 'NONE',  ( 0.000000000000000000, 0.000000000000000000, 1.000000000000000000 ) ) ;
#36036 = ORIENTED_EDGE ( 'NONE', *, *, #20915, .T. ) ;
#36037 = CARTESIAN_POINT ( 'NONE',  ( 22.21443852417969111, 2.286644819169600051, -21.81262643821637681 ) ) ;
#36038 = CARTESIAN_POINT ( 'NONE',  ( -13.63581098909220479, 27.45627467658446008, 7.000000000000000000 ) ) ;
#36039 = CARTESIAN_POINT ( 'NONE',  ( -33.75875814100331951, 2.759858869446534246, 11.00000000000000000 ) ) ;
#36040 = ORIENTED_EDGE ( 'NONE', *, *, #38359, .F. ) ;
#36041 = CARTESIAN_POINT ( 'NONE',  ( -20.97617324094073510, 0.7433129137733408554, -26.21918480705897991 ) ) ;
#36042 = CIRCLE ( 'NONE', #18518, 1.000000000000003553 ) ;
#36043 = CARTESIAN_POINT ( 'NONE',  ( 20.49959133494802543, 0.2219702378425635336, -30.00000000000000000 ) ) ;
#36044 = CARTESIAN_POINT ( 'NONE',  ( 19.02196449790080024, -24.34812345384549914, 18.87996532025784546 ) ) ;
#36045 = ORIENTED_EDGE ( 'NONE', *, *, #8115, .T. ) ;
#36046 = CARTESIAN_POINT ( 'NONE',  ( -29.21107446086027082, 1.733986180571662095, -5.000000000000000000 ) ) ;
#36047 = CIRCLE ( 'NONE', #25639, 1.000000000000000888 ) ;
#36048 = CARTESIAN_POINT ( 'NONE',  ( -21.88444403592365362, 6.126538576424530369, -21.50719306941233455 ) ) ;
#36049 = DIRECTION ( 'NONE',  ( 1.000000000000000000, 0.000000000000000000, 0.000000000000000000 ) ) ;
#36050 = AXIS2_PLACEMENT_3D ( 'NONE', #37499, #22050, #31397 ) ;
#36051 = VECTOR ( 'NONE', #8136, 1000.000000000000000 ) ;
#36052 = CARTESIAN_POINT ( 'NONE',  ( -18.23649648353780961, -16.09146789626143814, 20.99999999999999645 ) ) ;
#36053 = CARTESIAN_POINT ( 'NONE',  ( -10.44103466624267185, 32.57396620494226624, 9.000000000000001776 ) ) ;
#36054 = DIRECTION ( 'NONE',  ( 0.000000000000000000, 0.000000000000000000, -1.000000000000000000 ) ) ;
#36055 = DIRECTION ( 'NONE',  ( -0.9945218953682745111, -0.1045284632676425907, 0.000000000000000000 ) ) ;
#36056 = EDGE_LOOP ( 'NONE', ( #30924, #27381, #34381, #837, #1430 ) ) ;
#36057 = CARTESIAN_POINT ( 'NONE',  ( -25.41367398360687346, 5.264759306010887485, -10.30541271499615164 ) ) ;
#36058 = DIRECTION ( 'NONE',  ( 0.000000000000000000, 0.000000000000000000, 1.000000000000000000 ) ) ;
#36059 = CARTESIAN_POINT ( 'NONE',  ( 3.914034194965611668, 30.06176806842419680, 9.000000000000001776 ) ) ;
#36060 = CARTESIAN_POINT ( 'NONE',  ( 24.21332198295975502, -23.75827105196518474, -11.15521848907045666 ) ) ;
#36061 = DIRECTION ( 'NONE',  ( 0.000000000000000000, 0.000000000000000000, 1.000000000000000000 ) ) ;
#36062 = CARTESIAN_POINT ( 'NONE',  ( 14.48927117870126757, -30.61587158504672246, 23.00000000000000355 ) ) ;
#36063 = CARTESIAN_POINT ( 'NONE',  ( 10.79245250836826564, 17.68824287289717034, -27.42597519482002610 ) ) ;
#36064 = CARTESIAN_POINT ( 'NONE',  ( 5.067385705950949948, -26.57793081542402547, 12.73282698324853257 ) ) ;
#36065 = ORIENTED_EDGE ( 'NONE', *, *, #32764, .F. ) ;
#36066 = CARTESIAN_POINT ( 'NONE',  ( -13.63746324345819261, 16.03261875762171584, -25.28435114513372284 ) ) ;
#36067 = CARTESIAN_POINT ( 'NONE',  ( -24.44578022397290695, -10.62045233751050866, 20.99999999999999645 ) ) ;
#36068 = EDGE_CURVE ( 'NONE', #490, #27538, #32458, .T. ) ;
#36069 = LINE ( 'NONE', #20434, #30193 ) ;
#36070 = CARTESIAN_POINT ( 'NONE',  ( 12.14281235004362358, 19.90984008834854890, -20.54315895355848554 ) ) ;
#36071 = ORIENTED_EDGE ( 'NONE', *, *, #20103, .T. ) ;
#36072 = CARTESIAN_POINT ( 'NONE',  ( 12.39413036303999149, 20.48625930257307104, -19.49701620399659419 ) ) ;
#36073 = ORIENTED_EDGE ( 'NONE', *, *, #29990, .F. ) ;
#36074 = VECTOR ( 'NONE', #28866, 1000.000000000000000 ) ;
#36076 = CARTESIAN_POINT ( 'NONE',  ( -9.997483185316569987, 21.95197631500770896, 10.49999999999999467 ) ) ;
#36075 = CARTESIAN_POINT ( 'NONE',  ( -15.11182017094948016, 26.49105686739811460, -8.289746988309037334 ) ) ;
#36077 = CARTESIAN_POINT ( 'NONE',  ( -9.506566060136700358, -18.16246691004805314, -30.00000000000000000 ) ) ;
#36078 = CARTESIAN_POINT ( 'NONE',  ( -37.09709568333393293, -7.051483854460517620, 11.55979286843891529 ) ) ;
#36079 = AXIS2_PLACEMENT_3D ( 'NONE', #3192, #21868, #19025 ) ;
#36080 = CARTESIAN_POINT ( 'NONE',  ( -31.33135991916500984, -16.39895654298046423, -11.06949826535703352 ) ) ;
#36081 = CARTESIAN_POINT ( 'NONE',  ( -8.170773189261824498, -23.31984667172876868, -14.74591960211686725 ) ) ;
#36082 = CARTESIAN_POINT ( 'NONE',  ( 5.027400250556079975, 36.23526740290145653, 10.49999999999999822 ) ) ;
#36083 = CARTESIAN_POINT ( 'NONE',  ( 15.93428740759538265, 25.01899822204553203, -5.474102051487178322 ) ) ;
#36084 = EDGE_CURVE ( 'NONE', #32234, #26241, #26993, .T. ) ;
#36085 = ORIENTED_EDGE ( 'NONE', *, *, #18262, .F. ) ;
#36086 = CARTESIAN_POINT ( 'NONE',  ( 19.41880252833811227, 6.610239277501288591, -29.41827274932495584 ) ) ;
#36087 = CIRCLE ( 'NONE', #18563, 1.000000000000000888 ) ;
#36088 = CARTESIAN_POINT ( 'NONE',  ( 6.282361020112163352, 14.70372268239673375, 10.50000000000000000 ) ) ;
#36089 = DIRECTION ( 'NONE',  ( -1.000000000000000000, 0.000000000000000000, 0.000000000000000000 ) ) ;
#36090 = EDGE_CURVE ( 'NONE', #22206, #37186, #37215, .T. ) ;
#36091 = FACE_OUTER_BOUND ( 'NONE', #19580, .T. ) ;
#36092 = EDGE_LOOP ( 'NONE', ( #21502, #23476, #14231, #9360, #14564 ) ) ;
#36093 = CARTESIAN_POINT ( 'NONE',  ( -32.26688085667248629, -1.675871053962237012, -5.926420720323367419 ) ) ;
#36094 = CARTESIAN_POINT ( 'NONE',  ( 20.82064840824700624, 0.7693617283651914551, -26.82585393716254529 ) ) ;
#36095 = CARTESIAN_POINT ( 'NONE',  ( 14.47283171447379146, 21.48159823030311344, 7.000000000000000000 ) ) ;
#36096 = CARTESIAN_POINT ( 'NONE',  ( 25.30804003627885024, -11.14301119665278783, 20.99999999999999645 ) ) ;
#36097 = DIRECTION ( 'NONE',  ( -0.1045284632676437703, 0.9945218953682745111, 0.000000000000000000 ) ) ;
#36098 = DIRECTION ( 'NONE',  ( -0.000000000000000000, -0.000000000000000000, 1.000000000000000000 ) ) ;
#36099 = LINE ( 'NONE', #14760, #10296 ) ;
#36100 = EDGE_CURVE ( 'NONE', #20514, #7288, #40051, .T. ) ;
#36101 = EDGE_LOOP ( 'NONE', ( #19944, #39817, #1063, #24595 ) ) ;
#36102 = EDGE_CURVE ( 'NONE', #35323, #4132, #36618, .T. ) ;
#36103 = DIRECTION ( 'NONE',  ( -0.000000000000000000, -0.000000000000000000, -1.000000000000000000 ) ) ;
#36104 = VECTOR ( 'NONE', #36175, 1000.000000000000114 ) ;
#36105 = AXIS2_PLACEMENT_3D ( 'NONE', #27128, #11493, #32837 ) ;
#36106 = CARTESIAN_POINT ( 'NONE',  ( -5.330077540933487512, 17.71145523154927659, 6.000000000000000000 ) ) ;
#36107 = ORIENTED_EDGE ( 'NONE', *, *, #22736, .F. ) ;
#36108 = CARTESIAN_POINT ( 'NONE',  ( 0.4084515277692671864, 38.10027764858106281, -7.117403505773802763 ) ) ;
#36109 = CARTESIAN_POINT ( 'NONE',  ( -8.183247089818959097, 16.78440424842446532, 12.00000000000000000 ) ) ;
#36110 = VECTOR ( 'NONE', #35023, 1000.000000000000000 ) ;
#36111 = DIRECTION ( 'NONE',  ( -0.000000000000000000, -0.000000000000000000, -1.000000000000000000 ) ) ;
#36112 = CARTESIAN_POINT ( 'NONE',  ( 4.003810537522394242, 8.420815593655317954, 10.49999999999999822 ) ) ;
#36113 = DIRECTION ( 'NONE',  ( -1.000000000000000000, 0.000000000000000000, 0.000000000000000000 ) ) ;
#36114 = DIRECTION ( 'NONE',  ( 1.000000000000000000, 0.000000000000000000, 0.000000000000000000 ) ) ;
#36115 = CARTESIAN_POINT ( 'NONE',  ( 14.46172013027408632, 28.25976373080003867, -8.225629111251091530 ) ) ;
#36116 = CARTESIAN_POINT ( 'NONE',  ( -32.33143948542088708, 1.358872982498823268, -5.000000000000000888 ) ) ;
#36117 = ORIENTED_EDGE ( 'NONE', *, *, #9131, .F. ) ;
#36119 = CARTESIAN_POINT ( 'NONE',  ( 0.8712018466506370462, 31.30332840660451765, 13.00000000000000178 ) ) ;
#36118 = CARTESIAN_POINT ( 'NONE',  ( -16.41392363336672844, 12.39559230606829487, -28.28840681818169145 ) ) ;
#36120 = CARTESIAN_POINT ( 'NONE',  ( -19.26948696230207858, 27.85601271560029701, 3.000000000000000000 ) ) ;
#36121 = CARTESIAN_POINT ( 'NONE',  ( 15.45930891439913601, -26.66055752704448523, -6.416469317147711848 ) ) ;
#36122 = DIRECTION ( 'NONE',  ( -1.000000000000000000, 0.000000000000000000, 0.000000000000000000 ) ) ;
#36123 = CARTESIAN_POINT ( 'NONE',  ( 15.22307974005524223, 26.43793140921028240, -7.826725321211265296 ) ) ;
#36124 = DIRECTION ( 'NONE',  ( -0.9781476007338041345, 0.2079116908177663092, 0.000000000000000000 ) ) ;
#36125 = ADVANCED_FACE ( 'NONE', ( #15676 ), #2856, .T. ) ;
#36126 = DIRECTION ( 'NONE',  ( 1.000000000000000000, 0.000000000000000000, 0.000000000000000000 ) ) ;
#36127 = CARTESIAN_POINT ( 'NONE',  ( -25.79871209414094935, -22.89210493903414090, -11.11974611591713291 ) ) ;
#36128 = CARTESIAN_POINT ( 'NONE',  ( 1.767497973323724381, -24.39642072439984943, -9.396636978634532511 ) ) ;
#36129 = CARTESIAN_POINT ( 'NONE',  ( 15.52046154931812261, 26.41174381453696540, -5.000000000000000888 ) ) ;
#36130 = CARTESIAN_POINT ( 'NONE',  ( 18.90886957614733177, 10.57106918749075319, -21.18213341435799180 ) ) ;
#36131 = CARTESIAN_POINT ( 'NONE',  ( -6.064571727552472424, 31.45661825943146894, 6.000000000000000000 ) ) ;
#36132 = ORIENTED_EDGE ( 'NONE', *, *, #1183, .F. ) ;
#36133 = CARTESIAN_POINT ( 'NONE',  ( -5.270476743073104764, 25.91271121330065696, -18.72494855390057467 ) ) ;
#36134 = VERTEX_POINT ( 'NONE', #24621 ) ;
#36135 = VECTOR ( 'NONE', #33054, 1000.000000000000114 ) ;
#36136 = VECTOR ( 'NONE', #7075, 1000.000000000000000 ) ;
#36137 = CARTESIAN_POINT ( 'NONE',  ( 5.204598533297671636, 36.56827286999722304, 7.339470489435498735 ) ) ;
#36138 = VERTEX_POINT ( 'NONE', #18140 ) ;
#36139 = DIRECTION ( 'NONE',  ( 0.1470157664651934870, -0.6916548014802242905, -0.7071067811865497932 ) ) ;
#36140 = CARTESIAN_POINT ( 'NONE',  ( 19.15807744002891155, 8.842452143891316396, 7.500000000000000000 ) ) ;
#36141 = VERTEX_POINT ( 'NONE', #3284 ) ;
#36142 = CARTESIAN_POINT ( 'NONE',  ( -20.95633139473599726, 0.9343472425770981138, -26.23583468170135546 ) ) ;
#36143 = ORIENTED_EDGE ( 'NONE', *, *, #7253, .F. ) ;
#36144 = CARTESIAN_POINT ( 'NONE',  ( 24.22071271199023101, -7.313483937193986151, -19.78735341019923055 ) ) ;
#36145 = ORIENTED_EDGE ( 'NONE', *, *, #19562, .T. ) ;
#36146 = CARTESIAN_POINT ( 'NONE',  ( -11.44134295108998955, 15.31698729810788961, 9.500000000000000000 ) ) ;
#36147 = ORIENTED_EDGE ( 'NONE', *, *, #8513, .T. ) ;
#36148 = ADVANCED_FACE ( 'NONE', ( #30530 ), #34170, .F. ) ;
#36149 = FACE_OUTER_BOUND ( 'NONE', #37671, .T. ) ;
#36150 = CARTESIAN_POINT ( 'NONE',  ( -5.348113209407908464, 9.835177808069893501, 13.00000000000000178 ) ) ;
#36151 = CARTESIAN_POINT ( 'NONE',  ( 0.4999999999999990563, 31.00000000000000355, 7.000000000000000000 ) ) ;
#36152 = ORIENTED_EDGE ( 'NONE', *, *, #6591, .F. ) ;
#36153 = SURFACE_SIDE_STYLE ('',( #36549 ) ) ;
#36154 = DIRECTION ( 'NONE',  ( 0.000000000000000000, 0.000000000000000000, 1.000000000000000000 ) ) ;
#36155 = CARTESIAN_POINT ( 'NONE',  ( -2.552861293176900137, 8.084864722426296169, 10.99999999999999822 ) ) ;
#36156 = CARTESIAN_POINT ( 'NONE',  ( 11.70245575391219006, 4.690003899809237708, 9.500000000000000000 ) ) ;
#36157 = CARTESIAN_POINT ( 'NONE',  ( 16.76787866856672338, 15.62184907137590706, -17.91620485821478326 ) ) ;
#36158 = AXIS2_PLACEMENT_3D ( 'NONE', #8406, #20803, #33405 ) ;
#36159 = CARTESIAN_POINT ( 'NONE',  ( 6.908205946113893603, 19.31174812457788548, -29.26867246192825078 ) ) ;
#36160 = VECTOR ( 'NONE', #27782, 1000.000000000000000 ) ;
#36161 = ORIENTED_EDGE ( 'NONE', *, *, #35340, .T. ) ;
#36162 = CARTESIAN_POINT ( 'NONE',  ( -22.16749550643533340, 10.73470648441587905, -8.406596372856219190 ) ) ;
#36163 = DIRECTION ( 'NONE',  ( 1.000000000000000000, 0.000000000000000000, 0.000000000000000000 ) ) ;
#36164 = FACE_OUTER_BOUND ( 'NONE', #37769, .T. ) ;
#36165 = CARTESIAN_POINT ( 'NONE',  ( 13.94326871252339473, -24.14806653283149629, -13.49309882371043834 ) ) ;
#36166 = CARTESIAN_POINT ( 'NONE',  ( 37.48538792151179422, -11.24999995791135809, -5.000000000000002665 ) ) ;
#36167 = CIRCLE ( 'NONE', #8937, 1.000000000000004441 ) ;
#36168 = CARTESIAN_POINT ( 'NONE',  ( -14.47283171447380035, 21.48159823030330884, 7.500000000000004441 ) ) ;
#36169 = EDGE_CURVE ( 'NONE', #14281, #16948, #12426, .T. ) ;
#36170 = CIRCLE ( 'NONE', #14096, 0.5000000000000004441 ) ;
#36171 = CARTESIAN_POINT ( 'NONE',  ( -13.20806276164241488, 22.23819342938818622, -16.44376970385624759 ) ) ;
#36172 = CARTESIAN_POINT ( 'NONE',  ( -36.73707435953562594, -10.93158220173930673, 14.53008259254087875 ) ) ;
#36173 = CARTESIAN_POINT ( 'NONE',  ( 13.64569075595249181, -26.22458777178208322, -6.419671810663616363 ) ) ;
#36174 = EDGE_CURVE ( 'NONE', #6531, #27384, #24023, .T. ) ;
#36175 = DIRECTION ( 'NONE',  ( 0.6691306063588570163, -0.7431448254773952433, 0.000000000000000000 ) ) ;
#36176 = ORIENTED_EDGE ( 'NONE', *, *, #21242, .T. ) ;
#36177 = ORIENTED_EDGE ( 'NONE', *, *, #8661, .F. ) ;
#36178 = CARTESIAN_POINT ( 'NONE',  ( -12.21035293360103147, 31.03120155201804309, -9.465151556475316141 ) ) ;
#36179 = DIRECTION ( 'NONE',  ( -0.7431448254773850293, 0.6691306063588685626, 0.000000000000000000 ) ) ;
#36180 = DIRECTION ( 'NONE',  ( 0.3090169943749572767, 0.9510565162951503115, -0.000000000000000000 ) ) ;
#36181 = EDGE_CURVE ( 'NONE', #19810, #9924, #38002, .T. ) ;
#36182 = DIRECTION ( 'NONE',  ( -0.4999999999999921174, 0.8660254037844431485, 0.000000000000000000 ) ) ;
#36183 = VERTEX_POINT ( 'NONE', #242 ) ;
#36184 = CARTESIAN_POINT ( 'NONE',  ( 30.65966444727390794, 0.03748699155148955270, -6.888076747643670394 ) ) ;
#36185 = CARTESIAN_POINT ( 'NONE',  ( -5.400683141673551013, 15.91724817395922997, 7.000000000000000000 ) ) ;
#36186 = DIRECTION ( 'NONE',  ( -0.8660254037844431485, -0.4999999999999921174, 0.000000000000000000 ) ) ;
#36187 = CARTESIAN_POINT ( 'NONE',  ( -20.41099665934841312, -29.27811314928202080, 11.00000000000014211 ) ) ;
#36188 = ORIENTED_EDGE ( 'NONE', *, *, #15267, .T. ) ;
#36189 = CARTESIAN_POINT ( 'NONE',  ( -29.97333235930364381, 0.04935946867576600922, -9.238760947532812295 ) ) ;
#36190 = ADVANCED_BREP_SHAPE_REPRESENTATION ( '', ( #8155, #24238 ), #11913 ) ;
#36191 = CARTESIAN_POINT ( 'NONE',  ( 14.09933648065468503, 26.02968990214155198, 7.500000000000000888 ) ) ;
#36192 = ORIENTED_EDGE ( 'NONE', *, *, #29090, .F. ) ;
#36193 = CARTESIAN_POINT ( 'NONE',  ( 21.43667605784225572, -3.053840757090042324, -24.61930641589043489 ) ) ;
#36194 = TOROIDAL_SURFACE ( 'NONE', #22568, 1.000000000000000000, 0.5000000000000000000 ) ;
#36195 = AXIS2_PLACEMENT_3D ( 'NONE', #15544, #28324, #33843 ) ;
#36196 = CARTESIAN_POINT ( 'NONE',  ( 36.05338440271408018, -10.94427667939843651, 15.72805884748937011 ) ) ;
#36197 = ORIENTED_EDGE ( 'NONE', *, *, #9993, .T. ) ;
#36198 = CARTESIAN_POINT ( 'NONE',  ( 7.360725290688645117, 38.43561981343065526, 13.92931973827796632 ) ) ;
#36199 = EDGE_CURVE ( 'NONE', #15690, #17187, #8163, .T. ) ;
#36200 = AXIS2_PLACEMENT_3D ( 'NONE', #30604, #12898, #30994 ) ;
#36201 = CARTESIAN_POINT ( 'NONE',  ( 15.48695972778119945, -26.74878859331994718, 16.30093088680190405 ) ) ;
#36202 = ADVANCED_FACE ( 'NONE', ( #12627 ), #4078, .F. ) ;
#36203 = LINE ( 'NONE', #29894, #39011 ) ;
#36204 = EDGE_CURVE ( 'NONE', #37355, #27267, #9785, .T. ) ;
#36205 = CARTESIAN_POINT ( 'NONE',  ( -1.610977985363139187, 29.80447555512211011, 20.82122704794079482 ) ) ;
#36206 = VECTOR ( 'NONE', #24684, 1000.000000000000000 ) ;
#36207 = DIRECTION ( 'NONE',  ( -0.000000000000000000, -0.000000000000000000, -1.000000000000000000 ) ) ;
#36208 = ORIENTED_EDGE ( 'NONE', *, *, #24142, .T. ) ;
#36209 = CARTESIAN_POINT ( 'NONE',  ( -7.766013557953293400, 28.81973365084998306, 10.49999999999999822 ) ) ;
#36210 = CARTESIAN_POINT ( 'NONE',  ( -13.48130249190472796, 27.93180293473203690, 11.00000000000000000 ) ) ;
#36211 = CARTESIAN_POINT ( 'NONE',  ( 3.933113624042559930, 20.35544397462496846, -27.75572121666948178 ) ) ;
#36212 = CARTESIAN_POINT ( 'NONE',  ( -8.118377661053489902, 10.47536095541709322, 7.500000000000000888 ) ) ;
#36213 = CARTESIAN_POINT ( 'NONE',  ( 28.25018339771033027, -2.647087534805522946, 19.27171037444156454 ) ) ;
#36214 = CARTESIAN_POINT ( 'NONE',  ( 14.50103858733138829, -20.35908921518062087, -19.15145559871423941 ) ) ;
#36215 = CARTESIAN_POINT ( 'NONE',  ( 1.947644445291253357, 40.50000000000005684, 11.00000000000000178 ) ) ;
#36216 = DIRECTION ( 'NONE',  ( 0.9135454576426005335, -0.4067366430758008744, 0.000000000000000000 ) ) ;
#36217 = CARTESIAN_POINT ( 'NONE',  ( -3.813962023474485541, 32.29559562678526419, 11.00000000000000000 ) ) ;
#36218 = EDGE_LOOP ( 'NONE', ( #7506, #32489, #720, #11869 ) ) ;
#36219 = EDGE_CURVE ( 'NONE', #36670, #20763, #19123, .T. ) ;
#36220 = CARTESIAN_POINT ( 'NONE',  ( 11.39842292676588720, 18.51123022929508721, -23.84032446260234295 ) ) ;
#36221 = VECTOR ( 'NONE', #35084, 1000.000000000000000 ) ;
#36223 = VERTEX_POINT ( 'NONE', #15879 ) ;
#36222 = EDGE_CURVE ( 'NONE', #6988, #37631, #22358, .T. ) ;
#36224 = CARTESIAN_POINT ( 'NONE',  ( -11.34469411494776203, 17.22161296595826485, -28.09528742440320670 ) ) ;
#36225 = CARTESIAN_POINT ( 'NONE',  ( -31.19396690150113471, -3.926129315323696467, 18.42518152272069898 ) ) ;
#36226 = ADVANCED_FACE ( 'NONE', ( #19727 ), #25218, .T. ) ;
#36227 = CARTESIAN_POINT ( 'NONE',  ( -2.199596516246109523, 8.143600047011682719, 10.66666666666666607 ) ) ;
#36228 = CARTESIAN_POINT ( 'NONE',  ( 15.42070031560629317, 26.50090741082905055, -6.417193677922045758 ) ) ;
#36229 = VERTEX_POINT ( 'NONE', #22763 ) ;
#36230 = CARTESIAN_POINT ( 'NONE',  ( 18.12106542394759501, -11.46725993656733777, -25.57869145427667945 ) ) ;
#36231 = ORIENTED_EDGE ( 'NONE', *, *, #5088, .F. ) ;
#36232 = AXIS2_PLACEMENT_3D ( 'NONE', #15304, #27691, #39689 ) ;
#36234 = CARTESIAN_POINT ( 'NONE',  ( -32.33143948541789570, 1.358872982501806215, -5.000000000000000000 ) ) ;
#36233 = CARTESIAN_POINT ( 'NONE',  ( -13.50527592257643050, 23.96582696250451860, -14.41748651284650151 ) ) ;
#36235 = CARTESIAN_POINT ( 'NONE',  ( -10.71436039581699795, -17.92443767809337629, -26.74123038190443324 ) ) ;
#36236 = LINE ( 'NONE', #27281, #14644 ) ;
#36237 = VECTOR ( 'NONE', #38577, 1000.000000000000114 ) ;
#36238 = ORIENTED_EDGE ( 'NONE', *, *, #10628, .T. ) ;
#36239 = ADVANCED_FACE ( 'NONE', ( #13217 ), #9585, .F. ) ;
#36240 = CARTESIAN_POINT ( 'NONE',  ( -27.04735894903886972, -9.297324301607403640, -16.71430700021294413 ) ) ;
#36241 = CARTESIAN_POINT ( 'NONE',  ( -14.28239120255770622, -25.56022528091948587, -10.18897211997865782 ) ) ;
#36242 = DIRECTION ( 'NONE',  ( -0.000000000000000000, -0.000000000000000000, -1.000000000000000000 ) ) ;
#36243 = EDGE_LOOP ( 'NONE', ( #3020, #12870, #805 ) ) ;
#36244 = CARTESIAN_POINT ( 'NONE',  ( 20.40557468639088157, 2.415499751543392914, -28.75714396012276097 ) ) ;
#36245 = CARTESIAN_POINT ( 'NONE',  ( -7.741055489194995864, 10.14404956260399615, 10.49999999999999822 ) ) ;
#36246 = FACE_OUTER_BOUND ( 'NONE', #38340, .T. ) ;
#36247 = ORIENTED_EDGE ( 'NONE', *, *, #37458, .F. ) ;
#36248 = CARTESIAN_POINT ( 'NONE',  ( -29.65891584835985384, -0.01954106857342741491, -10.17503558318995083 ) ) ;
#36249 = CARTESIAN_POINT ( 'NONE',  ( 31.65879457089920024, -0.9929091283696672710, -6.398057018500724169 ) ) ;
#36250 = CARTESIAN_POINT ( 'NONE',  ( 31.78757023779201774, -12.37085478034622454, 19.27171037444154678 ) ) ;
#36251 = VERTEX_POINT ( 'NONE', #3483 ) ;
#36252 = CARTESIAN_POINT ( 'NONE',  ( -20.74417435968310031, 3.585152392585164272, -25.26646650636820013 ) ) ;
#36253 = LINE ( 'NONE', #37040, #30059 ) ;
#36254 = EDGE_CURVE ( 'NONE', #21244, #27921, #15944, .T. ) ;
#36255 = DIRECTION ( 'NONE',  ( 0.1045284632676437703, -0.9945218953682745111, -0.000000000000000000 ) ) ;
#36256 = AXIS2_PLACEMENT_3D ( 'NONE', #13566, #22906, #4018 ) ;
#36257 = CARTESIAN_POINT ( 'NONE',  ( -37.37248716976025520, -8.922526051835991012, 10.99999999999990941 ) ) ;
#36258 = VECTOR ( 'NONE', #39492, 1000.000000000000000 ) ;
#36259 = CARTESIAN_POINT ( 'NONE',  ( -2.165907168841142205, 7.657055764658191599, 7.339470489435488965 ) ) ;
#36260 = CARTESIAN_POINT ( 'NONE',  ( 6.535904741238498517, 35.95058573176943639, 10.76099332938163755 ) ) ;
#36261 = DIRECTION ( 'NONE',  ( 0.000000000000000000, 0.000000000000000000, 1.000000000000000000 ) ) ;
#36262 = EDGE_LOOP ( 'NONE', ( #33342, #1868, #30088 ) ) ;
#36263 = CARTESIAN_POINT ( 'NONE',  ( -19.89457789833269885, 5.001894110080484346, -29.40556248342900147 ) ) ;
#36264 = DIRECTION ( 'NONE',  ( 0.6691306063588671194, 0.7431448254773861395, 0.000000000000000000 ) ) ;
#36265 = CARTESIAN_POINT ( 'NONE',  ( 8.007761790012084546, 9.776959832083274904, 11.00000000000000000 ) ) ;
#36266 = CARTESIAN_POINT ( 'NONE',  ( 21.45659587343440222, -22.35059298105742798, -13.95210435312599273 ) ) ;
#36267 = CYLINDRICAL_SURFACE ( 'NONE', #18390, 0.5000000000000004441 ) ;
#36268 = CARTESIAN_POINT ( 'NONE',  ( -14.36203778474861181, 19.98498072221388000, 10.49999999999999822 ) ) ;
#36269 = CARTESIAN_POINT ( 'NONE',  ( 14.72331344930747932, 25.96238726373383088, -10.15914416928072050 ) ) ;
#36270 = CARTESIAN_POINT ( 'NONE',  ( 10.15481549915635640, -27.08512292515340647, 13.32518128616567310 ) ) ;
#36271 = ORIENTED_EDGE ( 'NONE', *, *, #24947, .F. ) ;
#36272 = CARTESIAN_POINT ( 'NONE',  ( -14.74746392996318356, 18.03178186202489641, -18.77012448782567944 ) ) ;
#36273 = CARTESIAN_POINT ( 'NONE',  ( -23.79772124597074523, -17.36195373897575678, 20.82122704794079482 ) ) ;
#36274 = EDGE_CURVE ( 'NONE', #4798, #24101, #29596, .T. ) ;
#36275 = DIRECTION ( 'NONE',  ( 1.000000000000000000, 0.000000000000000000, 0.000000000000000000 ) ) ;
#36276 = CARTESIAN_POINT ( 'NONE',  ( 15.30701244550224338, 26.47243815946491452, -7.358024508618584036 ) ) ;
#36277 = EDGE_LOOP ( 'NONE', ( #26650, #35977 ) ) ;
#36278 = DIRECTION ( 'NONE',  ( 0.8090169943749503378, 0.5877852522924691403, 0.000000000000000000 ) ) ;
#36279 = ORIENTED_EDGE ( 'NONE', *, *, #18557, .F. ) ;
#36281 = CARTESIAN_POINT ( 'NONE',  ( -2.853172919594720192, 21.57294901687549427, 6.000000000000000000 ) ) ;
#36280 = CARTESIAN_POINT ( 'NONE',  ( -14.67353854144589675, 25.58823882037592412, -10.64067760867671808 ) ) ;
#36282 = CARTESIAN_POINT ( 'NONE',  ( -15.51079060825593281, -26.67363690140799903, -6.415640535509750997 ) ) ;
#36283 = CARTESIAN_POINT ( 'NONE',  ( -18.84564290660895836, -29.34375446593489656, 11.00000000000029132 ) ) ;
#36284 = CIRCLE ( 'NONE', #12826, 16.00000000000000000 ) ;
#36285 = CIRCLE ( 'NONE', #31083, 0.5000000000000004441 ) ;
#36286 = CARTESIAN_POINT ( 'NONE',  ( -30.51621992633454639, -15.97226344309796886, -11.97627014025983705 ) ) ;
#36287 = CARTESIAN_POINT ( 'NONE',  ( -7.977729298563027704, -22.95874574334327889, -15.75516193211872640 ) ) ;
#36288 = CARTESIAN_POINT ( 'NONE',  ( 12.93365880273942281, 18.25915373805785791, -21.78730442601257167 ) ) ;
#36289 = EDGE_LOOP ( 'NONE', ( #16905, #7674 ) ) ;
#36290 = CARTESIAN_POINT ( 'NONE',  ( 20.83270517224113760, 6.805427843616754124, -21.08448443926039317 ) ) ;
#36291 = DIRECTION ( 'NONE',  ( 1.000000000000000000, 0.000000000000000000, 0.000000000000000000 ) ) ;
#36292 = CARTESIAN_POINT ( 'NONE',  ( 6.471564538981485981, 17.88766432731502931, 23.00000000000000355 ) ) ;
#36293 = DIRECTION ( 'NONE',  ( 1.000000000000000000, 0.000000000000000000, 0.000000000000000000 ) ) ;
#36294 = VECTOR ( 'NONE', #16304, 1000.000000000000000 ) ;
#36295 = EDGE_LOOP ( 'NONE', ( #17157, #16436, #1918, #3777 ) ) ;
#36296 = CARTESIAN_POINT ( 'NONE',  ( -23.01684666815623714, -0.4182225803685448717, -21.47969933400415954 ) ) ;
#36297 = CARTESIAN_POINT ( 'NONE',  ( 30.96479225765983045, -0.1042645752839200801, -5.473789633946161359 ) ) ;
#36298 = DIRECTION ( 'NONE',  ( 0.9945218953682730678, -0.1045284632676564962, 0.000000000000000000 ) ) ;
#36299 = CARTESIAN_POINT ( 'NONE',  ( 21.62094419769710285, -18.41873747673067641, 20.82122704794092627 ) ) ;
#36300 = DIRECTION ( 'NONE',  ( 0.000000000000000000, 0.000000000000000000, 1.000000000000000000 ) ) ;
#36301 = CARTESIAN_POINT ( 'NONE',  ( 18.07620401364302865, 24.68088026512193167, -13.58461195433497082 ) ) ;
#36302 = CARTESIAN_POINT ( 'NONE',  ( -75.15099915297791711, 43.38844959084113384, 0.000000000000000000 ) ) ;
#36303 = ADVANCED_FACE ( 'NONE', ( #443 ), #28664, .F. ) ;
#36304 = ORIENTED_EDGE ( 'NONE', *, *, #33845, .F. ) ;
#36305 = CARTESIAN_POINT ( 'NONE',  ( -8.294006203984645609, 33.46401007850805343, 13.00000000000000178 ) ) ;
#36306 = CARTESIAN_POINT ( 'NONE',  ( 6.843305518951320998, 35.42677428760913472, 10.49999999999999822 ) ) ;
#36307 = ORIENTED_EDGE ( 'NONE', *, *, #9937, .F. ) ;
#36308 = CARTESIAN_POINT ( 'NONE',  ( 1.569683897492700098, 38.21696230019209395, -6.697046784752907378 ) ) ;
#36309 = CARTESIAN_POINT ( 'NONE',  ( -6.953812613386785912, 14.77701242934787906, 12.00000000000000000 ) ) ;
#36310 = CARTESIAN_POINT ( 'NONE',  ( 14.97058623676931255, 26.66112013780996648, 16.87380292611441135 ) ) ;
#36311 = EDGE_CURVE ( 'NONE', #13704, #21433, #1713, .T. ) ;
#36312 = DIRECTION ( 'NONE',  ( -0.8090169943749505599, -0.5877852522924689183, 0.000000000000000000 ) ) ;
#36313 = CYLINDRICAL_SURFACE ( 'NONE', #11520, 1.000000000000000888 ) ;
#36314 = CARTESIAN_POINT ( 'NONE',  ( 9.356056665764066693, 26.06569820189703535, 10.00000000000000000 ) ) ;
#36315 = FACE_OUTER_BOUND ( 'NONE', #23014, .T. ) ;
#36316 = CARTESIAN_POINT ( 'NONE',  ( 14.71880540954476935, 27.90283997931214088, -7.780570891888019425 ) ) ;
#36317 = CARTESIAN_POINT ( 'NONE',  ( -10.10646936306323518, 32.94553861768095970, 7.500000000000004441 ) ) ;
#36318 = ORIENTED_EDGE ( 'NONE', *, *, #22787, .T. ) ;
#36320 = DIRECTION ( 'NONE',  ( 0.4067366430757913820, -0.9135454576426049744, -7.055756032835740798E-16 ) ) ;
#36319 = CARTESIAN_POINT ( 'NONE',  ( -18.78764273638527982, 16.18379394525580039, -10.35842720535364592 ) ) ;
#36321 = CARTESIAN_POINT ( 'NONE',  ( 9.762586613238328326, -29.39641002289260285, 10.99999999999999822 ) ) ;
#36322 = CARTESIAN_POINT ( 'NONE',  ( 10.55467174157632293, -19.57048749257938525, -22.73257509897530326 ) ) ;
#36323 = CARTESIAN_POINT ( 'NONE',  ( 12.13489577391684904, 19.91918273965267261, -20.54176214682885515 ) ) ;
#36324 = CARTESIAN_POINT ( 'NONE',  ( 15.40434907611582638, 26.82505288294843027, -5.474005114572026542 ) ) ;
#36325 = CARTESIAN_POINT ( 'NONE',  ( -3.485571585149886520, -11.25000000000002132, 10.00000000000000000 ) ) ;
#36326 = CARTESIAN_POINT ( 'NONE',  ( 5.330070799514983193, 27.28854476845134513, 12.00000000000000000 ) ) ;
#36327 = CARTESIAN_POINT ( 'NONE',  ( -20.41145111406656198, -16.99166856771202205, -18.69276795763255805 ) ) ;
#36328 = CARTESIAN_POINT ( 'NONE',  ( 3.253891525658406447, -22.11403326693343985, -19.03245994517476092 ) ) ;
#36329 = CARTESIAN_POINT ( 'NONE',  ( 11.29606703750313912, 17.49295334550439307, -26.84622463755728106 ) ) ;
#36330 = CARTESIAN_POINT ( 'NONE',  ( 18.06948145980227949, 10.11918264026371439, -26.62323384584303909 ) ) ;
#36331 = FACE_OUTER_BOUND ( 'NONE', #19902, .T. ) ;
#36332 = EDGE_CURVE ( 'NONE', #29063, #38519, #34565, .T. ) ;
#36333 = ORIENTED_EDGE ( 'NONE', *, *, #37077, .F. ) ;
#36334 = CARTESIAN_POINT ( 'NONE',  ( -4.760937472852409869, 20.33112424556681574, -27.05855014857421637 ) ) ;
#36335 = VERTEX_POINT ( 'NONE', #34370 ) ;
#36336 = AXIS2_PLACEMENT_3D ( 'NONE', #6359, #37052, #7515 ) ;
#36337 = CARTESIAN_POINT ( 'NONE',  ( -19.62624412895475245, 17.27415994119605003, 15.13084544680118704 ) ) ;
#36338 = ORIENTED_EDGE ( 'NONE', *, *, #18087, .F. ) ;
#36339 = CARTESIAN_POINT ( 'NONE',  ( -5.034171952701854025, 35.03623199971307400, 9.500000000000000000 ) ) ;
#36340 = CARTESIAN_POINT ( 'NONE',  ( 9.221287281574507944, 10.65863771052197784, 10.49999999999999822 ) ) ;
#36341 = VECTOR ( 'NONE', #1369, 1000.000000000000227 ) ;
#36342 = CARTESIAN_POINT ( 'NONE',  ( -27.00797239653981663, 0.4251854506619431873, -14.48925554260671689 ) ) ;
#36343 = B_SPLINE_CURVE_WITH_KNOTS ( 'NONE', 3,
 ( #8341, #33135, #35976, #26218, #23379, #35775 ),
 .UNSPECIFIED., .F., .F.,
 ( 4, 2, 4 ),
 ( 0.000000000000000000, 0.0002970590326188848234, 0.0005941180652377696467 ),
 .UNSPECIFIED. ) ;
#36344 = CARTESIAN_POINT ( 'NONE',  ( 26.03424934262190504, -8.709753677229443269, -17.70432680259551361 ) ) ;
#36345 = ADVANCED_FACE ( 'NONE', ( #6916 ), #19318, .T. ) ;
#36346 = EDGE_LOOP ( 'NONE', ( #11037, #22577, #17562, #19242 ) ) ;
#36347 = CARTESIAN_POINT ( 'NONE',  ( 11.44134295108989363, 15.31698729810773152, 9.500000000000000000 ) ) ;
#36348 = VERTEX_POINT ( 'NONE', #32118 ) ;
#36349 = FACE_OUTER_BOUND ( 'NONE', #31579, .T. ) ;
#36350 = LINE ( 'NONE', #8515, #1405 ) ;
#36351 = DIRECTION ( 'NONE',  ( 1.000000000000000000, 0.000000000000000000, 0.000000000000000000 ) ) ;
#36352 = VERTEX_POINT ( 'NONE', #7122 ) ;
#36353 = EDGE_CURVE ( 'NONE', #23354, #11801, #18926, .T. ) ;
#36354 = PRESENTATION_STYLE_ASSIGNMENT (( #23959 ) ) ;
#36355 = LINE ( 'NONE', #30860, #27576 ) ;
#36356 = CARTESIAN_POINT ( 'NONE',  ( 11.48173768534035943, 32.16538668264416145, 10.50000000000000000 ) ) ;
#36357 = EDGE_CURVE ( 'NONE', #12690, #3600, #10383, .T. ) ;
#36358 = DIRECTION ( 'NONE',  ( 0.7071067811865479058, 0.000000000000000000, -0.7071067811865472397 ) ) ;
#36359 = CARTESIAN_POINT ( 'NONE',  ( 17.24737218078871592, 14.85018931016522181, -17.94678984768380303 ) ) ;
#36360 = CARTESIAN_POINT ( 'NONE',  ( 8.110597763130101612, 20.77001312407615075, -23.39814370609576244 ) ) ;
#36361 = ORIENTED_EDGE ( 'NONE', *, *, #28655, .F. ) ;
#36362 = CARTESIAN_POINT ( 'NONE',  ( -21.25246432144205500, 11.48441715314585387, -10.88392780175655794 ) ) ;
#36363 = DIRECTION ( 'NONE',  ( 1.000000000000000000, 0.000000000000000000, 0.000000000000000000 ) ) ;
#36364 = DIRECTION ( 'NONE',  ( 0.000000000000000000, 0.000000000000000000, 1.000000000000000000 ) ) ;
#36365 = CARTESIAN_POINT ( 'NONE',  ( 10.55460110364784931, -19.04761602628894934, -23.81187091824480362 ) ) ;
#36366 = CARTESIAN_POINT ( 'NONE',  ( 16.23042486173695309, -23.86708630543283505, 18.87996532025784546 ) ) ;
#36367 = AXIS2_PLACEMENT_3D ( 'NONE', #35847, #8009, #5366 ) ;
#36368 = CARTESIAN_POINT ( 'NONE',  ( 19.79815887584821610, 19.84782313723624370, -5.000000000000007994 ) ) ;
#36369 = CARTESIAN_POINT ( 'NONE',  ( -15.36269874125315482, 26.70556469616796846, -6.416677824283240739 ) ) ;
#36370 = CARTESIAN_POINT ( 'NONE',  ( -14.44668725894448436, -16.26647643531120124, -24.50689636315220810 ) ) ;
#36371 = CARTESIAN_POINT ( 'NONE',  ( 13.43210918908202878, -25.89342552787512730, -8.311467949088584106 ) ) ;
#36372 = EDGE_CURVE ( 'NONE', #36487, #38004, #26013, .T. ) ;
#36373 = CARTESIAN_POINT ( 'NONE',  ( 0.5000000000000000000, 37.00000000000000711, 7.000000000000000000 ) ) ;
#36374 = EDGE_CURVE ( 'NONE', #1646, #15234, #10142, .T. ) ;
#36375 = ORIENTED_EDGE ( 'NONE', *, *, #21085, .F. ) ;
#36376 = VERTEX_POINT ( 'NONE', #14028 ) ;
#36377 = CARTESIAN_POINT ( 'NONE',  ( -7.743198174825847602, 19.19541131226637276, -27.89444138947942875 ) ) ;
#36378 = DIRECTION ( 'NONE',  ( 1.000000000000000000, 0.000000000000000000, 0.000000000000000000 ) ) ;
#36379 = CARTESIAN_POINT ( 'NONE',  ( -12.69365875748883710, 14.48606190191228116, 10.49999999999999822 ) ) ;
#36380 = AXIS2_PLACEMENT_3D ( 'NONE', #6351, #22191, #19349 ) ;
#36381 = FACE_OUTER_BOUND ( 'NONE', #33249, .T. ) ;
#36382 = ORIENTED_EDGE ( 'NONE', *, *, #39444, .F. ) ;
#36383 = CARTESIAN_POINT ( 'NONE',  ( 30.86596729670053563, -0.003225903683491773612, -5.000000000000000000 ) ) ;
#36384 = CIRCLE ( 'NONE', #3283, 16.00000000000000000 ) ;
#36385 = DIRECTION ( 'NONE',  ( 0.000000000000000000, 0.000000000000000000, 1.000000000000000000 ) ) ;
#36386 = DIRECTION ( 'NONE',  ( 0.5000000000000039968, 0.8660254037844363761, 0.000000000000000000 ) ) ;
#36387 = ORIENTED_EDGE ( 'NONE', *, *, #37220, .T. ) ;
#36388 = CARTESIAN_POINT ( 'NONE',  ( -21.70627603254861526, 0.7432028481183311497, -23.85585032862205423 ) ) ;
#36389 = DIRECTION ( 'NONE',  ( 0.000000000000000000, 0.000000000000000000, 1.000000000000000000 ) ) ;
#36390 = ORIENTED_EDGE ( 'NONE', *, *, #10041, .F. ) ;
#36391 = CARTESIAN_POINT ( 'NONE',  ( 32.67224823038714732, -4.906388482558933894, -9.920036700255655759 ) ) ;
#36392 = CARTESIAN_POINT ( 'NONE',  ( 18.85272453233919165, -29.14374917747379357, 12.73282698324887896 ) ) ;
#36393 = ORIENTED_EDGE ( 'NONE', *, *, #29011, .T. ) ;
#36394 = CARTESIAN_POINT ( 'NONE',  ( -16.30840571581334686, 28.99314201041626404, 13.92931973827731618 ) ) ;
#36395 = CONICAL_SURFACE ( 'NONE', #33797, 1.000000000000004441, 0.7853981633974522758 ) ;
#36396 = CARTESIAN_POINT ( 'NONE',  ( -16.00000000000000000, 22.50000000000000711, 11.00000000000000178 ) ) ;
#36397 = DIRECTION ( 'NONE',  ( -0.7071067811865511255, 0.000000000000000000, -0.7071067811865440200 ) ) ;
#36398 = ADVANCED_FACE ( 'NONE', ( #38412 ), #38032, .T. ) ;
#36399 = CARTESIAN_POINT ( 'NONE',  ( -7.341573453990910991, 26.39883817588575354, 20.69868183039782394 ) ) ;
#36400 = DIRECTION ( 'NONE',  ( 0.000000000000000000, 0.000000000000000000, 1.000000000000000000 ) ) ;
#36401 = ORIENTED_EDGE ( 'NONE', *, *, #10758, .T. ) ;
#36402 = CARTESIAN_POINT ( 'NONE',  ( 10.10646936306337729, 32.94553861768082470, 10.49999999999999645 ) ) ;
#36403 = FACE_OUTER_BOUND ( 'NONE', #8496, .T. ) ;
#36404 = CARTESIAN_POINT ( 'NONE',  ( 7.091416633034167027, 36.58341554298284137, -6.718649601333577692 ) ) ;
#36405 = DIRECTION ( 'NONE',  ( 0.000000000000000000, 0.000000000000000000, -1.000000000000000000 ) ) ;
#36406 = CARTESIAN_POINT ( 'NONE',  ( 23.61737546510196850, -7.194424252577104717, 21.00000000000000000 ) ) ;
#36407 = VECTOR ( 'NONE', #27893, 1000.000000000000000 ) ;
#36408 = CARTESIAN_POINT ( 'NONE',  ( 11.91734804082858012, -17.02703054535963290, -27.27743194981858821 ) ) ;
#36409 = DIRECTION ( 'NONE',  ( 0.000000000000000000, 0.000000000000000000, 1.000000000000000000 ) ) ;
#36410 = CARTESIAN_POINT ( 'NONE',  ( 5.473344025737210572, 14.11593743010426394, 10.49999999999999822 ) ) ;
#36411 = DIRECTION ( 'NONE',  ( 1.000000000000000000, 0.000000000000000000, 0.000000000000000000 ) ) ;
#36412 = VERTEX_POINT ( 'NONE', #32731 ) ;
#36413 = CARTESIAN_POINT ( 'NONE',  ( 11.00268105793074547, 17.54964049701253259, -27.44232077932614899 ) ) ;
#36414 = ORIENTED_EDGE ( 'NONE', *, *, #14721, .T. ) ;
#36415 = CARTESIAN_POINT ( 'NONE',  ( -15.33310310740069227, 26.06452538537273966, -7.829622284288262790 ) ) ;
#36416 = CARTESIAN_POINT ( 'NONE',  ( -17.70478766477605248, -23.47393717365530108, 19.27171037444159296 ) ) ;
#36417 = CARTESIAN_POINT ( 'NONE',  ( -9.331903152615899089, 11.35703883385581037, 11.00000000000000000 ) ) ;
#36418 = CARTESIAN_POINT ( 'NONE',  ( 15.06272762976659330, 25.82752587005803235, -9.240082175145575505 ) ) ;
#36419 = VERTEX_POINT ( 'NONE', #26420 ) ;
#36420 = CARTESIAN_POINT ( 'NONE',  ( 24.06311164388931445, -14.23786492898669387, -17.59357969373190755 ) ) ;
#36421 = VECTOR ( 'NONE', #34110, 1000.000000000000000 ) ;
#36422 = ORIENTED_EDGE ( 'NONE', *, *, #23609, .F. ) ;
#36424 = CYLINDRICAL_SURFACE ( 'NONE', #4337, 60.00000000000014211 ) ;
#36423 = CARTESIAN_POINT ( 'NONE',  ( -11.60894466518139545, 19.67965406879041623, -21.56349800617989132 ) ) ;
#36425 = CARTESIAN_POINT ( 'NONE',  ( -10.48684353440000194, -17.61503585894356050, -30.00000000000000000 ) ) ;
#36426 = DIRECTION ( 'NONE',  ( 0.000000000000000000, 0.000000000000000000, 1.000000000000000000 ) ) ;
#36427 = EDGE_CURVE ( 'NONE', #31487, #6543, #1852, .T. ) ;
#36428 = ORIENTED_EDGE ( 'NONE', *, *, #21931, .F. ) ;
#36429 = CARTESIAN_POINT ( 'NONE',  ( -35.35897274256637957, -12.18463282932507852, -6.291972826754448356 ) ) ;
#36430 = CARTESIAN_POINT ( 'NONE',  ( -15.03672417963925056, -26.50613305951797827, -6.888625959290687106 ) ) ;
#36431 = CARTESIAN_POINT ( 'NONE',  ( 14.96930490892014554, 21.54088032874971859, 7.500000000000010658 ) ) ;
#36432 = ORIENTED_EDGE ( 'NONE', *, *, #36703, .T. ) ;
#36433 = CARTESIAN_POINT ( 'NONE',  ( 24.26573961589400952, 2.169758022266998765, -17.60781658105700487 ) ) ;
#36434 = CARTESIAN_POINT ( 'NONE',  ( -7.935776944912362296, 22.65328985282726393, 13.00000000000000178 ) ) ;
#36435 = CARTESIAN_POINT ( 'NONE',  ( -36.53988293556027145, -0.5802930328939031046, 11.00000000000000000 ) ) ;
#36436 = ORIENTED_EDGE ( 'NONE', *, *, #4837, .T. ) ;
#36437 = CARTESIAN_POINT ( 'NONE',  ( -30.95087757567503672, -0.08989953764334629449, -5.000000000000000000 ) ) ;
#36438 = VERTEX_POINT ( 'NONE', #10585 ) ;
#36439 = CARTESIAN_POINT ( 'NONE',  ( 27.05815561153594473, -0.6001877338740869705, -15.34801442178561359 ) ) ;
#36440 = CIRCLE ( 'NONE', #18915, 1.000000000000000444 ) ;
#36441 = CARTESIAN_POINT ( 'NONE',  ( 33.29356883319506721, -10.99541271083377403, 18.42518152272108622 ) ) ;
#36442 = AXIS2_PLACEMENT_3D ( 'NONE', #22738, #35143, #13802 ) ;
#36443 = VERTEX_POINT ( 'NONE', #26823 ) ;
#36444 = CARTESIAN_POINT ( 'NONE',  ( -24.48240760914098502, 2.712249908169665158, -16.64270392758168526 ) ) ;
#36445 = DIRECTION ( 'NONE',  ( 0.000000000000000000, 0.000000000000000000, -1.000000000000000000 ) ) ;
#36446 = ADVANCED_FACE ( 'NONE', ( #4887 ), #38815, .T. ) ;
#36447 = CARTESIAN_POINT ( 'NONE',  ( -11.94134295108998423, 16.18301270189233421, 9.500000000000000000 ) ) ;
#36448 = DIRECTION ( 'NONE',  ( 0.000000000000000000, 0.000000000000000000, 1.000000000000000000 ) ) ;
#36449 = EDGE_CURVE ( 'NONE', #37593, #19542, #36343, .T. ) ;
#36450 = AXIS2_PLACEMENT_3D ( 'NONE', #12190, #5489, #6 ) ;
#36451 = FACE_OUTER_BOUND ( 'NONE', #29673, .T. ) ;
#36452 = EDGE_CURVE ( 'NONE', #39537, #17600, #31539, .T. ) ;
#36453 = DIRECTION ( 'NONE',  ( 0.000000000000000000, 0.000000000000000000, 1.000000000000000000 ) ) ;
#36454 = DIRECTION ( 'NONE',  ( -0.000000000000000000, -0.000000000000000000, 1.000000000000000000 ) ) ;
#36455 = VERTEX_POINT ( 'NONE', #23775 ) ;
#36456 = CARTESIAN_POINT ( 'NONE',  ( -23.92566527182959391, 5.176061040404443148, -14.76782440308691591 ) ) ;
#36457 = DIRECTION ( 'NONE',  ( -0.000000000000000000, -0.000000000000000000, -1.000000000000000000 ) ) ;
#36458 = DIRECTION ( 'NONE',  ( -1.000000000000000000, 0.000000000000000000, 0.000000000000000000 ) ) ;
#36459 = CARTESIAN_POINT ( 'NONE',  ( 18.70657072468925364, -18.32550425351821488, -18.79420699992576971 ) ) ;
#36460 = LINE ( 'NONE', #14725, #4108 ) ;
#36461 = CARTESIAN_POINT ( 'NONE',  ( 10.68641602773397636, 17.65275450399973423, -28.05634532095279710 ) ) ;
#36462 = CARTESIAN_POINT ( 'NONE',  ( 4.262995805457294793E-14, -26.57793081542402547, 12.73282698324853257 ) ) ;
#36463 = ORIENTED_EDGE ( 'NONE', *, *, #16332, .T. ) ;
#36464 = CARTESIAN_POINT ( 'NONE',  ( -14.03330550907330654, 18.32430351830364756, -19.75759142101557586 ) ) ;
#36465 = CARTESIAN_POINT ( 'NONE',  ( -25.56674216509407671, -13.93466449336376023, 20.94377226548387583 ) ) ;
#36466 = LINE ( 'NONE', #11686, #31483 ) ;
#36467 = CARTESIAN_POINT ( 'NONE',  ( 11.20058424733595892, 17.74459894083964784, -26.22661702102002224 ) ) ;
#36468 = ORIENTED_EDGE ( 'NONE', *, *, #31754, .T. ) ;
#36469 = CARTESIAN_POINT ( 'NONE',  ( 5.767236651883444587, 13.71142893291679243, 10.50000000000000000 ) ) ;
#36470 = VERTEX_POINT ( 'NONE', #20539 ) ;
#36472 = DIRECTION ( 'NONE',  ( 0.000000000000000000, 0.000000000000000000, 1.000000000000000000 ) ) ;
#36471 = CARTESIAN_POINT ( 'NONE',  ( -15.18975761229610022, 26.55092571743323404, -7.822985543115054341 ) ) ;
#36473 = EDGE_CURVE ( 'NONE', #10495, #11157, #32933, .T. ) ;
#36474 = CARTESIAN_POINT ( 'NONE',  ( -11.55840277251474646, -20.97515074911826360, -19.49524396482431143 ) ) ;
#36475 = CARTESIAN_POINT ( 'NONE',  ( 9.221287281574507944, 10.65863771052197784, 10.49999999999999822 ) ) ;
#36476 = EDGE_CURVE ( 'NONE', #21371, #18984, #13382, .T. ) ;
#36477 = CARTESIAN_POINT ( 'NONE',  ( -18.11135944020848498, -10.93062044766753793, -26.25495776335099762 ) ) ;
#36478 = CARTESIAN_POINT ( 'NONE',  ( -13.30200433025800777, -25.37444367340206242, -10.20725642727310678 ) ) ;
#36479 = CARTESIAN_POINT ( 'NONE',  ( -22.38472516250436328, -15.35952186208485593, 21.00000000000000000 ) ) ;
#36480 = CARTESIAN_POINT ( 'NONE',  ( 11.83150832767071314, 16.74097710667822270, -30.00000000000000000 ) ) ;
#36481 = ORIENTED_EDGE ( 'NONE', *, *, #25437, .F. ) ;
#36482 = CARTESIAN_POINT ( 'NONE',  ( 22.91801202536632687, 6.219164452797125264, -15.83068595770922826 ) ) ;
#36483 = DIRECTION ( 'NONE',  ( 0.9876883405951372152, -0.1564344650402341719, 0.000000000000000000 ) ) ;
#36484 = VECTOR ( 'NONE', #8703, 999.9999999999998863 ) ;
#36485 = CARTESIAN_POINT ( 'NONE',  ( 0.000000000000000000, 22.50000000000000355, 10.00000000000000000 ) ) ;
#36486 = CARTESIAN_POINT ( 'NONE',  ( 4.096822963000107620, 8.035697679810645866, 7.000000000000000000 ) ) ;
#36487 = VERTEX_POINT ( 'NONE', #35370 ) ;
#36488 = CARTESIAN_POINT ( 'NONE',  ( -22.50773814093716396, -0.7003419581363549140, -22.56284863701274190 ) ) ;
#36489 = CARTESIAN_POINT ( 'NONE',  ( 20.52860846656784588, 0.8226844751264725808, -28.70573514187030995 ) ) ;
#36490 = AXIS2_PLACEMENT_3D ( 'NONE', #4032, #25569, #12977 ) ;
#36491 = DIRECTION ( 'NONE',  ( 0.4067366430758009854, 0.9135454576426005335, 0.000000000000000000 ) ) ;
#36493 = VECTOR ( 'NONE', #36445, 1000.000000000000000 ) ;
#36492 = CARTESIAN_POINT ( 'NONE',  ( 26.13185812888305293, -11.12779425996326133, 20.94377226548378346 ) ) ;
#36494 = CARTESIAN_POINT ( 'NONE',  ( 21.88499642459564143, -5.528038495964486820, -29.99999999999998224 ) ) ;
#36495 = ADVANCED_FACE ( 'NONE', ( #29273 ), #17925, .T. ) ;
#36496 = DIRECTION ( 'NONE',  ( 1.000000000000000000, 0.000000000000000000, 0.000000000000000000 ) ) ;
#36497 = CIRCLE ( 'NONE', #1463, 0.5000000000000004441 ) ;
#36498 = EDGE_CURVE ( 'NONE', #1779, #10635, #14428, .T. ) ;
#36499 = EDGE_LOOP ( 'NONE', ( #17519, #20101, #25912, #28783 ) ) ;
#36500 = CARTESIAN_POINT ( 'NONE',  ( 9.559505275947156377, 25.28115294937476065, 6.000000000000000000 ) ) ;
#36501 = CARTESIAN_POINT ( 'NONE',  ( 6.713764256189890922, 35.89999254728742528, 10.49999999999999822 ) ) ;
#36502 = DIRECTION ( 'NONE',  ( -1.000000000000000000, 0.000000000000000000, 0.000000000000000000 ) ) ;
#36503 = CARTESIAN_POINT ( 'NONE',  ( 1.293490870016113403, 31.31656944015267996, -14.73212527803245919 ) ) ;
#36504 = DIRECTION ( 'NONE',  ( 0.000000000000000000, 0.000000000000000000, 1.000000000000000000 ) ) ;
#36505 = CARTESIAN_POINT ( 'NONE',  ( -3.853172919594720192, 21.57294901687549427, 12.00000000000000000 ) ) ;
#36506 = DIRECTION ( 'NONE',  ( -0.3090169943749573878, -0.9510565162951503115, 0.000000000000000000 ) ) ;
#36507 = DIRECTION ( 'NONE',  ( -0.000000000000000000, -0.000000000000000000, -1.000000000000000000 ) ) ;
#36508 = DIRECTION ( 'NONE',  ( 0.9510565162951543083, 0.3090169943749450088, 0.000000000000000000 ) ) ;
#36509 = CARTESIAN_POINT ( 'NONE',  ( 9.762440214479946476, -29.39637225272704057, 11.00000000000000000 ) ) ;
#36510 = CARTESIAN_POINT ( 'NONE',  ( 14.65877742485253421, 27.77006656560355680, -8.242821808329072297 ) ) ;
#36511 = DIRECTION ( 'NONE',  ( 1.000000000000000000, 0.000000000000000000, 0.000000000000000000 ) ) ;
#36512 = ORIENTED_EDGE ( 'NONE', *, *, #38029, .T. ) ;
#36513 = VECTOR ( 'NONE', #37626, 1000.000000000000227 ) ;
#36515 = CARTESIAN_POINT ( 'NONE',  ( 11.77090408390491305, 15.39748370681878775, 12.00000000000000000 ) ) ;
#36514 = CARTESIAN_POINT ( 'NONE',  ( -16.37425825659163792, 12.35560620482834970, -30.00000000000000000 ) ) ;
#36516 = DIRECTION ( 'NONE',  ( 0.1045284632676437842, -0.9945218953682744001, 0.000000000000000000 ) ) ;
#36517 = CARTESIAN_POINT ( 'NONE',  ( 15.06737418716398480, -26.14303779321338084, -8.767816294897599505 ) ) ;
#36518 = CARTESIAN_POINT ( 'NONE',  ( 15.39919595897969806, 26.75075905497483930, -5.946079338151666782 ) ) ;
#36519 = CARTESIAN_POINT ( 'NONE',  ( 14.83164354014592945, 25.63566593113468173, -10.17862006668016051 ) ) ;
#36520 = ORIENTED_EDGE ( 'NONE', *, *, #30997, .T. ) ;
#36521 = CARTESIAN_POINT ( 'NONE',  ( 0.5000000000000035527, 32.50000000000000000, 10.50000000000000178 ) ) ;
#36522 = DIRECTION ( 'NONE',  ( -0.000000000000000000, -0.000000000000000000, -1.000000000000000000 ) ) ;
#36523 = CARTESIAN_POINT ( 'NONE',  ( -29.42985357383858869, -23.05064539992688921, -7.560940416845337353 ) ) ;
#36524 = CARTESIAN_POINT ( 'NONE',  ( 3.957494336073486441, -24.62814106778900225, -8.398072415613651032 ) ) ;
#36525 = CARTESIAN_POINT ( 'NONE',  ( 11.74988495535431454, 18.20669567406710954, -23.89381587855401534 ) ) ;
#36526 = CARTESIAN_POINT ( 'NONE',  ( 20.21597881006783837, 12.43147293057613645, -12.89012422323875917 ) ) ;
#36527 = DIRECTION ( 'NONE',  ( 0.07391278520356295290, -0.7032331762534080877, -0.7071067811865440200 ) ) ;
#36528 = ADVANCED_FACE ( 'NONE', ( #14229 ), #23172, .F. ) ;
#36529 = CARTESIAN_POINT ( 'NONE',  ( -4.218276626635449666, 29.63384946082300431, -15.71993721405139155 ) ) ;
#36530 = ORIENTED_EDGE ( 'NONE', *, *, #5088, .T. ) ;
#36531 = VECTOR ( 'NONE', #2925, 1000.000000000000000 ) ;
#36532 = CARTESIAN_POINT ( 'NONE',  ( -23.18947492591163240, 13.38844959084118535, 11.00000000000000000 ) ) ;
#36533 = ORIENTED_EDGE ( 'NONE', *, *, #24916, .F. ) ;
#36534 = FACE_OUTER_BOUND ( 'NONE', #37189, .T. ) ;
#36535 = AXIS2_PLACEMENT_3D ( 'NONE', #5785, #29569, #38915 ) ;
#36536 = DIRECTION ( 'NONE',  ( 0.000000000000000000, 0.000000000000000000, 1.000000000000000000 ) ) ;
#36537 = CARTESIAN_POINT ( 'NONE',  ( -25.10967418331198431, 0.5688158262986504621, -17.45731339471036137 ) ) ;
#36538 = CARTESIAN_POINT ( 'NONE',  ( 19.70705905309527139, -5.958174894697001456, -28.49491022416014019 ) ) ;
#36539 = CIRCLE ( 'NONE', #26143, 1.000000000000000000 ) ;
#36540 = VERTEX_POINT ( 'NONE', #17092 ) ;
#36541 = CONTEXT_DEPENDENT_SHAPE_REPRESENTATION ( #36595, #31748 ) ;
#36542 = DIRECTION ( 'NONE',  ( 1.000000000000000000, 0.000000000000000000, 0.000000000000000000 ) ) ;
#36543 = ORIENTED_EDGE ( 'NONE', *, *, #1303, .T. ) ;
#36544 = DIRECTION ( 'NONE',  ( 1.000000000000000000, 0.000000000000000000, 0.000000000000000000 ) ) ;
#36545 = CYLINDRICAL_SURFACE ( 'NONE', #32561, 0.5000000000000004441 ) ;
#36546 = CIRCLE ( 'NONE', #6034, 1.000000000000000888 ) ;
#36547 = FACE_OUTER_BOUND ( 'NONE', #23874, .T. ) ;
#36548 = ORIENTED_EDGE ( 'NONE', *, *, #34355, .T. ) ;
#36549 = SURFACE_STYLE_FILL_AREA ( #39593 ) ;
#36550 = FACE_OUTER_BOUND ( 'NONE', #18705, .T. ) ;
#36551 = DIRECTION ( 'NONE',  ( -0.000000000000000000, -0.000000000000000000, -1.000000000000000000 ) ) ;
#36552 = CARTESIAN_POINT ( 'NONE',  ( 13.37378135583786332, 20.59160479820249634, 9.500000000000000000 ) ) ;
#36553 = CARTESIAN_POINT ( 'NONE',  ( 17.60659027557944967, -14.36865807356775626, -23.06510994001489578 ) ) ;
#36554 = CARTESIAN_POINT ( 'NONE',  ( 20.03430053822841828, 14.93931088505822657, -5.965758641065874279 ) ) ;
#36555 = AXIS2_PLACEMENT_3D ( 'NONE', #178, #383, #25156 ) ;
#36556 = CARTESIAN_POINT ( 'NONE',  ( 12.40530672973724080, 32.54280113045124523, -5.895856452077529397 ) ) ;
#36557 = ORIENTED_EDGE ( 'NONE', *, *, #39560, .F. ) ;
#36558 = CARTESIAN_POINT ( 'NONE',  ( -21.55543886414327304, 11.63864511105562194, -8.900058298306362303 ) ) ;
#36559 = CARTESIAN_POINT ( 'NONE',  ( 1.605696033269625955, 17.55816537872232530, 12.00000000000000000 ) ) ;
#36560 = CARTESIAN_POINT ( 'NONE',  ( 14.52509594610761923, 21.97885917798724975, 10.50000000000000355 ) ) ;
#36561 = CARTESIAN_POINT ( 'NONE',  ( 15.52008768824105545, -26.55333232259659582, -7.352602181182319008 ) ) ;
#36562 = CARTESIAN_POINT ( 'NONE',  ( 12.30736835487432579, 14.81698729810772619, 7.499999999999997335 ) ) ;
#36563 = CARTESIAN_POINT ( 'NONE',  ( 13.47223693944937750, 18.09844039693851769, -30.00000000000000355 ) ) ;
#36564 = CARTESIAN_POINT ( 'NONE',  ( -15.16325337730098255, 26.31972413366512242, -8.296376571532537270 ) ) ;
#36565 = VECTOR ( 'NONE', #15209, 1000.000000000000114 ) ;
#36566 = CARTESIAN_POINT ( 'NONE',  ( -23.62391352436328873, -26.37202438933310589, -7.195775402117879693 ) ) ;
#36567 = CARTESIAN_POINT ( 'NONE',  ( 10.73433329256054414, -21.08021252179972294, -19.58150332943896643 ) ) ;
#36568 = EDGE_CURVE ( 'NONE', #35341, #28707, #2052, .T. ) ;
#36569 = CARTESIAN_POINT ( 'NONE',  ( 10.10646936306337729, 32.94553861768082470, 7.499999999999997335 ) ) ;
#36570 = VERTEX_POINT ( 'NONE', #17498 ) ;
#36571 = VERTEX_POINT ( 'NONE', #20743 ) ;
#36572 = CARTESIAN_POINT ( 'NONE',  ( -11.83993818029857437, 32.97031935882627351, -6.772281498610635886 ) ) ;
#36573 = CARTESIAN_POINT ( 'NONE',  ( -13.47830981910551529, 21.58612669357095371, 7.000000000000000000 ) ) ;
#36574 = DIRECTION ( 'NONE',  ( 0.9135454576426005335, -0.4067366430758009299, 0.000000000000000000 ) ) ;
#36575 = VECTOR ( 'NONE', #39246, 1000.000000000000000 ) ;
#36576 = LINE ( 'NONE', #3250, #29946 ) ;
#36577 = VERTEX_POINT ( 'NONE', #16685 ) ;
#36578 = CARTESIAN_POINT ( 'NONE',  ( 27.08975123792179218, 0.3078043105649791999, -14.48142009230936900 ) ) ;
#36579 = ADVANCED_FACE ( 'NONE', ( #1245 ), #13626, .T. ) ;
#36580 = DIRECTION ( 'NONE',  ( 1.000000000000000000, 0.000000000000000000, 0.000000000000000000 ) ) ;
#36581 = CARTESIAN_POINT ( 'NONE',  ( -2.525645716490712012, 8.212903943950955465, 10.99999999999999289 ) ) ;
#36582 = ADVANCED_FACE ( 'NONE', ( #39409 ), #24375, .F. ) ;
#36583 = ORIENTED_EDGE ( 'NONE', *, *, #13464, .T. ) ;
#36584 = CARTESIAN_POINT ( 'NONE',  ( -20.96866610389652053, 0.8170365396961356552, -26.22569017582818063 ) ) ;
#36585 = FACE_OUTER_BOUND ( 'NONE', #36773, .T. ) ;
#36586 = ORIENTED_EDGE ( 'NONE', *, *, #37807, .F. ) ;
#36587 = CARTESIAN_POINT ( 'NONE',  ( 24.19774762110479926, -2.790396721216801268, -20.13477434463229798 ) ) ;
#36588 = CIRCLE ( 'NONE', #4766, 1.000000000000000888 ) ;
#36589 = CARTESIAN_POINT ( 'NONE',  ( 37.17935095643323962, -12.86265498539263064, 13.32518128616619357 ) ) ;
#36590 = ORIENTED_EDGE ( 'NONE', *, *, #23586, .F. ) ;
#36591 = CARTESIAN_POINT ( 'NONE',  ( -16.81416712651214596, 27.17354907310119572, 13.92931973827808889 ) ) ;
#36592 = CARTESIAN_POINT ( 'NONE',  ( 17.62780868050938565, -18.45076755199376706, 20.82122704794079837 ) ) ;
#36593 = CARTESIAN_POINT ( 'NONE',  ( -3.992867117591420545, 8.524771480177605554, 7.499999999999997335 ) ) ;
#36594 = CARTESIAN_POINT ( 'NONE',  ( -8.207473342610091649, 28.06734471880738369, 20.25080042701566541 ) ) ;
#36595 =( REPRESENTATION_RELATIONSHIP ('NONE','NONE', #15382, #28068 ) REPRESENTATION_RELATIONSHIP_WITH_TRANSFORMATION ( #23749 )SHAPE_REPRESENTATION_RELATIONSHIP( ) );
#36596 = VECTOR ( 'NONE', #18613, 1000.000000000000000 ) ;
#36597 = DIRECTION ( 'NONE',  ( 1.000000000000000000, 0.000000000000000000, 0.000000000000000000 ) ) ;
#36598 = ORIENTED_EDGE ( 'NONE', *, *, #37103, .F. ) ;
#36599 = CYLINDRICAL_SURFACE ( 'NONE', #39861, 1.000000000000000000 ) ;
#36600 = EDGE_CURVE ( 'NONE', #3501, #400, #38680, .T. ) ;
#36601 = CARTESIAN_POINT ( 'NONE',  ( -14.57486473880221745, 26.18419839932921533, 11.00000000000000000 ) ) ;
#36602 = EDGE_CURVE ( 'NONE', #23885, #9748, #18094, .T. ) ;
#36603 = CARTESIAN_POINT ( 'NONE',  ( 3.318832056366368022, 20.47935037984655793, -27.74009767284220729 ) ) ;
#36604 = CARTESIAN_POINT ( 'NONE',  ( 2.587660364795204782, 9.681887955242936883, 13.00000000000000178 ) ) ;
#36605 = VECTOR ( 'NONE', #17929, 1000.000000000000114 ) ;
#36606 = CARTESIAN_POINT ( 'NONE',  ( 19.72827082054694259, 4.852702923338547691, 19.99202127657091665 ) ) ;
#36607 = CARTESIAN_POINT ( 'NONE',  ( 12.27390640609045036, -16.43329545370340838, -29.28898356251528412 ) ) ;
#36608 = CARTESIAN_POINT ( 'NONE',  ( 8.412270287199559604, 10.07085245822950981, 10.49999999999999822 ) ) ;
#36609 = CARTESIAN_POINT ( 'NONE',  ( -12.80736835487442349, 15.68301270189233954, 11.00000000000000000 ) ) ;
#36610 = CARTESIAN_POINT ( 'NONE',  ( -14.06524961900331583, 27.71236540882611976, 7.000000000000000000 ) ) ;
#36611 = ORIENTED_EDGE ( 'NONE', *, *, #14867, .F. ) ;
#36612 = CARTESIAN_POINT ( 'NONE',  ( 14.25784677919622823, 24.55947563112205145, -12.54307605572578055 ) ) ;
#36613 = VECTOR ( 'NONE', #14875, 1000.000000000000114 ) ;
#36614 = VERTEX_POINT ( 'NONE', #15433 ) ;
#36615 = CARTESIAN_POINT ( 'NONE',  ( -11.20756347206190284, 17.73954208893731277, -26.22736157229892839 ) ) ;
#36616 = CARTESIAN_POINT ( 'NONE',  ( -17.49459433713212064, -24.91609123032629469, 18.42518152272109333 ) ) ;
#36617 = CARTESIAN_POINT ( 'NONE',  ( 15.14201655615061526, -26.36804160454520485, -7.828362067540088454 ) ) ;
#36618 = LINE ( 'NONE', #11832, #28259 ) ;
#36619 = CARTESIAN_POINT ( 'NONE',  ( 11.07485645340150171, 17.25102576792224340, -29.35029984720032914 ) ) ;
#36620 = ORIENTED_EDGE ( 'NONE', *, *, #35595, .T. ) ;
#36621 = CARTESIAN_POINT ( 'NONE',  ( 22.67567822676405953, -14.36290881944746900, -18.61438165153855095 ) ) ;
#36622 = ORIENTED_EDGE ( 'NONE', *, *, #9617, .T. ) ;
#36624 = CARTESIAN_POINT ( 'NONE',  ( -6.864468484317908903, 35.45925531351075222, 10.49999999999999645 ) ) ;
#36623 = CARTESIAN_POINT ( 'NONE',  ( -14.29471368831881328, 25.61313551457574178, -11.55151809035900712 ) ) ;
#36625 = CARTESIAN_POINT ( 'NONE',  ( -17.10877210688781958, -26.84738589896849703, -7.313269270788000043 ) ) ;
#36626 = ADVANCED_FACE ( 'NONE', ( #30680 ), #21722, .T. ) ;
#36627 = DIRECTION ( 'NONE',  ( 0.000000000000000000, 0.000000000000000000, 1.000000000000000000 ) ) ;
#36628 = VECTOR ( 'NONE', #4470, 1000.000000000000114 ) ;
#36629 = ORIENTED_EDGE ( 'NONE', *, *, #8407, .T. ) ;
#36630 = CARTESIAN_POINT ( 'NONE',  ( -35.25710161250010799, -11.00445477990710685, -6.726159309538959796 ) ) ;
#36631 = PRODUCT_DEFINITION_CONTEXT ( 'detailed design', #6209, 'design' ) ;
#36632 = CARTESIAN_POINT ( 'NONE',  ( -15.13531929286639155, -26.65245416579944759, -5.000000000000000888 ) ) ;
#36633 = LINE ( 'NONE', #21189, #13796 ) ;
#36634 = ORIENTED_EDGE ( 'NONE', *, *, #30287, .T. ) ;
#36635 = CARTESIAN_POINT ( 'NONE',  ( 20.86090429746450781, 3.082049809194417289, -25.22830055382215875 ) ) ;
#36636 = DIRECTION ( 'NONE',  ( 0.6445931928399499800, 0.000000000000000000, 0.7645257456386926886 ) ) ;
#36637 = DIRECTION ( 'NONE',  ( 0.4067366430758009299, 0.9135454576426005335, 0.000000000000000000 ) ) ;
#36638 = ORIENTED_EDGE ( 'NONE', *, *, #31263, .F. ) ;
#36639 = CARTESIAN_POINT ( 'NONE',  ( -30.84155282226171124, -0.08171445749998075547, -6.415951416867066825 ) ) ;
#36640 = ORIENTED_EDGE ( 'NONE', *, *, #23139, .F. ) ;
#36641 = CARTESIAN_POINT ( 'NONE',  ( 31.13255865061531935, -1.317985051374632066, -9.160379792037252500 ) ) ;
#36642 = CARTESIAN_POINT ( 'NONE',  ( 33.53288488731369910, -7.900844017966136335, 17.92354375535250810 ) ) ;
#36643 = EDGE_LOOP ( 'NONE', ( #19432, #27957, #34045, #38688 ) ) ;
#36644 = CARTESIAN_POINT ( 'NONE',  ( -22.04274155920867884, 2.809314319882194599, -21.86559244833277305 ) ) ;
#36645 = DIRECTION ( 'NONE',  ( 0.1045284632676437703, -0.9945218953682742891, 0.000000000000000000 ) ) ;
#36646 = CIRCLE ( 'NONE', #4185, 1.000000000000000888 ) ;
#36647 = DIRECTION ( 'NONE',  ( -0.000000000000000000, -0.000000000000000000, -1.000000000000000000 ) ) ;
#36648 = CARTESIAN_POINT ( 'NONE',  ( -14.98890121934590347, -28.67928442654175569, 11.55979286843935050 ) ) ;
#36649 = PLANE ( 'NONE',  #9115 ) ;
#36650 = ADVANCED_FACE ( 'NONE', ( #12381 ), #2843, .T. ) ;
#36651 = AXIS2_PLACEMENT_3D ( 'NONE', #8021, #13711, #29561 ) ;
#36652 = VECTOR ( 'NONE', #19651, 1000.000000000000114 ) ;
#36653 = CARTESIAN_POINT ( 'NONE',  ( -2.485571585149885632, -11.24999999999987566, 10.00000000000000000 ) ) ;
#36654 = CYLINDRICAL_SURFACE ( 'NONE', #15274, 1.000000000000000888 ) ;
#36655 = ORIENTED_EDGE ( 'NONE', *, *, #30468, .T. ) ;
#36656 = CARTESIAN_POINT ( 'NONE',  ( -23.86420076115572186, 7.970790765993674754, -8.878367169149885996 ) ) ;
#36657 = LINE ( 'NONE', #8014, #24198 ) ;
#36658 = DIRECTION ( 'NONE',  ( 0.000000000000000000, 0.000000000000000000, 1.000000000000000000 ) ) ;
#36659 = CARTESIAN_POINT ( 'NONE',  ( 15.51366702551998955, -14.30026934863555788, -26.35746096789312176 ) ) ;
#36660 = CARTESIAN_POINT ( 'NONE',  ( 11.87435565298210882, 15.06698729810772619, 10.00000000000000000 ) ) ;
#36661 = CARTESIAN_POINT ( 'NONE',  ( 11.95885763855134343, 20.12759201311160950, -20.50636973948041586 ) ) ;
#36662 = CARTESIAN_POINT ( 'NONE',  ( -10.13173764377114239, -27.22067640326290672, 12.73282698326143425 ) ) ;
#36663 = VERTEX_POINT ( 'NONE', #21129 ) ;
#36664 = CARTESIAN_POINT ( 'NONE',  ( -13.78067611128539838, 16.29607663636611647, -24.15683527709576239 ) ) ;
#36665 = CARTESIAN_POINT ( 'NONE',  ( -24.39151161285703040, -15.73551128733878102, 20.94377226548378701 ) ) ;
#36666 = DIRECTION ( 'NONE',  ( 0.000000000000000000, 0.000000000000000000, 1.000000000000000000 ) ) ;
#36667 = CARTESIAN_POINT ( 'NONE',  ( 12.94909081049822142, 21.61942785653063126, -17.44119972322781109 ) ) ;
#36668 = ORIENTED_EDGE ( 'NONE', *, *, #26974, .F. ) ;
#36669 = CARTESIAN_POINT ( 'NONE',  ( -14.47283171447380212, 21.48159823030330884, 11.00000000000000355 ) ) ;
#36670 = VERTEX_POINT ( 'NONE', #27028 ) ;
#36672 = CYLINDRICAL_SURFACE ( 'NONE', #21821, 1.000000000000000000 ) ;
#36671 = CARTESIAN_POINT ( 'NONE',  ( -14.89167003689908775, 25.93687804966682364, -9.701378797208148441 ) ) ;
#36673 = CARTESIAN_POINT ( 'NONE',  ( -13.03749113462529685, -23.09334588019250489, -15.44824872094964796 ) ) ;
#36674 = EDGE_CURVE ( 'NONE', #31582, #2112, #24174, .T. ) ;
#36675 = CARTESIAN_POINT ( 'NONE',  ( -5.947717410344456113, 34.62949535663729250, 10.50000000000000000 ) ) ;
#36676 = AXIS2_PLACEMENT_3D ( 'NONE', #31720, #25614, #10187 ) ;
#36677 = CARTESIAN_POINT ( 'NONE',  ( -34.06221145678576079, -17.84677894165469070, -5.435607523623667170 ) ) ;
#36678 = CARTESIAN_POINT ( 'NONE',  ( -7.489852218780842286, -19.16649717563461408, -28.77838134633300626 ) ) ;
#36679 = CYLINDRICAL_SURFACE ( 'NONE', #24790, 60.00000000000001421 ) ;
#36680 = CARTESIAN_POINT ( 'NONE',  ( 13.62177027565629395, 19.65269395691544574, -18.61040937102566772 ) ) ;
#36682 = EDGE_CURVE ( 'NONE', #39628, #37016, #14635, .T. ) ;
#36681 = ORIENTED_EDGE ( 'NONE', *, *, #22739, .T. ) ;
#36683 = CARTESIAN_POINT ( 'NONE',  ( 21.51332232471817818, 6.076221697413749290, -19.98667434612283955 ) ) ;
#36684 = DIRECTION ( 'NONE',  ( 1.000000000000000000, 0.000000000000000000, 0.000000000000000000 ) ) ;
#36685 = EDGE_CURVE ( 'NONE', #21498, #13490, #35433, .T. ) ;
#36686 = DIRECTION ( 'NONE',  ( -0.1045284632676422437, 0.9945218953682746221, 0.000000000000000000 ) ) ;
#36687 = DIRECTION ( 'NONE',  ( 0.5254827454987509583, -0.4731467892558243182, -0.7071067811865472397 ) ) ;
#36688 = VECTOR ( 'NONE', #2736, 1000.000000000000000 ) ;
#36689 = ORIENTED_EDGE ( 'NONE', *, *, #30665, .F. ) ;
#36690 = CARTESIAN_POINT ( 'NONE',  ( -31.63647013363080873, -0.8270238094956997577, -5.469293166058980304 ) ) ;
#36691 = CARTESIAN_POINT ( 'NONE',  ( 20.48330953517068664, 0.8273339926270942835, -30.00000000000000000 ) ) ;
#36692 = VECTOR ( 'NONE', #33220, 1000.000000000000000 ) ;
#36693 = ADVANCED_FACE ( 'NONE', ( #24772 ), #21671, .T. ) ;
#36694 = VECTOR ( 'NONE', #3045, 1000.000000000000114 ) ;
#36695 = CARTESIAN_POINT ( 'NONE',  ( 5.034171952702014785, 35.03623199971300295, 10.50000000000000000 ) ) ;
#36696 = CARTESIAN_POINT ( 'NONE',  ( 26.53285121770567301, -6.841429973034632184, 20.69868183039801224 ) ) ;
#36697 = CARTESIAN_POINT ( 'NONE',  ( -14.09933648065464062, 26.02968990214173317, 7.000000000000000000 ) ) ;
#36698 = DIRECTION ( 'NONE',  ( 0.000000000000000000, 0.000000000000000000, -1.000000000000000000 ) ) ;
#36699 = ORIENTED_EDGE ( 'NONE', *, *, #20676, .T. ) ;
#36700 = ADVANCED_FACE ( 'NONE', ( #30482 ), #17896, .T. ) ;
#36701 = LINE ( 'NONE', #24304, #22315 ) ;
#36702 = EDGE_CURVE ( 'NONE', #34372, #8296, #6252, .T. ) ;
#36703 = EDGE_CURVE ( 'NONE', #21181, #37730, #27052, .T. ) ;
#36704 = CARTESIAN_POINT ( 'NONE',  ( -11.44134295108998955, 15.31698729810788784, 10.00000000000000000 ) ) ;
#36705 = DIRECTION ( 'NONE',  ( 0.000000000000000000, 0.000000000000000000, 1.000000000000000000 ) ) ;
#36706 = CARTESIAN_POINT ( 'NONE',  ( 3.705883046374359946, 36.09340752835787214, -9.737407412482861346 ) ) ;
#36707 = PLANE ( 'NONE',  #32153 ) ;
#36708 = CARTESIAN_POINT ( 'NONE',  ( -7.713869163866016621, 10.18146832927085121, 10.49999999999999822 ) ) ;
#36709 = CARTESIAN_POINT ( 'NONE',  ( -13.87104230352202272, 20.53934056656885687, 9.500000000000000000 ) ) ;
#36710 = CIRCLE ( 'NONE', #5556, 17.99999999999993250 ) ;
#36711 = DIRECTION ( 'NONE',  ( -0.1045284632676437564, 0.9945218953682744001, 0.000000000000000000 ) ) ;
#36712 = LINE ( 'NONE', #24507, #31345 ) ;
#36713 = CARTESIAN_POINT ( 'NONE',  ( 12.28720923547795429, -14.55658080553756406, 23.00000000000000000 ) ) ;
#36714 = CARTESIAN_POINT ( 'NONE',  ( 14.49954575914088117, 27.42131279283395529, -9.169623025717175580 ) ) ;
#36715 = LINE ( 'NONE', #39947, #25613 ) ;
#36716 = ORIENTED_EDGE ( 'NONE', *, *, #39192, .F. ) ;
#36719 = CIRCLE ( 'NONE', #10757, 17.00000000000000000 ) ;
#36718 = DIRECTION ( 'NONE',  ( 0.6724985119639513842, 0.2185080122244070777, -0.7071067811865541231 ) ) ;
#36717 = CARTESIAN_POINT ( 'NONE',  ( -18.00665338107467051, 15.31517184407994669, -14.87167487327246640 ) ) ;
#36720 = CARTESIAN_POINT ( 'NONE',  ( 4.955893845527869601, 31.78717482294046093, 10.74999999999999289 ) ) ;
#36721 = CARTESIAN_POINT ( 'NONE',  ( 9.786533863580281434, -18.56354127006651211, -26.22476242672100000 ) ) ;
#36722 = CARTESIAN_POINT ( 'NONE',  ( -12.11431921870781281, -16.53859995802357474, -29.29246340261923720 ) ) ;
#36723 = CARTESIAN_POINT ( 'NONE',  ( 32.09165771328607519, 1.123514972292635861, 13.32518128616608521 ) ) ;
#36724 = CARTESIAN_POINT ( 'NONE',  ( 15.27973808755479723, 26.56710540162124801, -7.356736264727379293 ) ) ;
#36725 = ORIENTED_EDGE ( 'NONE', *, *, #2698, .T. ) ;
#36726 = DIRECTION ( 'NONE',  ( 0.9781476007338072431, 0.2079116908177517375, 0.000000000000000000 ) ) ;
#36727 = CARTESIAN_POINT ( 'NONE',  ( -9.892954722048926897, 20.95745441963943279, 10.49999999999999289 ) ) ;
#36728 = EDGE_CURVE ( 'NONE', #19765, #6144, #10780, .T. ) ;
#36729 = CARTESIAN_POINT ( 'NONE',  ( -28.85413502746283498, -22.61874590850457523, -8.864180790608637395 ) ) ;
#36730 = CARTESIAN_POINT ( 'NONE',  ( 1.335132817696313978, -21.21848675767797587, -23.33513061438837610 ) ) ;
#36731 = CARTESIAN_POINT ( 'NONE',  ( 15.02468189385244024, 25.06093797422134273, -10.19064726329248138 ) ) ;
#36732 = EDGE_CURVE ( 'NONE', #38335, #32089, #16238, .T. ) ;
#36733 = CARTESIAN_POINT ( 'NONE',  ( 22.21982769557913784, 11.10346373912405049, -5.482723809593267106 ) ) ;
#36734 = FACE_OUTER_BOUND ( 'NONE', #35039, .T. ) ;
#36735 = CARTESIAN_POINT ( 'NONE',  ( -5.141937788641745222, 36.05078749574169450, -9.302716111124565757 ) ) ;
#36736 = ORIENTED_EDGE ( 'NONE', *, *, #39922, .F. ) ;
#36737 = CARTESIAN_POINT ( 'NONE',  ( -20.24687895915023716, -3.686470766795223675, -28.55337830014365963 ) ) ;
#36738 = CARTESIAN_POINT ( 'NONE',  ( -18.37899676825032103, 22.33688965561464812, 13.32518128618448650 ) ) ;
#36739 = ORIENTED_EDGE ( 'NONE', *, *, #10527, .F. ) ;
#36740 = CARTESIAN_POINT ( 'NONE',  ( 2.518583951651050867, 7.712953814960687104, 7.499999999999990230 ) ) ;
#36741 = CARTESIAN_POINT ( 'NONE',  ( 9.892954722048896699, 20.95745441963929423, 10.50000000000000533 ) ) ;
#36742 = VECTOR ( 'NONE', #8129, 1000.000000000000000 ) ;
#36743 = CARTESIAN_POINT ( 'NONE',  ( -29.99078130865111547, 0.6403921273831606475, -7.361166318520860230 ) ) ;
#36744 = CARTESIAN_POINT ( 'NONE',  ( 34.70950711422840840, -12.76021984960118338, -7.998181218355810529 ) ) ;
#36745 = VECTOR ( 'NONE', #15534, 1000.000000000000000 ) ;
#36746 = CONICAL_SURFACE ( 'NONE', #11428, 1.000000000000004441, 0.7853981633974522758 ) ;
#36747 = ORIENTED_EDGE ( 'NONE', *, *, #7096, .T. ) ;
#36748 = DIRECTION ( 'NONE',  ( -1.000000000000000000, 0.000000000000000000, 0.000000000000000000 ) ) ;
#36749 = VERTEX_POINT ( 'NONE', #15835 ) ;
#36750 = FACE_BOUND ( 'NONE', #33828, .T. ) ;
#36751 = DIRECTION ( 'NONE',  ( 0.4999999999999921174, -0.8660254037844431485, -0.000000000000000000 ) ) ;
#36752 = DIRECTION ( 'NONE',  ( 1.000000000000000000, 0.000000000000000000, 0.000000000000000000 ) ) ;
#36753 = ORIENTED_EDGE ( 'NONE', *, *, #9062, .T. ) ;
#36754 =( LENGTH_UNIT ( ) NAMED_UNIT ( * ) SI_UNIT ( .MILLI., .METRE. ) );
#36755 = CARTESIAN_POINT ( 'NONE',  ( -12.67417846324130259, 14.47720745114830443, 7.499999999999993783 ) ) ;
#36756 = CARTESIAN_POINT ( 'NONE',  ( -37.48531001978128074, -11.24999991186452775, 11.00000000000002309 ) ) ;
#36757 = CARTESIAN_POINT ( 'NONE',  ( 3.459945280434955972, 26.15050560728434448, 23.00000000000000355 ) ) ;
#36758 = CARTESIAN_POINT ( 'NONE',  ( 29.70821612178828630, -22.86209932760419861, -7.558102420314961378 ) ) ;
#36759 = CARTESIAN_POINT ( 'NONE',  ( 17.51810871584791940, 13.86375751818291846, -19.02218500560174874 ) ) ;
#36760 = CARTESIAN_POINT ( 'NONE',  ( 7.501377273760489572, 19.07882637373012713, -29.99999999999999645 ) ) ;
#36761 = ORIENTED_EDGE ( 'NONE', *, *, #2944, .F. ) ;
#36762 = CARTESIAN_POINT ( 'NONE',  ( -22.27105386152767608, 10.77722882959855966, -7.426802025917476513 ) ) ;
#36763 = CARTESIAN_POINT ( 'NONE',  ( -3.503793317224518145, 8.420815634768723967, 11.00000000000000000 ) ) ;
#36764 = CARTESIAN_POINT ( 'NONE',  ( 15.59663170297798729, -26.74431364097485897, -5.944724389301430989 ) ) ;
#36765 = DIRECTION ( 'NONE',  ( 0.000000000000000000, 0.000000000000000000, 1.000000000000000000 ) ) ;
#36766 = CARTESIAN_POINT ( 'NONE',  ( 35.84808252048253507, -3.038699442442335030, -4.999999999999996447 ) ) ;
#36767 = CARTESIAN_POINT ( 'NONE',  ( -11.46203485482419815, 18.45655401365020509, -23.85043275240798266 ) ) ;
#36768 = VECTOR ( 'NONE', #26475, 1000.000000000000000 ) ;
#36769 = CARTESIAN_POINT ( 'NONE',  ( -15.94698504394344596, -17.91589082531237764, -21.01243287115451963 ) ) ;
#36770 = CARTESIAN_POINT ( 'NONE',  ( 13.02878361272089691, -26.04899829346652140, -6.894447511635101833 ) ) ;
#36771 = CARTESIAN_POINT ( 'NONE',  ( -6.404490139165758933, 34.42612703509939820, 9.500000000000000000 ) ) ;
#36772 = EDGE_LOOP ( 'NONE', ( #29427, #10157, #30532, #7172 ) ) ;
#36773 = EDGE_LOOP ( 'NONE', ( #5303, #22474, #16298, #7727 ) ) ;
#36774 = CARTESIAN_POINT ( 'NONE',  ( -8.005635539500367770, 26.78432071055680908, -16.83492925294579123 ) ) ;
#36775 = CARTESIAN_POINT ( 'NONE',  ( -14.78469161520108699, 20.18088120075973535, 10.49999999999999467 ) ) ;
#36776 = CARTESIAN_POINT ( 'NONE',  ( -5.348113209407908464, 9.835177808069893501, 13.00000000000000178 ) ) ;
#36777 = DIRECTION ( 'NONE',  ( 0.9945218953682729568, -0.1045284632676570929, -0.000000000000000000 ) ) ;
#36778 = EDGE_LOOP ( 'NONE', ( #25920, #32548, #31244, #1247, #14945 ) ) ;
#36779 = CARTESIAN_POINT ( 'NONE',  ( 21.70875678425652566, 0.7301209385331313140, -23.85431322577691304 ) ) ;
#36780 = FACE_OUTER_BOUND ( 'NONE', #13418, .T. ) ;
#36781 = CARTESIAN_POINT ( 'NONE',  ( -14.52509594610762456, 21.97885917798744870, 11.00000000000000000 ) ) ;
#36782 = ORIENTED_EDGE ( 'NONE', *, *, #26900, .T. ) ;
#36783 = CARTESIAN_POINT ( 'NONE',  ( -30.71051382067356172, -0.01506129966919131369, -6.887934430901168525 ) ) ;
#36784 = DIRECTION ( 'NONE',  ( -1.000000000000000000, 0.000000000000000000, 0.000000000000000000 ) ) ;
#36785 = ORIENTED_EDGE ( 'NONE', *, *, #3168, .F. ) ;
#36786 = CARTESIAN_POINT ( 'NONE',  ( 33.01932729430679814, -6.854573688073132942, -10.30955742185432200 ) ) ;
#36787 = VERTEX_POINT ( 'NONE', #19474 ) ;
#36788 = CARTESIAN_POINT ( 'NONE',  ( 1.926143243141009931, 40.30103163374183595, 12.73282698324853435 ) ) ;
#36789 = CARTESIAN_POINT ( 'NONE',  ( -17.83459896180957927, -17.64923967996706367, 20.94377226548378346 ) ) ;
#36790 = CARTESIAN_POINT ( 'NONE',  ( -37.62663912510979003, -8.659558992827880886, -5.000000000000005329 ) ) ;
#36791 = CARTESIAN_POINT ( 'NONE',  ( -7.531283639252405848, 27.60866748444384555, 20.50957957746029692 ) ) ;
#36792 = VECTOR ( 'NONE', #31868, 1000.000000000000000 ) ;
#36793 = CARTESIAN_POINT ( 'NONE',  ( -3.503793317224520365, 8.420815634768723967, 11.00000000000000000 ) ) ;
#36794 = ORIENTED_EDGE ( 'NONE', *, *, #5319, .F. ) ;
#36795 = ADVANCED_FACE ( 'NONE', ( #22515 ), #13174, .F. ) ;
#36796 = FACE_OUTER_BOUND ( 'NONE', #11365, .T. ) ;
#36797 = CARTESIAN_POINT ( 'NONE',  ( 5.473344025737211460, 14.11593743010426394, 10.49999999999999822 ) ) ;
#36798 = AXIS2_PLACEMENT_3D ( 'NONE', #32033, #23090, #7443 ) ;
#36799 = AXIS2_PLACEMENT_3D ( 'NONE', #14572, #26962, #11923 ) ;
#36800 = CARTESIAN_POINT ( 'NONE',  ( 6.623974762475253186, 33.89653518476367111, -11.11648977816992812 ) ) ;
#36801 = CARTESIAN_POINT ( 'NONE',  ( -14.99905852611806445, 22.33194247983213643, 7.000000000000000000 ) ) ;
#36802 = EDGE_CURVE ( 'NONE', #9003, #39481, #28021, .T. ) ;
#36803 = CARTESIAN_POINT ( 'NONE',  ( 2.036571916123615100, 8.108948098542045457, 10.49999999999999467 ) ) ;
#36804 = EDGE_CURVE ( 'NONE', #21291, #30744, #14434, .T. ) ;
#36805 = CARTESIAN_POINT ( 'NONE',  ( 13.76863925707710301, -20.58511431638807210, -19.22791859126990488 ) ) ;
#36806 = CARTESIAN_POINT ( 'NONE',  ( -9.705584749708384251, 11.06314620770957013, 7.221809905720049549 ) ) ;
#36807 = CARTESIAN_POINT ( 'NONE',  ( -3.161220354320354531, 12.43736188311282653, 10.50000000000000000 ) ) ;
#36808 = CARTESIAN_POINT ( 'NONE',  ( 10.21799113078985677, 32.82168114676792925, 10.66666666666666430 ) ) ;
#36809 = VERTEX_POINT ( 'NONE', #9742 ) ;
#36810 = VERTEX_POINT ( 'NONE', #7076 ) ;
#36811 = CARTESIAN_POINT ( 'NONE',  ( -15.24185242054940836, 26.37366825853258945, -7.827947956013988851 ) ) ;
#36812 = CARTESIAN_POINT ( 'NONE',  ( -26.16909114927327451, -23.33537003677659527, 18.42518152272073095 ) ) ;
#36813 = CARTESIAN_POINT ( 'NONE',  ( 12.22774578270097656, -22.02461334279974636, -17.44299809173021387 ) ) ;
#36814 = CARTESIAN_POINT ( 'NONE',  ( 3.607749162633204332, 7.931741834401770497, 10.49999999999999822 ) ) ;
#36815 = ORIENTED_EDGE ( 'NONE', *, *, #36498, .T. ) ;
#36816 = ORIENTED_EDGE ( 'NONE', *, *, #27719, .T. ) ;
#36818 = CARTESIAN_POINT ( 'NONE',  ( 13.57128027507778789, 27.95460132399998443, 10.49999999999999822 ) ) ;
#36817 = CARTESIAN_POINT ( 'NONE',  ( -10.27241934331446416, 20.16311048434034348, -22.50241456494288173 ) ) ;
#36819 = CARTESIAN_POINT ( 'NONE',  ( -11.05369788186578539, -17.27790053512912039, -30.00000000000000711 ) ) ;
#36820 = DIRECTION ( 'NONE',  ( -0.000000000000000000, -0.000000000000000000, -1.000000000000000000 ) ) ;
#36821 = VECTOR ( 'NONE', #29335, 1000.000000000000000 ) ;
#36822 = VERTEX_POINT ( 'NONE', #197 ) ;
#36823 = CARTESIAN_POINT ( 'NONE',  ( -25.03491786389344043, -8.622393956815280092, -18.71499684687251630 ) ) ;
#36824 = CARTESIAN_POINT ( 'NONE',  ( -13.87499679755532078, -24.58662948498892220, -12.55662072122034800 ) ) ;
#36825 = CARTESIAN_POINT ( 'NONE',  ( 33.75875814100314187, 2.759858869446414786, 11.00000000000000000 ) ) ;
#36826 = EDGE_LOOP ( 'NONE', ( #36117, #30848, #4770, #30148 ) ) ;
#36827 = CARTESIAN_POINT ( 'NONE',  ( 21.14671899331803928, 1.666164666168168385, -25.10787130110661991 ) ) ;
#36828 = DIRECTION ( 'NONE',  ( 1.000000000000000000, 0.000000000000000000, 0.000000000000000000 ) ) ;
#36829 = CARTESIAN_POINT ( 'NONE',  ( 23.05386822411318803, -7.747535282638377652, 23.00000000000000000 ) ) ;
#36830 = EDGE_CURVE ( 'NONE', #35424, #880, #18956, .T. ) ;
#36831 = AXIS2_PLACEMENT_3D ( 'NONE', #4764, #17968, #36049 ) ;
#36832 = VERTEX_POINT ( 'NONE', #791 ) ;
#36833 = CARTESIAN_POINT ( 'NONE',  ( -30.79303797620794114, -0.1002779665139238718, -6.885808881345242050 ) ) ;
#36834 = ORIENTED_EDGE ( 'NONE', *, *, #35969, .F. ) ;
#36835 = CARTESIAN_POINT ( 'NONE',  ( 30.12800540966269125, -0.8552404287211460288, -10.58273019797263714 ) ) ;
#36836 = AXIS2_PLACEMENT_3D ( 'NONE', #4803, #26336, #29584 ) ;
#36837 = CARTESIAN_POINT ( 'NONE',  ( 27.44755207257203367, -22.53416897284666121, 18.42518152272072385 ) ) ;
#36838 = ORIENTED_EDGE ( 'NONE', *, *, #18485, .T. ) ;
#36839 = CARTESIAN_POINT ( 'NONE',  ( -20.91675722910995816, 2.871490340677382402, -25.21439981239640815 ) ) ;
#36840 = CARTESIAN_POINT ( 'NONE',  ( -8.910254037844422825, 17.93301270189230223, 10.49999999999999822 ) ) ;
#36841 = DIRECTION ( 'NONE',  ( 1.000000000000000000, 0.000000000000000000, 0.000000000000000000 ) ) ;
#36842 = CARTESIAN_POINT ( 'NONE',  ( -2.525645716490712012, 8.212903943950955465, 11.00000000000000000 ) ) ;
#36843 = DIRECTION ( 'NONE',  ( 1.000000000000000000, 0.000000000000000000, 0.000000000000000000 ) ) ;
#36844 = AXIS2_PLACEMENT_3D ( 'NONE', #6512, #235, #27863 ) ;
#36845 = EDGE_CURVE ( 'NONE', #36810, #5091, #25176, .T. ) ;
#36846 = AXIS2_PLACEMENT_3D ( 'NONE', #20148, #10194, #38227 ) ;
#36847 = CIRCLE ( 'NONE', #33656, 6.000000000000005329 ) ;
#36848 = CARTESIAN_POINT ( 'NONE',  ( 0.000000000000000000, 22.50000000000000355, 7.000000000000000000 ) ) ;
#36849 = CARTESIAN_POINT ( 'NONE',  ( -17.05532387642082526, 7.816133769664412867, 11.00000000000000000 ) ) ;
#36850 = ORIENTED_EDGE ( 'NONE', *, *, #24010, .F. ) ;
#36851 = CARTESIAN_POINT ( 'NONE',  ( -24.85289228938016493, 7.121634862230863838, -5.479396508039022784 ) ) ;
#36852 = PLANE ( 'NONE',  #28809 ) ;
#36853 = EDGE_CURVE ( 'NONE', #16522, #3856, #31869, .T. ) ;
#36854 = DIRECTION ( 'NONE',  ( -0.8090169943749504489, -0.5877852522924691403, 0.000000000000000000 ) ) ;
#36855 = CARTESIAN_POINT ( 'NONE',  ( 21.93136298064665723, -25.57125421755331729, -9.878379079991990608 ) ) ;
#36856 = CIRCLE ( 'NONE', #6991, 0.4999999999999995559 ) ;
#36857 = CARTESIAN_POINT ( 'NONE',  ( -5.953812613386785912, 14.77701242934787906, 13.00000000000000178 ) ) ;
#36858 = CARTESIAN_POINT ( 'NONE',  ( 11.28378745254010695, 18.60854979943831111, -23.82222365283083576 ) ) ;
#36859 = CIRCLE ( 'NONE', #6992, 0.5000000000000004441 ) ;
#36860 = CARTESIAN_POINT ( 'NONE',  ( -15.20016916873736079, -27.86040092368267551, 14.53008259254011136 ) ) ;
#36861 = VERTEX_POINT ( 'NONE', #13379 ) ;
#36862 = CARTESIAN_POINT ( 'NONE',  ( -16.18186380107325917, 24.02863330739335623, -6.421819638462467061 ) ) ;
#36863 = CARTESIAN_POINT ( 'NONE',  ( -19.22069824708770014, -18.72532366025136596, 20.82122704794093337 ) ) ;
#36864 = DIRECTION ( 'NONE',  ( 0.000000000000000000, 0.000000000000000000, 1.000000000000000000 ) ) ;
#36865 = CARTESIAN_POINT ( 'NONE',  ( 14.85533356076911637, 25.56315567979834213, -10.18121021804152448 ) ) ;
#36866 = ORIENTED_EDGE ( 'NONE', *, *, #25538, .T. ) ;
#36867 = DIRECTION ( 'NONE',  ( -0.000000000000000000, -0.000000000000000000, -1.000000000000000000 ) ) ;
#36868 = EDGE_LOOP ( 'NONE', ( #17768, #35675, #33527, #15324 ) ) ;
#36870 = CARTESIAN_POINT ( 'NONE',  ( -0.5000000000000004441, 37.00000000000000711, 7.000000000000000000 ) ) ;
#36869 = CARTESIAN_POINT ( 'NONE',  ( -10.92279190285937140, 17.50161691125836327, -28.07041777319187048 ) ) ;
#36871 = CARTESIAN_POINT ( 'NONE',  ( -14.76270255855745894, -25.48967811294425800, -10.64446229900349650 ) ) ;
#36872 = LINE ( 'NONE', #9043, #21739 ) ;
#36873 = CARTESIAN_POINT ( 'NONE',  ( -19.19651427957619561, -10.81311144643282773, -24.21601489736221779 ) ) ;
#36874 = CARTESIAN_POINT ( 'NONE',  ( -10.17830574738310823, -20.64784012530623158, -20.65330454052350007 ) ) ;
#36875 = CARTESIAN_POINT ( 'NONE',  ( -14.64659974985906210, 21.96608861361228904, 10.49999999999999822 ) ) ;
#36876 = CARTESIAN_POINT ( 'NONE',  ( 13.87278661928481860, 20.14957414006898873, -17.58567953334315703 ) ) ;
#36877 = EDGE_LOOP ( 'NONE', ( #6378, #6166 ) ) ;
#36878 = CARTESIAN_POINT ( 'NONE',  ( 19.81143946857858040, 6.663503521798424423, -25.44058611693839467 ) ) ;
#36879 = DIRECTION ( 'NONE',  ( 1.000000000000000000, 0.000000000000000000, 0.000000000000000000 ) ) ;
#36880 = EDGE_CURVE ( 'NONE', #32024, #659, #17678, .T. ) ;
#36881 = CARTESIAN_POINT ( 'NONE',  ( -11.44473057578096942, 31.45924896672619298, 10.49999999999999822 ) ) ;
#36882 = EDGE_CURVE ( 'NONE', #10398, #16279, #9545, .T. ) ;
#36883 = PLANE ( 'NONE',  #14800 ) ;
#36884 = ORIENTED_EDGE ( 'NONE', *, *, #5871, .T. ) ;
#36885 = CARTESIAN_POINT ( 'NONE',  ( -21.39596226364862375, -0.2386576062743040183, -24.90343605780445557 ) ) ;
#36887 = CARTESIAN_POINT ( 'NONE',  ( 22.74759679801531220, 0.5550921298590332231, -21.60981102281446553 ) ) ;
#36886 = TOROIDAL_SURFACE ( 'NONE', #20038, 1.000000000000000000, 0.5000000000000000000 ) ;
#36888 = AXIS2_PLACEMENT_3D ( 'NONE', #32392, #13077, #1105 ) ;
#36889 = FACE_OUTER_BOUND ( 'NONE', #2094, .T. ) ;
#36890 = CARTESIAN_POINT ( 'NONE',  ( 27.79678266235291773, -11.09703717633714426, 20.69868183039781329 ) ) ;
#36891 = EDGE_LOOP ( 'NONE', ( #13220, #40020, #1030, #39372, #18251 ) ) ;
#36892 = CIRCLE ( 'NONE', #10943, 1.000000000000000000 ) ;
#36893 = CARTESIAN_POINT ( 'NONE',  ( 22.40982762235196901, 2.618079236896951656, -30.00000000000000355 ) ) ;
#36895 = CIRCLE ( 'NONE', #16118, 0.9999999999999991118 ) ;
#36894 = DIRECTION ( 'NONE',  ( 0.000000000000000000, 0.000000000000000000, 1.000000000000000000 ) ) ;
#36896 = ORIENTED_EDGE ( 'NONE', *, *, #20284, .T. ) ;
#36897 = DIRECTION ( 'NONE',  ( 1.000000000000000000, 0.000000000000000000, 0.000000000000000000 ) ) ;
#36898 = ADVANCED_FACE ( 'NONE', ( #21922 ), #10009, .T. ) ;
#36899 = CARTESIAN_POINT ( 'NONE',  ( -0.6417741116369681809, 11.68927977431952137, 13.00000000000000178 ) ) ;
#36900 = DIRECTION ( 'NONE',  ( 1.000000000000000000, 0.000000000000000000, 0.000000000000000000 ) ) ;
#36901 = CARTESIAN_POINT ( 'NONE',  ( 2.741814962476898820, 38.30556977738701363, -5.000000000000001776 ) ) ;
#36902 = DIRECTION ( 'NONE',  ( 1.000000000000000000, 0.000000000000000000, 0.000000000000000000 ) ) ;
#36903 = LINE ( 'NONE', #27754, #22732 ) ;
#36904 = CARTESIAN_POINT ( 'NONE',  ( 14.04642159563909942, 39.70023260537602994, 10.00000000000000000 ) ) ;
#36905 = DIRECTION ( 'NONE',  ( -1.000000000000000000, 0.000000000000000000, 0.000000000000000000 ) ) ;
#36906 = DIRECTION ( 'NONE',  ( 0.000000000000000000, 0.000000000000000000, 1.000000000000000000 ) ) ;
#36907 = CARTESIAN_POINT ( 'NONE',  ( 14.46080647158823318, 26.53523365061236561, 10.49999999999999645 ) ) ;
#36908 = CIRCLE ( 'NONE', #19384, 57.00000000000003553 ) ;
#36909 = CARTESIAN_POINT ( 'NONE',  ( 15.07870883215744762, 27.77416456386047727, -5.935715514897943024 ) ) ;
#36910 = DIRECTION ( 'NONE',  ( 0.000000000000000000, 0.000000000000000000, 1.000000000000000000 ) ) ;
#36911 = AXIS2_PLACEMENT_3D ( 'NONE', #38626, #20147, #32546 ) ;
#36912 = ORIENTED_EDGE ( 'NONE', *, *, #21061, .F. ) ;
#36914 = CYLINDRICAL_SURFACE ( 'NONE', #30455, 1.000000000000000888 ) ;
#36913 = CARTESIAN_POINT ( 'NONE',  ( -15.82159548417086725, 15.31645673244926442, -21.04376448643831665 ) ) ;
#36915 = AXIS2_PLACEMENT_3D ( 'NONE', #21791, #267, #38033 ) ;
#36916 = DIRECTION ( 'NONE',  ( 1.533293416683372906E-16, -0.7071067811865474617, -0.7071067811865474617 ) ) ;
#36917 = CARTESIAN_POINT ( 'NONE',  ( 14.60635565259179991, -25.45748058625455457, -10.65361818253279935 ) ) ;
#36918 = CARTESIAN_POINT ( 'NONE',  ( -12.40276988179543771, -16.90054568133930957, -26.59307398819964519 ) ) ;
#36919 = DIRECTION ( 'NONE',  ( 0.000000000000000000, 0.000000000000000000, 1.000000000000000000 ) ) ;
#36920 = CARTESIAN_POINT ( 'NONE',  ( 14.28350017971037111, 24.49113824962887520, -12.54891074749486712 ) ) ;
#36921 = CIRCLE ( 'NONE', #1892, 1.000000000000000888 ) ;
#36922 = B_SPLINE_SURFACE_WITH_KNOTS ( 'NONE', 3, 3, ( 
 ( #11537, #6029, #36518, #9284, #12329, #2595, #27569, #30227, #12132, #18433, #30824, #33489, #31022, #2396, #14785, #8689, #27767, #23926, #5629, #18039, #39757, #11935, #36323, #6813, #15774, #13314, #25314, #16579, #22656, #31809, #3580, #37313, #22460, #21865 ),
 ( #25116, #28164, #34270, #340, #12724, #19415, #35061, #22067, #3381, #19616, #936, #9488, #4176, #34467, #22257, #32010, #25710, #28359, #6615, #10275, #16177, #37513, #6424, #7216, #34661, #3975, #12921, #38104, #31217, #28562, #9690, #138, #737, #12528 ),
 ( #24919, #15978, #16375, #13115, #19022, #25504, #31414, #537, #19217, #28761, #37712, #10077, #9876, #31606, #18829, #3776, #34865, #37905, #7014, #23473, #33037, #8028, #36070, #29567, #4379, #20030, #8232, #38507, #14328, #17192, #35869, #16783, #26721, #38713 ),
 ( #23065, #25907, #10891, #29771, #13519, #29169, #20435, #35263, #5186, #1336, #13720, #32631, #39107, #1747, #10682, #32831, #26110, #11090, #14126, #4987, #7624, #17398, #1953, #20638, #35469, #11293, #26525, #26319, #32426, #20234, #10478, #19827, #23673, #28962 ),
 ( #4585, #1138, #38306, #32216, #16986, #22859, #7417, #29364, #4785, #1541, #13925, #23274, #35672, #7826, #38913, #21029, #17799, #12077, #30774, #30578, #2934, #24074, #14733, #24667, #27123, #5975, #33636, #36467, #26923, #24273, #27710, #39308, #18382, #8439 ),
 ( #9036, #29966, #8636, #11882, #33438, #40102, #33237, #21420, #5578, #34021, #17991, #36865, #2737, #12278, #33827, #37061, #15323, #39901, #15128, #36667, #27517, #17597, #8837, #9231, #14932, #11488, #5384, #30379, #2544, #24467, #21616, #30173, #21224, #2146 ),
 ( #27320, #14529, #11687, #23873, #39708, #36276, #20835, #2348, #39509, #5783, #18186, #6370, #21813, #9826, #16321, #34609, #15722, #37849, #34216, #28507, #31555, #25449, #25065, #679, #6956, #13263, #18775, #19363, #3721, #3527, #31165, #37657, #27912, #37260 ),
 ( #9635, #31361, #3330, #6564, #28110, #6762, #10222, #22205, #19163, #16124, #13059, #12472, #15924, #12869, #288, #10024, #38052, #22403, #34805, #25655, #31761, #12671, #37461, #22608, #22015, #3923, #28706, #884, #34413, #6177, #28307, #487, #18578, #18971 ),
 ( #25261, #30965, #3132, #15529, #89, #9434, #24866, #4735, #7167, #39059, #20181, #10426, #7974, #35818, #13668, #32376, #28910, #13879, #17142, #32577, #20386, #22810, #23425, #38458, #35015, #14278, #10631, #31954, #1488, #4940, #38257, #23013, #19978, #19772 ),
 ( #26268, #16527, #1088, #32166, #35207, #29520, #38661, #7366, #32781, #4533, #11237, #17344, #26468, #35415, #4122, #1695, #13466, #7573, #29720, #1901, #25856, #1286, #26669, #4327, #11041, #10834, #19565, #16732, #29115, #26058, #16934, #29318, #23225, #35621 ),
 ( #7778, #14071, #38865, #39660, #39260, #17544, #34322, #17942, #28019, #36418, #9542, #14478, #11833, #23822, #21920, #24222, #6476, #15633, #36024, #30124, #30325, #14684, #18880, #11439, #194, #2298, #396, #27073, #3241, #8790, #31271, #12581, #3434, #24973 ),
 ( #39460, #18141, #28216, #36228, #37366, #11642, #23626, #24024, #15832, #21178, #8182, #20589, #32986, #5138, #5733, #33581, #2497, #30531, #29918, #14885, #2098, #20980, #26871, #8391, #8583, #33388, #20787, #33184, #5335, #27274, #17748, #5531, #36619, #31669 ),
 ( #9738, #34922, #13576, #37568, #28416, #4236, #19077, #29224, #12974, #591, #16430, #22918, #995, #22318, #16639, #25363, #35118, #38163, #32067, #3834, #7271, #25962, #19884, #37765, #38363, #10333, #10135, #9936, #4029, #34520, #3633, #34717, #32276, #22121 ),
 ( #13170, #6870, #13376, #16842, #28820, #25765, #22714, #19673, #31469, #22512, #19471, #19270, #29022, #4440, #1196, #10535, #7477, #12777, #25172, #25565, #16234, #28617, #6670, #787, #37964, #35319, #16030, #7073, #31865, #20892, #2206, #38565, #5447, #35730 ),
 ( #36129, #14592, #14388, #26981, #7881, #38768, #8493, #10949, #30030, #17453, #20288, #10738, #8085, #11546, #23123, #39367, #32485, #33091, #35524, #7688, #23933, #17250, #5244, #29824, #23334, #20697, #32686, #8292, #36329, #33294, #13982, #17855, #39165, #38970 ),
 ( #20089, #20494, #1393, #4641, #4841, #26579, #26373, #1801, #17044, #2009, #13779, #26775, #32888, #11348, #23730, #29424, #11144, #5042, #29623, #17656, #26171, #1600, #14184, #23530, #35927, #2403, #30638, #14989, #18048, #24129, #30441, #2603, #9295, #24929 ),
 ( #11943, #27183, #21873, #3199, #27376, #33694, #39765, #24725, #15588, #2999, #27973, #36731, #24334, #37324, #8895, #18641, #6039, #21285, #39568, #36929, #148, #11744, #31032, #21089, #21679, #36525, #8697, #12537, #5843, #34080, #18443, #18245, #15387, #2796 ),
 ( #15188, #6239, #27779, #9497, #34280, #6434, #30234, #12337, #40166, #9095, #37125, #14793, #21480, #33497, #27579, #5636, #39964, #12141, #24531, #33886, #30833, #34476, #10089, #6624, #15986, #34874, #22870, #12931, #15784, #746, #19627, #3390, #19032, #10286 ),
 ( #31424, #3591, #22469, #28973, #7025, #28367, #22668, #547, #948, #3985, #351, #28174, #4188, #34672, #35072, #19427, #25322, #31820, #37721, #9887, #13124, #7226, #22267, #28773, #6825, #19226, #25919, #37917, #13328, #1148, #31616, #25720, #35274, #38114 ),
 ( #12732, #3786, #16188, #28572, #32023, #13531, #25515, #16387, #16591, #38316, #10488, #18838, #25124, #31226, #37523, #9700, #22076, #8243, #32227, #39118, #38518, #2158, #17408, #19839, #11499, #32844, #23080, #20649, #33050, #26331, #4796, #1347, #26536, #29784 ),
 ( #14541, #20042, #5200, #4997, #17202, #32437, #38924, #29181, #10693, #16996, #26935, #16795, #13730, #4390, #11304, #11100, #26122, #35479, #4596, #7635, #1964, #14138, #29375, #17609, #32642, #23884, #29978, #23684, #10901, #1552, #14340, #13935, #23287, #39322 ),
 ( #38725, #36083, #35682, #7430, #23483, #7836, #20244, #29579, #1757, #35880, #8038, #20446, #26732, #30786, #9242, #9049, #21629, #2557, #33450, #3145, #5592, #24679, #12091, #14944, #5397, #2748, #6190, #17811, #37073, #27134, #27725, #24086, #30186, #36480 ),
 ( #12290, #24480, #34034, #18003, #33248, #27925, #18595, #30390, #39720, #8648, #2949, #30979, #21432, #15541, #27332, #11896, #102, #24285, #12484, #36876, #36680, #2361, #15141, #36288, #14745, #8451, #39522, #40113, #11699, #21041, #20849, #8850, #21236, #33838 ),
 ( #33647, #5796, #18198, #30591, #15336, #5986, #27532, #39913, #18394, #13276, #6972, #10037, #31569, #22416, #24878, #3735, #25668, #22217, #18789, #12683, #501, #3539, #19376, #7181, #301, #16137, #12881, #18983, #25277, #9650, #34231, #19579, #21826, #37670 ),
 ( #25078, #16338, #31177, #1101, #37474, #22028, #28521, #35029, #13073, #34427, #28720, #6577, #31775, #34820, #3937, #15937, #899, #38066, #31971, #31374, #10236, #22622, #34621, #28320, #696, #6382, #15734, #9839, #4136, #3342, #28123, #6774, #16541, #25464 ),
 ( #19175, #37864, #28923, #37273, #9447, #7987, #16947, #26683, #4952, #26484, #19993, #38272, #29532, #22825, #7588, #20400, #4749, #38878, #23028, #1707, #35830, #29734, #1300, #32794, #17156, #29331, #13683, #10848, #35221, #32180, #26071, #17358, #7382, #19785 ),
 ( #4342, #7791, #14291, #35633, #23240, #14087, #20194, #16747, #1501, #26280, #38472, #32590, #1913, #11054, #13481, #25869, #10440, #29128, #23438, #10645, #38675, #13892, #35428, #32389, #4546, #4267, #31504, #12812, #29053, #10370, #6507, #13610, #3670, #31701 ),
 ( #22747, #22547, #35151, #16062, #6704, #16671, #19112, #38199, #25598, #28451, #18913, #16266, #19710, #31304, #7305, #430, #1028, #3472, #15867, #32103, #25397, #13408, #37997, #626, #34958, #34553, #37605, #3868, #1231, #13008, #19506, #37793, #9968, #25999 ),
 ( #7108, #28650, #31898, #9575, #823, #21956, #6903, #28256, #9774, #22347, #34753, #4062, #34359, #25207, #13203, #19307, #10171, #16468, #28851, #22151, #25803, #35356, #10977, #1838, #39199, #22953, #29854, #29257, #33120, #8116, #10570, #2235, #23565, #13809 ),
 ( #26203, #20523, #11378, #4673, #35555, #5273, #7718, #26809, #14216, #17077, #7511, #4869, #8328, #19914, #23761, #1428, #2038, #32312, #4473, #36157, #14014, #14416, #26606, #20120, #11174, #23156, #38597, #32718, #20729, #32521, #32918, #29452, #1632, #17685 ),
 ( #35960, #17284, #5076, #38396, #29655, #30061, #35760, #16877, #10771, #26402, #38801, #17483, #14623, #23365, #39000, #7916, #20320, #27407, #11773, #36359, #9327, #23964, #39795, #30667, #27810, #11575, #18473, #17883, #21709, #36959, #39394, #31063, #12169, #2432 ),
 ( #5666, #24362, #20917, #5872, #9124, #24565, #40195, #14823, #15416, #30469, #27012, #6268, #2629, #8522, #33725, #37154, #30265, #15017, #11971, #24158, #36759, #27210, #27607, #3227, #2828, #18275, #21511, #39992, #33322, #8927, #15220, #39599, #33914, #18669 ),
 ( #34112, #5470, #36554, #21319, #8725, #21117, #33525, #18078, #6069, #30864, #3026, #12367, #24755, #16641, #14390, #35928, #19885, #26172, #22919, #17251, #8086, #35731, #26776, #1802, #29825, #23336, #38364, #13780, #2010, #32278, #20495, #10950, #29624, #35320 ),
 ( #23124, #7478, #32068, #5043, #19674, #35525, #26374, #23531, #7272, #14185, #13577, #17454, #32687, #35119, #39166, #7882, #10537, #32889, #22715, #1394, #20090, #29023, #1601, #4842, #20289, #4237, #4441, #11145, #38566, #1197, #25963, #10739, #16843, #29425 ),
 ( #29225, #7690, #32486, #4642, #26580, #13983, #17045, #38769, #38972, #11547, #8896, #18049, #26982, #24532, #36526, #27781, #33887, #2797, #14794, #8293, #33695, #33092, #27184, #36930, #21481, #2207, #17856, #39965, #5245, #27580, #8698, #12143, #20893, #17657 ),
 ( #15388, #5449, #33498, #3000, #9096, #39569, #30235, #6040, #27377, #39368, #30032, #18444, #5637, #15189, #24130, #30834, #14593, #39766, #23934, #11349, #11944, #23731, #36130, #20698, #2404, #30442, #11745, #36330, #8494, #33295, #21091, #2604, #14990, #30639 ),
 ( #24335, #36733, #21286, #5844, #18246, #22471, #6435, #34674, #16389, #12338, #353, #24931, #27974, #34081, #149, #12538, #19228, #34876, #15589, #7028, #19429, #34281, #37126, #3987, #18840, #22078, #31822, #748, #28175, #31227, #10091, #15989, #37325, #6240 ),
 ( #28369, #3391, #9296, #6626, #40167, #21681, #13126, #31033, #31619, #18642, #3201, #25518, #15785, #3788, #549, #9498, #12933, #21874, #12733, #34479, #28574, #25125, #9890, #37525, #9702, #24726, #19034, #6827, #31426, #3593, #16190, #25324, #37919, #37723 ),
 ( #22269, #4392, #7432, #23290, #11102, #4190, #20044, #16797, #22872, #29183, #13533, #38116, #23485, #25722, #1349, #32439, #29581, #13330, #20246, #19629, #35882, #38727, #951, #32846, #13937, #16594, #1759, #14140, #19841, #26124, #22671, #7638, #10903, #26333 ),
 ( #17204, #32230, #28775, #8040, #13733, #10288, #35481, #38927, #32025, #38520, #10695, #25921, #23082, #28975, #29378, #4999, #4598, #16998, #35684, #1554, #35074, #7838, #32644, #1150, #4799, #20449, #26538, #7228, #38319, #10490, #35276, #9051, #5594, #2750 ),
 ( #39120, #20851, #15143, #27534, #8245, #23886, #5798, #11306, #33649, #2363, #18201, #26937, #23686, #21434, #30593, #14543, #33250, #17611, #11898, #39915, #30392, #12094, #36290, #39324, #24482, #11502, #36878, #33452, #8453, #26734, #24088, #33841, #36086, #17410 ),
 ( #20651, #33052, #29786, #5400, #8852, #18005, #17813, #2560, #2160, #5202, #11701, #1966, #30188, #27334, #14747, #27137, #14343, #36482, #24287, #29981, #39524, #36683, #8650, #21238, #21044, #14946, #39722, #37275, #25466, #15543, #31571, #34429, #12883, #6192 ),
 ( #6384, #30981, #15338, #28523, #2951, #18792, #9652, #6776, #30788, #37672, #37075, #698, #15939, #18396, #10039, #31376, #21631, #19177, #3737, #24880, #3344, #40115, #25080, #28322, #3541, #16139, #34036, #34623, #9449, #5988, #37866, #21828, #27728, #12685 ),
 ( #13075, #12292, #24681, #9245, #9841, #37476, #18597, #3148, #27927, #104, #503, #22030, #12486, #22418, #31179, #34233, #25279, #15736, #28125, #303, #6579, #18985, #22219, #38880, #28925, #16749, #26486, #35635, #22827, #1104, #4751, #10647, #10238, #28722 ),
 ( #23030, #13483, #3939, #1302, #17158, #16340, #7793, #25670, #26282, #901, #13278, #20196, #10442, #38677, #35430, #31973, #7590, #19581, #22624, #29130, #23242, #4138, #4548, #25871, #16543, #1709, #13685, #29333, #29534, #38274, #1503, #11056, #13894, #14089 ),
 ( #35031, #35223, #7384, #10850, #34822, #7183, #26073, #19787, #32182, #4344, #38474, #38068, #6974, #31777, #19995, #32391, #32592, #19378, #16949, #14293, #18154, #33403, #35832, #27481, #8598, #39073, #36635, #24236, #2113, #20801, #17360, #2311, #5544, #20995 ),
 ( #11848, #26885, #23440, #2703, #39273, #20402, #30138, #33596, #26685, #11452, #8404, #8196, #23838, #11251, #24038, #39867, #39477, #14697, #17955, #36433, #29736, #33198, #27088, #36037, #11656, #15091, #30340, #8804, #30544, #7989, #32796, #36244, #20603, #23639 ),
 ( #4954, #2512, #14899, #5748, #29932, #27288, #1915, #39673, #33001, #21191, #5152, #14492, #17558, #5350, #17763, #254, #18937, #12242, #27678, #9196, #28075, #16089, #6140, #9000, #34182, #12837, #36827, #40065, #3495, #18345, #28474, #24632, #37026, #15687 ),
 ( #21582, #25230, #37628, #30934, #9399, #5942, #31132, #34382, #37423, #9796, #33984, #455, #15494, #12044, #31528, #27879, #21387, #18743, #22176, #15290, #52, #37228, #18544, #12437, #3099, #12641, #24434, #25030, #3295, #21981, #9599, #30737, #21777, #6532 ),
 ( #34576, #15892, #24831, #33794, #31325, #2900, #6334, #6726, #19135, #28278, #3691, #29282, #22370, #16901, #25825, #1451, #10192, #34776, #32544, #13836, #38019, #4089, #848, #35382, #26228, #13636, #38624, #7132, #22573, #7741, #34982, #10798, #16694, #19530 ),
 ( #31726, #29078, #13228, #23182, #1255, #35583, #32336, #13030, #31921, #35175, #16493, #20145, #16287, #4498, #28877, #17103, #1052, #19941, #26023, #4699, #649, #25421, #38423, #7538, #25620, #28673, #13431, #10596, #37818, #38225, #9990, #22773, #6925, #19331 ),
 ( #3889, #10394, #7331, #19737, #4294, #32130, #22978, #39021, #20941, #4900, #11603, #14647, #8546, #8142, #23986, #30290, #36578, #1863, #2459, #27036, #26832, #14240, #20753, #11004, #20348, #11199, #8750, #38825, #23389, #26429, #33349, #8351, #35784, #7938 ),
 ( #39418, #2257, #32742, #39223, #36184, #26631, #17709, #21140, #30084, #14846, #24183, #5693, #1657, #29877, #23590, #17307, #29681, #35986, #20549, #5491, #33547, #32942, #29480, #14038, #5100, #17508, #2061, #14437, #11402, #23784, #27234, #33144, #5297, #39620 ),
 ( #36383, #11797, #17906, #21929, #30885, #3448, #8950, #34137, #18298, #15843, #6288, #28228, #9553, #30492, #24587, #12391, #9147, #409, #33749, #34334, #36982, #34530, #21532, #37377, #3252, #12788, #6486, #25184, #18891, #204, #15643, #24779, #28030, #18104 ),
 ( #37580, #18693, #5893, #33934, #9749, #27630, #22131, #12192, #8, #2653, #31282, #6091, #18496, #15039, #31086, #30688, #11993, #27432, #37177, #39818, #3048, #24386, #21343, #12592, #2853, #36779, #24983, #15241, #40014, #15440, #27833, #9350, #21729, #29234 ),
 ( #31677, #34729, #1005, #35330, #3844, #16650, #37973, #16245, #14350, #25779, #1208, #1973, #13180, #13586, #11312, #25973, #26741, #7282, #22326, #10148, #39128, #28627, #32289, #35128, #38374, #6880, #19281, #796, #22724, #23694, #25575, #3645, #28829, #7489 ),
 ( #31479, #10546, #37773, #6681, #29032, #19089, #16040, #32078, #22521, #19895, #4450, #34931, #4037, #604, #38173, #22932, #4246, #16856, #7082, #28425, #19480, #12984, #25373, #31877, #9945, #13386, #16441, #10344, #19683, #21051, #20858, #36489, #11509, #36691 ),
 ( #33258, #36297, #33655, #2568, #23893, #9058, #33459, #12301, #18403, #27541, #39531, #33059, #18208, #17619, #11707, #21442, #5996, #26944, #2370, #24488, #29989, #12102, #5603, #36887, #5407, #2167, #27735, #33849, #36094, #8459, #17820, #39729, #30796, #24295 ),
 ( #2958, #14754, #18011, #14551, #14952, #30600, #21246, #15346, #30196, #40122, #24095, #8251, #20659, #8658, #5208, #27341, #39332, #27145, #30401, #11905, #8859, #5806, #2757, #15150, #39923, #509, #15947, #34631, #37679, #30988, #22038, #31382, #37282, #12892 ),
 ( #28132, #21638, #6783, #6199, #311, #10048, #34830, #15549, #31185, #13083, #18604, #704, #9660, #25473, #34239, #3156, #16345, #37872, #21836, #12692, #24887, #19186, #22424, #9849, #6980, #3352, #6392, #31783, #18800, #19385, #25286, #15743, #34042, #3549 ),
 ( #9456, #3946, #22226, #28727, #16146, #37084, #25087, #18993, #37484, #907, #110, #28532, #34436, #24687, #6587, #3743, #31577, #9253, #27935, #12494, #28329, #35641, #38683, #20000, #10856, #13284, #32399, #1718, #10654, #7188, #1111, #29136, #32188, #7801 ),
 ( #13488, #28930, #10448, #29338, #17368, #7389, #10244, #35437, #14095, #38073, #25878, #4757, #19588, #22629, #17164, #4144, #7996, #23247, #25678, #29741, #20201, #38280, #26492, #38886, #4349, #23036, #31979, #4554, #32598, #29540, #11062, #22832, #23446, #16756 ),
 ( #35231, #16955, #35037, #16550, #19794, #20407, #1309, #13690, #26079, #35837, #1509, #38480, #7595, #13899, #26290, #32803, #4960, #17565, #15100, #27095, #18351, #24440, #33603, #5356, #39080, #24244, #23645, #17769, #27488, #12050, #33009, #8413, #30552, #36043 ),
 ( #29937, #9006, #21394, #36249, #11257, #5949, #20807, #24048, #33801, #2709, #30146, #33205, #36835, #17961, #2118, #8204, #1921, #36439, #5755, #14705, #39874, #5157, #30349, #14499, #14300, #2518, #26690, #18160, #20609, #2317, #8606, #39484, #26890, #39280 ),
 ( #11458, #21002, #23845, #11662, #11854, #33409, #5552, #14906, #27295, #36641, #39682, #8810, #21199, #34783, #9803, #37824, #31331, #6149, #21785, #9997, #59, #16096, #18944, #37635, #30941, #18550, #27886, #6539, #6933, #24837, #27684, #12648, #31534, #15297 ),
 ( #3106, #3698, #28482, #9405, #28082, #24638, #9606, #12846, #15898, #655, #15500, #19142, #34188, #30746, #22376, #6342, #40072, #37431, #13038, #33990, #18750, #15693, #12444, #31138, #37235, #3502, #2906, #28285, #21988, #461, #25236, #37035, #260, #34388 ),
 ( #25427, #22182, #3303, #12249, #34583, #9204, #25036, #21588, #6734, #10199, #25833, #7749, #856, #35592, #4301, #20153, #28884, #13236, #11012, #32552, #16501, #22781, #19539, #13845, #4709, #32346, #17112, #38233, #1060, #26438, #13438, #29489, #35390, #10403 ),
 ( #22582, #7548, #31928, #1666, #19948, #14046, #10808, #31733, #35183, #13645, #7338, #38836, #34990, #23192, #19745, #35792, #32139, #38633, #4506, #23397, #19340, #3898, #16295, #1460, #16909, #26032, #29291, #28681, #38431, #25628, #16702, #38026, #7139, #29086 ),
 ( #4097, #1262, #10604, #22985, #26237, #8361, #32952, #17316, #30500, #4908, #20761, #11611, #8758, #32751, #39629, #39030, #2661, #17913, #20357, #12003, #24191, #33155, #36587, #17517, #1873, #39826, #21147, #5109, #11411, #8151, #2468, #33554, #20950, #5701 ),
 ( #23598, #14250, #18113, #2266, #11805, #5307, #15048, #11208, #23994, #20557, #27439, #36391, #24393, #7947, #29689, #14446, #14655, #39231, #26641, #35995, #29888, #26840, #2070, #23793, #27241, #33356, #36193, #17717, #30092, #27045, #30297, #5499, #39427, #14855 ),
 ( #8555, #3654, #37386, #12200, #27842, #16047, #6100, #22139, #24991, #3456, #36989, #24596, #33942, #12600, #613, #30894, #33757, #18702, #37591, #21351, #9156, #28238, #2861, #12992, #21541, #18504, #213, #6689, #9560, #3057, #417, #15448, #18898, #21938 ),
 ( #31290, #9758, #28434, #15, #34538, #34345, #34145, #12398, #28038, #18306, #27640, #24788, #36786, #5902, #30697, #15250, #12797, #15651, #40021, #37187, #9358, #21737, #6493, #3259, #6295, #19096, #31095, #8958, #31488, #25191, #15852, #22333, #7496, #6889 ),
 ( #10156, #13188, #19289, #25582, #37981, #4456, #25383, #4253, #13795, #22731, #31684, #22529, #1013, #4047, #19901, #7702, #806, #16656, #13394, #19489, #25786, #34939, #34737, #20105, #3855, #38181, #29038, #26188, #9953, #16863, #16252, #32502, #35338, #37781 ),
 ( #13595, #7092, #29242, #31885, #32295, #10555, #1412, #16451, #38582, #10755, #4659, #28836, #23143, #22938, #35138, #10355, #1214, #28636, #7289, #19692, #17060, #32087, #25981, #38381, #35540, #29437, #1615, #35745, #11158, #14198, #11560, #20711, #29639, #27193 ),
 ( #2221, #5650, #14607, #39583, #8710, #30453, #26387, #14404, #38985, #1818, #7899, #26594, #23548, #33307, #21100, #35943, #33509, #18061, #8099, #10962, #13998, #20508, #36144, #38785, #14806, #2024, #32906, #24141, #30046, #5058, #20304, #36538, #8313, #17866 ),
 ( #4854, #26996, #17467, #11756, #39382, #23350, #5458, #32702, #29840, #33107, #26792, #17266, #39182, #30247, #11362, #23745, #5258, #2416, #23947, #17671, #36344, #8506, #20903, #24941, #27986, #9309, #160, #37137, #31239, #39978, #12550, #33898, #12155, #9712 ),
 ( #37336, #21694, #9508, #2614, #34092, #3402, #40179, #36744, #30651, #18455, #21493, #21888, #25138, #18258, #6253, #30845, #36941, #3011, #27591, #11956, #37538, #39779, #15402, #18655, #15797, #27389, #34292, #33706, #22092, #6446, #15002, #6639, #18850, #2809 ),
 ( #15202, #28186, #363, #12744, #6054, #34490, #19046, #24346, #24547, #8911, #21300, #12350, #9108, #31048, #5856, #27793, #24738, #3212, #15602, #25335, #28385, #35288, #10301, #12944, #37735, #28586, #31634, #28987, #38129, #6838, #4407, #16398, #7654, #13746 ),
 ( #16810, #26136, #31438, #3604, #31833, #16200, #19239, #9903, #3802, #758, #10503, #38532, #13139, #10708, #23092, #25530, #561, #35494, #37931, #13341, #16000, #32243, #19439, #10101, #1363, #7239, #22481, #22284, #34685, #25733, #7446, #3998, #29194, #34888 ),
 ( #7040, #28788, #22882, #962, #22682, #35086, #19640, #19854, #32035, #4204, #16605, #1163, #13545, #25932, #38332, #14154, #23497, #20462, #13950, #35895, #1770, #7851, #26345, #4811, #4612, #29390, #38738, #8054, #17012, #1567, #32451, #38938, #32656, #10919 ),
 ( #17217, #26552, #29591, #23302, #20258, #11113, #35697, #32857, #20057, #4329, #1490, #10836, #32579, #28509, #16529, #886, #3925, #10026, #16323, #28708, #35417, #23227, #31763, #35623, #7780, #10224, #13061, #20183, #22610, #38259, #16126, #16936, #4124, #35017 ),
 ( #13265, #22405, #26270, #10428, #19980, #28912, #13881, #6958, #32168, #25657, #19365, #19567, #19774, #25451, #38663, #31956, #7575, #16734, #38054, #29117, #7169, #1090, #22813, #4535, #13468, #26060, #25858, #35209, #681, #7368, #10633, #37852, #1288, #23015 ),
 ( #34807, #13670, #38460, #32378, #29320, #14280, #30327, #33186, #11644, #4942, #20388, #1903, #20789, #8793, #39061, #1697, #26873, #5533, #29522, #32783, #36420, #11044, #21180, #17346, #29722, #8393, #14887, #5337, #26672, #8585, #11239, #27075, #30126, #36026 ),
 ( #17751, #23628, #8184, #39262, #33391, #20591, #14686, #32988, #5140, #11835, #23824, #39462, #27276, #17546, #24026, #4737, #20982, #24224, #2300, #29920, #2101, #36621, #14480, #2499, #17944, #39662, #11441, #36230, #17144, #14073, #26470, #38867, #23427, #35820 ),
 ( #7976, #18143, #25567, #24974, #28821, #3835, #5735, #38165, #19271, #9543, #7074, #34923, #12778, #31470, #28020, #12975, #16235, #31670, #19472, #21921, #22513, #37569, #33583, #13377, #9739, #31076, #592, #4030, #37367, #22122, #19078, #18882, #34522, #34323 ),
 ( #15634, #31272, #6477, #28618, #25364, #3435, #31866, #3634, #10334, #16431, #37965, #6671, #3243, #788, #195, #16031, #997, #25766, #15833, #397, #12582, #28217, #10136, #28417, #25173, #37766, #9938, #22319, #34718, #6871, #13171, #28549, #30467, #24563 ),
 ( #24361, #15016, #25491, #27406, #6267, #33913, #36758, #27209, #36958, #723, #39598, #13099, #8724, #21318, #21509, #11772, #3762, #33724, #39794, #9326, #33523, #40193, #3025, #37152, #8925, #12366, #18668, #37890, #2628, #31062, #15415, #15219, #11970, #9123 ),
 ( #10064, #21116, #5870, #2827, #18274, #30666, #5665, #18472, #22443, #6068, #30863, #27809, #24754, #24157, #27606, #21708, #39991, #34111, #34851, #16163, #17881, #30264, #2431, #14821, #12168, #36553, #18077, #924, #7204, #35050, #26309, #1736, #22644, #14114 ),
 ( #38903, #20220, #4162, #10465, #7408, #26512, #4774, #32619, #17181, #13507, #16567, #11079, #28947, #35659, #23055, #25896, #16363, #13707, #29557, #28746, #23463, #38089, #22848, #10672, #13300, #7000, #35251, #38702, #35455, #1126, #20018, #31999, #19606, #1326 ),
 ( #16974, #38294, #19813, #19402, #26097, #1528, #31797, #32205, #13915, #3962, #10876, #25696, #7612, #4365, #16773, #10264, #29156, #38496, #32415, #23265, #4572, #29352, #7817, #11677, #39891, #29956, #32820, #17788, #36659, #20424, #11279, #27311, #1939, #12069 ),
 ( #8017, #35855, #21020, #23664, #4976, #2134, #30164, #5775, #8220, #2337, #14317, #18176, #24065, #36060, #29762, #30568, #14723, #39700, #8429, #21214, #26709, #36459, #20627, #39097, #17387, #27111, #2535, #33028, #14518, #39500, #26911, #2728, #5176, #11873 ),
 ( #39299, #14922, #33429, #15119, #24262, #27508, #8828, #17979, #5570, #8625, #30369, #17584, #33624, #11476, #33225, #23862, #36266, #20825, #5373, #18963, #6752, #40093, #15712, #12464, #18571, #24856, #9222, #33818, #19156, #21412, #37252, #28101, #25254, #9026 ),
 ( #672, #24658, #12271, #279, #34600, #12664, #34012, #15916, #37053, #6556, #9627, #3519, #3124, #31350, #37649, #31548, #21607, #9819, #22007, #21805, #6170, #25056, #5966, #15315, #30956, #3712, #18371, #30766, #2927, #28300, #3322, #27701, #15521, #27904 ),
 ( #37451, #79, #34207, #31157, #9425, #34406, #16113, #476, #22196, #28499, #24457, #36855, #6360, #18768, #12860, #6948, #13254, #875, #32367, #7768, #28697, #20170, #32567, #7157, #10016, #10213, #29105, #17132, #19556, #22395, #35199, #13867, #37840, #25647 ),
 ( #3914, #4725, #23003, #25441, #29507, #38449, #38044, #26256, #38652, #31946, #10418, #19355, #32158, #35407, #10622, #10825, #22598, #1480, #16519, #13051, #34798, #28902, #31752, #19761, #23213, #16313, #1080, #38249, #35007, #13455, #4113, #13661, #25848, #1278 ),
 ( #7565, #4318, #22800, #35609, #7357, #16722, #26050, #4525, #19966, #16925, #29309, #23416, #5127, #27259, #11821, #32769, #8172, #30315, #35808, #17932, #26859, #2485, #11225, #7963, #33570, #14874, #39049, #17534, #2087, #21167, #39648, #24210, #36607, #20576 ),
 ( #23616, #8774, #17736, #32972, #11030, #8379, #5720, #20376, #18130, #4928, #29908, #5324, #17333, #1684, #14467, #33375, #30113, #36012, #14674, #26658, #29707, #36214, #14061, #39248, #11629, #11429, #23812, #26455, #20777, #36408, #38854, #33174, #8571, #1890 ),
 ( #2284, #14268, #27063, #39448, #24012, #20969, #5518, #5921, #21755, #18521, #18321, #37610, #9776, #24612, #27456, #34557, #37005, #12417, #434, #2878, #37206, #36805, #12816, #6315, #30716, #24411, #25209, #24808, #34362, #3077, #15869, #21366, #18721, #15269 ),
 ( #33959, #34163, #39844, #28258, #6117, #21960, #31111, #27658, #3275, #40042, #12221, #9376, #18918, #9175, #233, #21561, #30914, #22156, #15668, #25007, #6707, #15467, #37404, #30519, #9578, #2679, #28054, #27859, #30, #15067, #12619, #12020, #6510, #31306 ),
 ( #3475, #8976, #33772, #28454, #1433, #16066, #31903, #22752, #19922, #3674, #10577, #9972, #13815, #29060, #31507, #23163, #4273, #34756, #32318, #4479, #38000, #16473, #13013, #38204, #1236, #16678, #16883, #6907, #7516, #22551, #19115, #38602, #34961, #630 ),
 ( #28656, #26210, #25402, #37799, #22350, #22959, #10376, #19311, #31704, #16269, #3872, #13616, #25809, #828, #29262, #4070, #35562, #10778, #35363, #7112, #13208, #26004, #25601, #19510, #10176, #28857, #1033, #13415, #35157, #7312, #19719, #32108, #38401, #17289 ),
 ( #1637, #4679, #11582, #26816, #29458, #14019, #4875, #7921, #5279, #14422, #23371, #20924, #32925, #24167, #30272, #39401, #11181, #17084, #30069, #26411, #23572, #33331, #17890, #38807, #14220, #36365, #10983, #23970, #5082, #8530, #29662, #35766, #39605, #5476 ),
 ( #29859, #2440, #20327, #39206, #32724, #14830, #23766, #1846, #26612, #27216, #2044, #11779, #20528, #7723, #39005, #36165, #35966, #8121, #17490, #11383, #14630, #20127, #8335, #20735, #33128, #32526, #17693, #2243, #27018, #12768, #27612, #15624, #21715, #6467 ),
 ( #24964, #18676, #34117, #3031, #6274, #36561, #15423, #37358, #33919, #30475, #24367, #12176, #15226, #31068, #18872, #11977, #27816, #24571, #30673, #36965, #21325, #5675, #31264, #33532, #9129, #25555, #9533, #21123, #28010, #27414, #3426, #3232, #8733, #388 ),
 ( #5877, #183, #36764, #12572, #21910, #34314, #39997, #15822, #28209, #18085, #8935, #2635, #15023, #6075, #33730, #12373, #39803, #18280, #18479, #2835, #21516, #30870, #24760, #37159, #9334, #584, #16631, #3826, #1386, #16226, #4229, #10325, #35311, #29012 ),
 ( #4021, #19665, #7470, #31661, #32059, #29216, #1187, #32266, #25757, #12966, #28609, #4431, #34710, #10526, #13369, #13568, #25355, #37757, #22310, #987, #25163, #19261, #22112, #7065, #25955, #9731, #9928, #38354, #31460, #37561, #6861, #780, #28812, #19877 ),
 ( #22909, #16835, #13162, #22503, #19070, #16422, #7263, #22706, #34512, #25556, #6662, #37957, #3626, #16021, #10128, #28408, #31858, #34913, #19462, #38153, #35109, #38759, #14175, #29415, #14380, #17846, #29817, #5033, #23723, #26767, #20081, #11136, #20486, #26366 ),
 ( #5236, #17242, #10731, #36121, #35515, #29615, #39360, #23924, #4633, #20279, #2197, #7678, #30020, #38962, #14583, #23326, #32478, #5438, #26973, #10940, #1792, #26572, #33287, #11536, #36322, #8486, #32679, #35722, #20885, #7874, #30226, #2002, #4833, #23116 ),
 ( #39157, #13975, #17035, #1591, #23522, #13770, #35918, #26162, #11338, #20689, #8077, #32880, #17444, #8282, #38557, #33084, #17649, #24517, #3186, #27173, #18037, #34068, #8688, #18827, #2594, #30432, #6026, #12526, #30822, #11933, #6229, #14980, #24714, #27765 ),
 ( #37115, #40154, #15576, #27367, #31020, #5834, #2394, #21863, #18234, #39559, #9084, #24917, #5628, #30627, #27567, #39755, #2785, #24323, #2989, #6422, #18431, #33875, #12327, #15375, #21079, #39954, #21470, #36721, #9282, #34268, #21666, #27963, #37310, #14784 ),
 ( #135, #9486, #33488, #8885, #11736, #24121, #18631, #12130, #36517, #21273, #33683, #15177, #36917, #28356, #34659, #31604, #10475, #28960, #4174, #16577, #37710, #535, #38304, #12919, #19614, #7012, #9874, #338, #37903, #1136, #12721, #13516, #22065, #6810 ),
 ( #22255, #25502, #19215, #25905, #6613, #22654, #3773, #7415, #16175, #10273, #16373, #22857, #35058, #35261, #32008, #13312, #28759, #10075, #934, #31215, #22457, #3379, #28560, #15771, #25312, #735, #13113, #28162, #25114, #37511, #9688, #34863, #19412, #34465 ),
 ( #31807, #7214, #3973, #19020, #31411, #25708, #3578, #15976, #38101, #1745, #27271, #32214, #26317, #14124, #10889, #2688, #35467, #11831, #38711, #36813, #23272, #39658, #4985, #30529, #24220, #15077, #8787, #1951, #17396, #26523, #29769, #19825, #38911, #21176 ),
 ( #7622, #35670, #39853, #29362, #5731, #8026, #36617, #20028, #32424, #16984, #35866, #24419, #13923, #16781, #11088, #33579, #4377, #4582, #18139, #26107, #29166, #1538, #7824, #23471, #27466, #20433, #20231, #12030, #32629, #14326, #1334, #13718, #4783, #38505 ),
 ( #17190, #10680, #29565, #23063, #32829, #12424, #5928, #15674, #19122, #12229, #24817, #34169, #33969, #9383, #24620, #9584, #13019, #25016, #241, #18924, #21969, #15278, #6320, #28062, #21569, #37411, #637, #34369, #34564, #3679, #25408, #21374, #21765, #6126 ),
 ( #15477, #37617, #30725, #25217, #18729, #9783, #18530, #2886, #8985, #6517, #12626, #31313, #3482, #27665, #31118, #15878, #30921, #28265, #33780, #441, #6714, #16073, #18329, #40049, #3282, #3084, #37013, #9183, #27867, #38, #12822, #28462, #37214, #22162 ),
 ( #31517, #10787, #34969, #1041, #38214, #17091, #35568, #23170, #7730, #4077, #7120, #4687, #19519, #26217, #13625, #16480, #6915, #4281, #20134, #19317, #32533, #28662, #13421, #1244, #31713, #29466, #25815, #29271, #26011, #31909, #10584, #22560, #25608, #32116 ),
 ( #22966, #1644, #1439, #14026, #38609, #19929, #35369, #16684, #7525, #37806, #29066, #9979, #35163, #3879, #38009, #10382, #28864, #32324, #22357, #13215, #38408, #22760, #7319, #19726, #4487, #16276, #34765, #835, #16890, #13822, #10182, #10991, #17895, #17297 ),
 ( #38813, #30481, #11588, #1851, #39610, #27224, #5087, #23773, #20337, #5285, #8536, #23976, #11785, #14227, #14835, #29865, #26419, #5682, #2050, #23378, #33134, #36567, #29669, #14427, #11391, #11186, #26822, #26618, #27026, #2642, #39010, #23578, #30074, #8739 ),
 ( #24172, #21128, #17497, #36173, #32730, #17697, #20929, #36371, #33538, #35975, #18093, #39212, #35773, #7927, #8340, #4884, #2247, #8128, #20536, #20741, #14634, #32932, #39408, #33338, #5481, #30278, #2450, #6280, #24972, #28018, #21330, #12380, #21721, #27617 ),
 ( #6475, #18484, #11982, #37365, #36770, #30876, #395, #25171, #5883, #21523, #3433, #8941, #31270, #40199, #15831, #24576, #33739, #6669, #28215, #12183, #3039, #15432, #34519, #12776, #37567, #9737, #33926, #36971, #22120, #9138, #19076, #31075, #6081, #24374 ),
 ( #18287, #31468, #30678, #27822, #18684, #2841, #15029, #24771, #18879, #3240, #37166, #193, #40005, #15231, #9341, #27419, #34123, #9541, #15632, #12580, #39808, #21919, #34321, #26170, #10134, #38362, #7687, #22917, #10737, #4235, #19269, #34921, #23122, #13169 ),
 ( #31668, #35117, #31864, #37963, #4028, #28616, #12973, #38564, #590, #16429, #7270, #4439, #28415, #35318, #34716, #35523, #7476, #6869, #20088, #13575, #16029, #3632, #29021, #3833, #16841, #29223, #22511, #994, #37764, #22713, #25961, #1195, #1392, #16233 ),
 ( #10534, #13375, #786, #19672, #25362, #25564, #7072, #9935, #22317, #19470, #28819, #19883, #32066, #25764, #38162, #10332, #16638, #32275, #13778, #7880, #5446, #17452, #8696, #14792, #23932, #35926, #29423, #14591, #13981, #8084, #17854, #2402, #23333, #38969 ),
 ( #11545, #27182, #20287, #39567, #11743, #26578, #1599, #36524, #11143, #14387, #24128, #4840, #39164, #38767, #32484, #8291, #32685, #26372, #4640, #26774, #36328, #5041, #30233, #35729, #20696, #17249, #29622, #10948, #11347, #39366, #17043, #23529, #23729, #20493 ),
 ( #8492, #32887, #1800, #29823, #20891, #17655, #14183, #33293, #2008, #36128, #26980, #30029, #33090, #2205, #5243, #40165, #9496, #18442, #14988, #8894, #36928, #39963, #15587, #3389, #36730, #12336, #9094, #15187, #21479, #5842, #30440, #15783, #18047, #33885 ),
 ( #21284, #21872, #5635, #33693, #12536, #27375, #37522, #18244, #30637, #24724, #31225, #9294, #2795, #24928, #27578, #3198, #6238, #147, #12140, #27972, #34279, #28173, #24530, #6433, #18640, #30832, #6038, #37124, #2602, #11942, #2998, #350, #39764, #24333 ),
 ( #15386, #21678, #25123, #34079, #31031, #37323, #18837, #27778, #12731, #21088, #33496, #38113, #1346, #10285, #35273, #4389, #26121, #22075, #10088, #34671, #37720, #3590, #9886, #22266, #28972, #16794, #25321, #29180, #13729, #3785, #6623, #9699, #16187, #31819 ),
 ( #7429, #22869, #19838, #28571, #6824, #34475, #19225, #38315, #25719, #745, #19031, #16386, #32226, #31423, #15985, #546, #13123, #13327, #28366, #12930, #25514, #1147, #22667, #31615, #35071, #37916, #22468, #3984, #10487, #34873, #19626, #7024, #19426, #28772 ),
 ( #7225, #947, #32022, #4187, #16590, #13530, #25918, #32436, #26330, #14137, #17201, #33048, #20847, #13934, #29783, #26535, #32641, #38923, #23286, #7634, #33246, #35478, #11099, #26731, #5198, #38724, #10900, #35681, #14339, #2359, #4795, #20041, #20445, #39320 ),
 ( #23079, #29976, #29374, #5395, #8241, #10692, #14743, #23683, #7835, #11497, #23882, #29578, #35879, #4595, #17407, #20647, #36081, #36287, #20243, #26933, #1756, #38517, #17809, #23482, #16995, #4996, #8449, #1551, #8037, #32843, #1963, #39117, #11303, #17607 ),
 ( #2156, #14539, #30184, #33448, #24478, #33836, #39718, #15334, #18787, #27723, #12482, #21824, #3340, #39520, #27530, #11894, #14942, #21039, #27330, #24283, #6188, #34229, #2555, #6380, #31175, #21234, #24084, #27132, #33645, #9047, #37271, #36678, #5984, #5590 ),
 ( #8848, #18001, #9445, #21430, #30977, #39911, #24876, #30388, #2947, #5794, #18196, #36478, #18392, #34032, #11697, #30589, #30784, #2746, #8646, #15139, #18593, #12089, #36874, #40111, #3143, #12288, #24677, #15539, #37071, #27923, #9240, #21627, #100, #897 ),
 ( #35027, #22823, #16336, #31372, #6772, #35219, #25275, #1099, #28921, #12879, #19173, #16135, #7380, #13479, #25867, #38270, #22215, #37668, #19783, #9837, #4134, #31773, #34619, #25076, #22414, #10438, #37472, #32178, #6575, #31567, #19374, #9648, #15732, #3733 ),
 ( #28121, #3537, #7179, #28519, #299, #694, #19577, #13274, #12681, #31969, #22026, #16539, #38064, #25666, #34818, #10234, #34425, #6970, #18981, #13071, #15935, #28318, #25462, #37862, #22620, #499, #10035, #3935, #28718, #38673, #4747, #29329, #13681, #26882 ),
 ( #5149, #29126, #19991, #36034, #10643, #20798, #4544, #32387, #7985, #14489, #32792, #13890, #8193, #16945, #26681, #29732, #23637, #23238, #39069, #17555, #11449, #1499, #29929, #1911, #1705, #26278, #35828, #26069, #35426, #10846, #23835, #38470, #23026, #1298 ),
 ( #4950, #8401, #20398, #17356, #14289, #11248, #7586, #14085, #11052, #35631, #20600, #36241, #32998, #2109, #39270, #4340, #16745, #17154, #7789, #20192, #32588, #29530, #26482, #38876, #23436, #8594, #49, #12434, #27285, #33981, #24827, #5541, #6137, #30734 ),
 ( #36632, #30135, #39864, #3096, #36430, #8801, #18151, #17952, #33593, #20992, #33791, #37225, #8997, #24431, #2897, #5939, #39474, #30541, #12041, #30337, #21384, #9396, #18341, #18541, #27876, #33195, #5346, #5745, #2509, #33400, #27085, #14896, #39670, #12239 ),
 ( #21579, #11844, #11653, #17760, #30931, #24233, #21188, #2700, #2308, #15491, #14694, #24035, #15087, #27478, #36824, #15287, #27675, #40062, #24629, #37023, #9193, #1401, #18740, #13786, #251, #15889, #31525, #31129, #29231, #28275, #35327, #3688, #21978, #28471 ),
 ( #34572, #32285, #34379, #25418, #3492, #6529, #38574, #6723, #10543, #26178, #31322, #38370, #23132, #7486, #10745, #646, #12638, #452, #35531, #18934, #16851, #16086, #22928, #25027, #37420, #12834, #13027, #21774, #25227, #3292, #19132, #4447, #15684, #9596 ),
 ( #37625, #34179, #19891, #28072, #6331, #9793, #22173, #40161, #21674, #6619, #18637, #15982, #15583, #31419, #34075, #24721, #31221, #25317, #6235, #19026, #27969, #31026, #3781, #15778, #3585, #19222, #3193, #28363, #742, #541, #16184, #37517, #12333, #143 ),
 ( #22262, #25120, #12927, #37121, #9289, #12532, #12728, #13120, #24925, #33882, #18833, #37717, #21476, #37318, #9881, #2995, #36925, #9493, #21869, #345, #6819, #9696, #34274, #6430, #3385, #34667, #28169, #31612, #22071, #28567, #9091, #6033, #34471, #18438 ),
 ( #30828, #15383, #27771, #32222, #35678, #28767, #28968, #10484, #10281, #25915, #943, #26117, #29573, #1342, #16789, #35475, #38513, #31815, #22865, #4385, #38110, #13726, #17198, #10688, #10897, #20240, #1753, #37911, #38312, #22664, #13321, #19423, #25716, #35067 ),
 ( #35269, #13930, #7222, #3981, #25509, #38720, #19622, #1144, #7424, #4791, #23280, #7832, #32637, #32016, #4183, #10083, #16586, #26325, #23073, #13525, #34870, #29177, #22465, #7020, #16381, #19833, #7630, #20036, #32433, #4591, #16992, #29370, #1547, #29778 ),
 ( #23679, #21230, #23479, #8034, #11096, #17997, #33243, #35875, #20441, #11299, #14334, #11694, #20842, #1960, #27326, #39315, #30585, #36673, #5585, #17603, #32838, #36474, #4993, #29972, #39715, #24279, #17404, #20644, #2550, #26728, #30385, #11494, #14939, #36077 ),
 ( #39113, #18193, #8238, #36282, #8844, #33043, #5390, #5194, #33642, #30180, #2152, #14535, #5789, #8446, #11889, #26929, #14133, #23879, #2355, #17805, #26531, #14739, #38919, #27129, #39515, #24080, #8642, #21035, #33444, #18388, #34420, #21622, #19169, #34027 ),
 ( #12875, #6570, #25269, #31367, #25071, #28116, #9440, #295, #2743, #21819, #3533, #95, #36871, #30780, #18587, #6183, #37467, #37664, #2942, #34224, #30972, #37067, #3138, #27718, #12084, #9832, #39907, #15535, #6376, #15931, #27525, #18977, #33833, #22211 ),
 ( #18781, #34615, #31171, #12284, #5981, #40108, #12677, #24674, #22021, #27919, #9643, #28313, #6768, #15330, #494, #15135, #12478, #9237, #3336, #24474, #9042, #21427, #24872, #37266, #15728, #7374, #28713, #4334, #16330, #19370, #25863, #19986, #891, #1293 ),
 ( #1494, #32383, #13677, #16740, #38265, #29122, #31562, #10434, #4539, #28917, #25456, #31768, #7175, #10229, #26065, #13885, #6965, #22818, #19572, #25662, #31963, #13270, #689, #26274, #28514, #4129, #35214, #16941, #16131, #23021, #22410, #38668, #38465, #3728 ),
 ( #19779, #38059, #34812, #22616, #10638, #35022, #35422, #16534, #7580, #29325, #10840, #3931, #23232, #35627, #1095, #13474, #32173, #13066, #7784, #37857, #10031, #29526, #14078, #17148, #24030, #39266, #1701, #26476, #17350, #20393, #17755, #26877, #35824, #33395 ),
 ( #8397, #11839, #20793, #5537, #14891, #36625, #32583, #20595, #4946, #7980, #38871, #32787, #29727, #39468, #27280, #1907, #39666, #24228, #14284, #11048, #20188, #26677, #2105, #30331, #39065, #11445, #23432, #2504, #36235, #11243, #23632, #4742, #14484, #36425 ),
 ( #36030, #33191, #8188, #32993, #23828, #5144, #17550, #29924, #14690, #5341, #30130, #2304, #27079, #11648, #8589, #20986, #17948, #31318, #5740, #21574, #12430, #9590, #33587, #246, #39859, #3487, #18735, #21184, #12828, #34175, #24427, #21974, #37219, #36819 ),
 ( #28067, #27670, #3288, #34374, #15884, #21380, #6525, #6325, #6131, #33786, #44, #30536, #12036, #18335, #28270, #18147, #2695, #15083, #12632, #27872, #27472, #8992, #5934, #30730, #31125, #15486, #2891, #18930, #33975, #25224, #447, #25022, #12234, #15283 ),
 ( #24625, #8797, #40056, #37019, #9189, #37416, #18536, #30926, #3089, #24822, #9390, #21770, #15680, #10589, #34771, #841, #38014, #16895, #35375, #22972, #7532, #3884, #6920, #4493, #19323, #26017, #13426, #16282, #6719, #4082, #19936, #19128, #32329, #22363 ) ),
 .UNSPECIFIED., .F., .F., .F.,
 ( 4, 3, 3, 3, 3, 3, 3, 3, 3, 3, 3, 3, 3, 3, 3, 3, 3, 3, 3, 3, 3, 3, 3, 3, 3, 3, 3, 3, 3, 3, 3, 3, 3, 3, 3, 3, 3, 3, 3, 3, 3, 3, 3, 3, 3, 3, 3, 3, 3, 3, 3, 4 ),
 ( 4, 3, 3, 3, 3, 3, 3, 3, 3, 3, 3, 4 ),
 ( -4.440892098500626162E-16, 0.0001220703125634871116, 0.0002441406251274183124, 0.0004882812502552807141, 0.0009765625005110055174, 0.001953125001022455124, 0.003906250002045354337, 0.007812500004091152764, 0.01562500000818274962, 0.03125000001636594332, 0.04687500002454914050, 0.06250000003273233073, 0.07812500004091552097, 0.09375000004909872509, 0.1093750000572819153, 0.1250000000654651056, 0.1406250000736483097, 0.1416015625741597617, 0.1420898438244154738, 0.1425781250746712137, 0.1445312500756941176, 0.1484375000777398979, 0.1562500000818314860, 0.1718750000900146901, 0.1875000000981978943, 0.2031250001063810706, 0.2187500001145642747, 0.2343750001227474788, 0.2500000001309306552, 0.2656250001391138316, 0.2812500001472970634, 0.2968750001554802398, 0.3125000001636634162, 0.3281250001718466480, 0.3320312501738924560, 0.3330078126744039357, 0.3332519532995317779, 0.3334960939246596201, 0.3339843751749153600, 0.3359375001759382640, 0.3437500001800298244, 0.3750000001963962326, 0.4062500002127625853, 0.4375000002291289936, 0.4687500002454954018, 0.4726562502475412098, 0.4746093752485641137, 0.4750976564988198536, 0.4755859377490755380, 0.4765625002495870177, 0.4843750002536785781, 0.5000000002618617545 ),
 ( 0.000000000000000000, 0.06250000000000004163, 0.1250000000000000833, 0.1875000000000001110, 0.2500000000000001665, 0.3750000000000002220, 0.5000000000000003331, 0.6250000000000004441, 0.7500000000000004441, 0.8750000000000005551, 0.9375000000000006661, 1.000000000000000666 ),
 .UNSPECIFIED. ) ;
#36923 = VERTEX_POINT ( 'NONE', #14943 ) ;
#36924 = FACE_OUTER_BOUND ( 'NONE', #29931, .T. ) ;
#36925 = CARTESIAN_POINT ( 'NONE',  ( -13.30932211733667714, -23.61699183225733734, -14.47971286837055516 ) ) ;
#36926 = CARTESIAN_POINT ( 'NONE',  ( -31.94006737154538200, 0.9747213384856526774, 13.92931973827809067 ) ) ;
#36927 = CARTESIAN_POINT ( 'NONE',  ( -28.82765927138905582, -24.00093021346537370, -6.713486956739352252 ) ) ;
#36928 = CARTESIAN_POINT ( 'NONE',  ( 1.466865423182375894, -22.17185249639828371, -19.06817386734656239 ) ) ;
#36929 = CARTESIAN_POINT ( 'NONE',  ( 13.16433369016599642, 21.27373372467787505, -17.47625806870802379 ) ) ;
#36930 = CARTESIAN_POINT ( 'NONE',  ( 18.28086812270377948, 11.17358269430334339, -22.25045871718272394 ) ) ;
#36931 = DIRECTION ( 'NONE',  ( -0.8660254037844432595, -0.4999999999999920064, 0.000000000000000000 ) ) ;
#36932 = CARTESIAN_POINT ( 'NONE',  ( -5.098808368553501502, 35.72236394901918999, -9.747318335016483815 ) ) ;
#36933 = ORIENTED_EDGE ( 'NONE', *, *, #1223, .T. ) ;
#36934 = CARTESIAN_POINT ( 'NONE',  ( -24.31092352897995923, -3.750127306134790395, -20.04326310685654278 ) ) ;
#36935 = ADVANCED_FACE ( 'NONE', ( #5199 ), #1396, .F. ) ;
#36936 = CARTESIAN_POINT ( 'NONE',  ( -18.69515074623005901, 22.45407711376556747, 11.55979286846285703 ) ) ;
#36937 = ORIENTED_EDGE ( 'NONE', *, *, #30354, .T. ) ;
#36938 = CARTESIAN_POINT ( 'NONE',  ( 8.559505275947156377, 25.28115294937476065, 13.00000000000000178 ) ) ;
#36939 = FACE_OUTER_BOUND ( 'NONE', #10407, .T. ) ;
#36940 = CARTESIAN_POINT ( 'NONE',  ( -26.25002775687122991, 0.6713331420556990503, -15.48113191161911040 ) ) ;
#36941 = CARTESIAN_POINT ( 'NONE',  ( 29.97182693708377244, -10.99419485510059857, -13.85563110560112676 ) ) ;
#36942 = AXIS2_PLACEMENT_3D ( 'NONE', #17247, #23526, #19468 ) ;
#36943 = VECTOR ( 'NONE', #21861, 999.9999999999998863 ) ;
#36944 = VERTEX_POINT ( 'NONE', #38366 ) ;
#36945 = DIRECTION ( 'NONE',  ( -0.000000000000000000, -0.000000000000000000, -1.000000000000000000 ) ) ;
#36946 = VERTEX_POINT ( 'NONE', #29977 ) ;
#36947 = AXIS2_PLACEMENT_3D ( 'NONE', #30306, #36207, #2478 ) ;
#36948 = CARTESIAN_POINT ( 'NONE',  ( 14.97191702109865297, 21.44669161452667794, 10.49999999999999822 ) ) ;
#36949 = CARTESIAN_POINT ( 'NONE',  ( -11.87435565298220652, 15.06698729810788961, 7.499999999999993783 ) ) ;
#36950 = EDGE_CURVE ( 'NONE', #32321, #17014, #32894, .T. ) ;
#36951 = FACE_OUTER_BOUND ( 'NONE', #216, .T. ) ;
#36952 = ORIENTED_EDGE ( 'NONE', *, *, #27799, .F. ) ;
#36953 = ADVANCED_FACE ( 'NONE', ( #32071 ), #4695, .T. ) ;
#36954 = CARTESIAN_POINT ( 'NONE',  ( -2.597202671505355998, 23.56478163197531472, -21.87304641510805325 ) ) ;
#36955 = CARTESIAN_POINT ( 'NONE',  ( 13.05736835487433289, 16.11602540378438420, 9.500000000000000000 ) ) ;
#36956 = DIRECTION ( 'NONE',  ( 0.000000000000000000, 0.000000000000000000, 1.000000000000000000 ) ) ;
#36957 = CARTESIAN_POINT ( 'NONE',  ( 2.525645716490518389, 8.212903943950921715, 7.000000000000000000 ) ) ;
#36958 = CARTESIAN_POINT ( 'NONE',  ( 29.35710168727448277, -22.60462445154060163, -8.421042284273656975 ) ) ;
#36959 = CARTESIAN_POINT ( 'NONE',  ( 15.82973276131441409, 13.18043781167240525, -27.70532646144207689 ) ) ;
#36960 = CARTESIAN_POINT ( 'NONE',  ( 12.74815967810739714, 30.65541959961472074, -9.036990827636632417 ) ) ;
#36961 = ORIENTED_EDGE ( 'NONE', *, *, #38535, .T. ) ;
#36962 = EDGE_CURVE ( 'NONE', #25278, #163, #26086, .T. ) ;
#36963 = CARTESIAN_POINT ( 'NONE',  ( -18.35172899305704064, 9.167379654309337766, -29.42880166646513018 ) ) ;
#36964 = CARTESIAN_POINT ( 'NONE',  ( 4.672335726382788046, 24.36080358023179571, 23.00000000000000000 ) ) ;
#36965 = CARTESIAN_POINT ( 'NONE',  ( 12.43149986465983581, -22.02020054580998476, -17.42080020519824757 ) ) ;
#36966 = CARTESIAN_POINT ( 'NONE',  ( -0.9819677022348329842, 30.37627742347970283, 12.00000000000000000 ) ) ;
#36967 = CARTESIAN_POINT ( 'NONE',  ( -11.41987377193683528, -19.41918266173334828, -20.90349153980999475 ) ) ;
#36969 = CIRCLE ( 'NONE', #18161, 16.00000000000000000 ) ;
#36968 = CARTESIAN_POINT ( 'NONE',  ( -15.00814140074610137, 26.00168467618496848, -9.236653823862166490 ) ) ;
#36970 = CARTESIAN_POINT ( 'NONE',  ( -13.64791795088057569, -15.39248673868869943, -28.54146132201631758 ) ) ;
#36971 = CARTESIAN_POINT ( 'NONE',  ( 8.501265317358036810, -19.09793930249271199, -26.33487222037532760 ) ) ;
#36972 = CARTESIAN_POINT ( 'NONE',  ( 11.40045258775034931, 32.09219725203293194, 10.82238833324614191 ) ) ;
#36973 = ORIENTED_EDGE ( 'NONE', *, *, #36169, .F. ) ;
#36974 = AXIS2_PLACEMENT_3D ( 'NONE', #20065, #4005, #22292 ) ;
#36975 = CARTESIAN_POINT ( 'NONE',  ( -7.311911706866655258, 22.04011237685605806, -22.15126999930638974 ) ) ;
#36976 = ADVANCED_FACE ( 'NONE', ( #22923 ), #30389, .F. ) ;
#36977 = CARTESIAN_POINT ( 'NONE',  ( 14.26584437371809777, 27.13525491562438319, 12.00000000000000000 ) ) ;
#36978 = CARTESIAN_POINT ( 'NONE',  ( -3.118678732975735279, 7.827785988993307242, 12.00000000000000000 ) ) ;
#36979 = EDGE_CURVE ( 'NONE', #32514, #16315, #21567, .T. ) ;
#36980 = DIRECTION ( 'NONE',  ( -0.6724985119639524944, 0.2185080122244146827, -0.7071067811865507924 ) ) ;
#36981 = VERTEX_POINT ( 'NONE', #19887 ) ;
#36982 = CARTESIAN_POINT ( 'NONE',  ( 24.54342919967269054, 0.4649732435212016179, -18.45589562361645619 ) ) ;
#36983 = LINE ( 'NONE', #410, #8969 ) ;
#36984 = FACE_OUTER_BOUND ( 'NONE', #39181, .T. ) ;
#36985 = ORIENTED_EDGE ( 'NONE', *, *, #10260, .F. ) ;
#36986 = CARTESIAN_POINT ( 'NONE',  ( -29.32665613511613500, 0.1060819663625076903, -10.65436168154521646 ) ) ;
#36987 = DIRECTION ( 'NONE',  ( 0.000000000000000000, 0.000000000000000000, 1.000000000000000000 ) ) ;
#36988 = EDGE_LOOP ( 'NONE', ( #21201, #31448, #25327 ) ) ;
#36989 = CARTESIAN_POINT ( 'NONE',  ( 33.33462692813205308, -5.949911538848129844, -9.434312102335114858 ) ) ;
#36990 = ORIENTED_EDGE ( 'NONE', *, *, #6145, .F. ) ;
#36991 = CARTESIAN_POINT ( 'NONE',  ( -17.01882136418224789, 27.23043334310857233, 13.32518128616608877 ) ) ;
#36992 = CARTESIAN_POINT ( 'NONE',  ( -6.008588623656293315, -15.38567963534269900, 20.94377226548378701 ) ) ;
#36993 = CARTESIAN_POINT ( 'NONE',  ( -0.6108529249775870307, 37.48755679569043053, 7.500000000000000888 ) ) ;
#36994 = ADVANCED_FACE ( 'NONE', ( #27331 ), #30185, .T. ) ;
#36995 = CARTESIAN_POINT ( 'NONE',  ( 4.183427099969757812, 31.55590659971980472, 20.25080042701566185 ) ) ;
#36996 = CARTESIAN_POINT ( 'NONE',  ( 5.136393443230283573, 36.08535633838087620, 10.66666666666666607 ) ) ;
#36997 = VERTEX_POINT ( 'NONE', #35121 ) ;
#36998 = ADVANCED_FACE ( 'NONE', ( #4239 ), #24150, .T. ) ;
#36999 = CARTESIAN_POINT ( 'NONE',  ( -10.44103466624267540, 32.57396620494226624, 11.00000000000000000 ) ) ;
#37000 = LINE ( 'NONE', #36797, #37705 ) ;
#37001 = AXIS2_PLACEMENT_3D ( 'NONE', #32662, #21063, #29802 ) ;
#37002 = CARTESIAN_POINT ( 'NONE',  ( 12.31033848243464668, 14.30014505118389145, 10.49999999999999467 ) ) ;
#37003 = CARTESIAN_POINT ( 'NONE',  ( 6.978616903035645080, 30.76321682976233163, -13.89331903619694231 ) ) ;
#37004 = DIRECTION ( 'NONE',  ( -0.000000000000000000, -0.000000000000000000, -1.000000000000000000 ) ) ;
#37005 = CARTESIAN_POINT ( 'NONE',  ( 16.05151241257415506, -23.71462521554112257, -14.24666968269734291 ) ) ;
#37006 = DIRECTION ( 'NONE',  ( -1.000000000000000000, 0.000000000000000000, 0.000000000000000000 ) ) ;
#37007 = LINE ( 'NONE', #18132, #39763 ) ;
#37008 = DIRECTION ( 'NONE',  ( 1.000000000000000000, 0.000000000000000000, 0.000000000000000000 ) ) ;
#37009 = VERTEX_POINT ( 'NONE', #1199 ) ;
#37010 = CARTESIAN_POINT ( 'NONE',  ( -15.41384351598270719, 26.69841823979104589, -5.946086308406814069 ) ) ;
#37011 = AXIS2_PLACEMENT_3D ( 'NONE', #2721, #28895, #7151 ) ;
#37012 = CARTESIAN_POINT ( 'NONE',  ( -33.46894051142380277, -4.475137156698075991, 16.87380292611441490 ) ) ;
#37013 = CARTESIAN_POINT ( 'NONE',  ( 9.808896528483906252, -18.87720056256629775, -25.03243745114713903 ) ) ;
#37014 = CARTESIAN_POINT ( 'NONE',  ( -3.992867117591419213, 8.524771480177605554, 10.49999999999999822 ) ) ;
#37015 = ORIENTED_EDGE ( 'NONE', *, *, #35460, .F. ) ;
#37016 = VERTEX_POINT ( 'NONE', #25965 ) ;
#37017 = CARTESIAN_POINT ( 'NONE',  ( -13.86191765000858034, 30.49075772208747992, -5.458815180633147968 ) ) ;
#37018 = B_SPLINE_CURVE_WITH_KNOTS ( 'NONE', 3,
 ( #34594, #1075, #19153, #16110, #28495, #13452 ),
 .UNSPECIFIED., .F., .F.,
 ( 4, 2, 4 ),
 ( 0.000000000000000000, 0.5000000000000000000, 1.000000000000000000 ),
 .UNSPECIFIED. ) ;
#37019 = CARTESIAN_POINT ( 'NONE',  ( -20.49308938538982616, -27.11270024657357425, -6.352872741783973431 ) ) ;
#37020 = CARTESIAN_POINT ( 'NONE',  ( 15.29245034862073283, 32.56469986092002955, -4.999999999999995559 ) ) ;
#37021 = ORIENTED_EDGE ( 'NONE', *, *, #29729, .F. ) ;
#37022 = CARTESIAN_POINT ( 'NONE',  ( -20.10573352757293009, -5.610599920320681555, -27.07607080465070837 ) ) ;
#37023 = CARTESIAN_POINT ( 'NONE',  ( -12.13390174137889943, -22.02765613461586369, -17.45112777453272557 ) ) ;
#37024 = CARTESIAN_POINT ( 'NONE',  ( 13.96188064734268686, 27.98367808437124538, 7.382773698552470343 ) ) ;
#37025 = VERTEX_POINT ( 'NONE', #7481 ) ;
#37026 = CARTESIAN_POINT ( 'NONE',  ( 20.43785338154470921, 1.730618592969307867, -29.36392387493818035 ) ) ;
#37027 = DIRECTION ( 'NONE',  ( 0.000000000000000000, 0.000000000000000000, 1.000000000000000000 ) ) ;
#37028 = DIRECTION ( 'NONE',  ( 0.000000000000000000, 0.000000000000000000, 1.000000000000000000 ) ) ;
#37029 = EDGE_CURVE ( 'NONE', #1914, #16860, #10741, .T. ) ;
#37030 = B_SPLINE_CURVE_WITH_KNOTS ( 'NONE', 3,
 ( #31248, #37742, #34690, #19245 ),
 .UNSPECIFIED., .F., .F.,
 ( 4, 4 ),
 ( 0.000000000000000000, 1.000000000000000000 ),
 .UNSPECIFIED. ) ;
#37031 = VECTOR ( 'NONE', #29256, 1000.000000000000000 ) ;
#37032 = EDGE_LOOP ( 'NONE', ( #22208, #20899, #13987, #10045 ) ) ;
#37033 = CARTESIAN_POINT ( 'NONE',  ( -25.22586935555838394, 0.3525131807024055042, -17.43529033463691746 ) ) ;
#37034 = EDGE_LOOP ( 'NONE', ( #14171, #27673, #9962, #32950 ) ) ;
#37035 = CARTESIAN_POINT ( 'NONE',  ( 20.54762595280696047, -0.6097413519664565129, -28.65496405823322590 ) ) ;
#37036 = CARTESIAN_POINT ( 'NONE',  ( 23.43324262027548599, -8.134040356058108046, 20.99999999999999645 ) ) ;
#37037 = CARTESIAN_POINT ( 'NONE',  ( 33.23893881994253263, -12.50319288011949936, 18.42518152272107912 ) ) ;
#37038 = ORIENTED_EDGE ( 'NONE', *, *, #34484, .T. ) ;
#37039 = CARTESIAN_POINT ( 'NONE',  ( -20.40386927488033919, 2.900997764857453198, -28.16784849636700372 ) ) ;
#37040 = CARTESIAN_POINT ( 'NONE',  ( 7.096882951594522204, 29.56287847632727050, 10.50000000000000000 ) ) ;
#37041 = CARTESIAN_POINT ( 'NONE',  ( -11.44134295108998955, 15.31698729810788784, 10.50000000000000000 ) ) ;
#37042 = AXIS2_PLACEMENT_3D ( 'NONE', #22345, #19110, #31896 ) ;
#37043 = PLANE ( 'NONE',  #38218 ) ;
#37044 = CIRCLE ( 'NONE', #7155, 0.5000000000000007772 ) ;
#37045 = CARTESIAN_POINT ( 'NONE',  ( -2.140527761532693418, 7.619874298175171035, 10.50000000000000000 ) ) ;
#37046 = FACE_BOUND ( 'NONE', #4889, .T. ) ;
#37047 = CARTESIAN_POINT ( 'NONE',  ( 32.09165771328606809, 1.123514972292636083, 13.32518128616608877 ) ) ;
#37048 = ORIENTED_EDGE ( 'NONE', *, *, #1844, .F. ) ;
#37049 = CARTESIAN_POINT ( 'NONE',  ( -23.58215323251389250, 7.916431794952161205, -10.35477734161397123 ) ) ;
#37050 = CYLINDRICAL_SURFACE ( 'NONE', #21680, 0.4999999999999998335 ) ;
#37051 = ADVANCED_FACE ( 'NONE', ( #18982 ), #300, .F. ) ;
#37052 = DIRECTION ( 'NONE',  ( -0.9945218953682730678, 0.1045284632676566905, 7.253119165527330602E-16 ) ) ;
#37053 = CARTESIAN_POINT ( 'NONE',  ( 23.53567760670948772, -25.90459182271207794, -8.508653576017058739 ) ) ;
#37054 = VECTOR ( 'NONE', #30060, 1000.000000000000227 ) ;
#37055 = CARTESIAN_POINT ( 'NONE',  ( -13.30736835483215508, 15.77027916469387847, 10.49999999999999645 ) ) ;
#37056 = CARTESIAN_POINT ( 'NONE',  ( 15.09835175993660172, 26.53469318400227905, -8.288073639389835989 ) ) ;
#37057 = ORIENTED_EDGE ( 'NONE', *, *, #26202, .F. ) ;
#37058 = CARTESIAN_POINT ( 'NONE',  ( -12.29080222946883794, 16.45214217256524236, -28.75623754596550441 ) ) ;
#37059 = CARTESIAN_POINT ( 'NONE',  ( -19.90456025098508164, -17.02442174103788020, 20.99999999999999645 ) ) ;
#37060 = FACE_OUTER_BOUND ( 'NONE', #39663, .T. ) ;
#37061 = CARTESIAN_POINT ( 'NONE',  ( 14.04351365870728685, 23.90287290350755711, -13.51466990167370064 ) ) ;
#37062 = EDGE_LOOP ( 'NONE', ( #4855, #15954, #3552, #20540 ) ) ;
#37063 = DIRECTION ( 'NONE',  ( 1.000000000000000000, 0.000000000000000000, 0.000000000000000000 ) ) ;
#37064 = ORIENTED_EDGE ( 'NONE', *, *, #29193, .F. ) ;
#37066 = DIRECTION ( 'NONE',  ( 0.7431448254773961315, 0.6691306063588561281, 0.000000000000000000 ) ) ;
#37065 = CARTESIAN_POINT ( 'NONE',  ( -14.83272754704879581, 26.11747447809059253, -9.691566001703526112 ) ) ;
#37067 = CARTESIAN_POINT ( 'NONE',  ( -11.65106285942700559, -20.96414419292345599, -19.48341064667247124 ) ) ;
#37068 = LINE ( 'NONE', #30973, #15339 ) ;
#37069 = CIRCLE ( 'NONE', #30607, 1.000000000000000000 ) ;
#37070 = CARTESIAN_POINT ( 'NONE',  ( -34.68504811378230812, -15.55931908636949856, -6.702081268225836830 ) ) ;
#37071 = CARTESIAN_POINT ( 'NONE',  ( -8.882954391321824517, -18.80275190887125092, -26.89438617859911318 ) ) ;
#37072 = CARTESIAN_POINT ( 'NONE',  ( -14.52509594610762456, 21.97885917798744870, 10.49999999999999467 ) ) ;
#37073 = CARTESIAN_POINT ( 'NONE',  ( 11.95648576969578514, 17.00773961595601946, -26.90402825398920683 ) ) ;
#37074 = ORIENTED_EDGE ( 'NONE', *, *, #26758, .F. ) ;
#37075 = CARTESIAN_POINT ( 'NONE',  ( 25.36334589218571622, 5.533731653267201622, -9.821327216179092545 ) ) ;
#37076 = CIRCLE ( 'NONE', #39647, 0.5000000000000004441 ) ;
#37077 = EDGE_CURVE ( 'NONE', #13835, #13564, #24284, .T. ) ;
#37078 = DIRECTION ( 'NONE',  ( 0.000000000000000000, 0.000000000000000000, 1.000000000000000000 ) ) ;
#37079 = CARTESIAN_POINT ( 'NONE',  ( -13.28401428810686724, 15.50858767547201822, 10.49999999999999822 ) ) ;
#37080 = CARTESIAN_POINT ( 'NONE',  ( -20.57926082878400820, -27.21289976832866842, -5.911089126657673276 ) ) ;
#37081 = EDGE_LOOP ( 'NONE', ( #10025, #12925, #11035, #13512, #38176 ) ) ;
#37082 = CARTESIAN_POINT ( 'NONE',  ( -29.50951042545606740, -0.6464191806711061528, -11.53192585844440288 ) ) ;
#37083 = ADVANCED_FACE ( 'NONE', ( #34033 ), #36679, .F. ) ;
#37084 = CARTESIAN_POINT ( 'NONE',  ( 30.94917753044411057, -0.3725058681004523864, -7.345268830895530954 ) ) ;
#37085 = CARTESIAN_POINT ( 'NONE',  ( -26.46527715132802783, -30.05405011173883167, 10.99999999999999822 ) ) ;
#37086 = EDGE_CURVE ( 'NONE', #32089, #747, #27531, .T. ) ;
#37087 = CARTESIAN_POINT ( 'NONE',  ( 27.41073561697711369, -13.75826678482997423, 20.69868183039782750 ) ) ;
#37088 = ORIENTED_EDGE ( 'NONE', *, *, #4369, .T. ) ;
#37089 = CIRCLE ( 'NONE', #4662, 1.000000000000000888 ) ;
#37090 = EDGE_CURVE ( 'NONE', #12080, #13281, #1447, .T. ) ;
#37091 = CARTESIAN_POINT ( 'NONE',  ( 37.49625565938770677, -14.69322820095493221, -4.999999999999991118 ) ) ;
#37092 = DIRECTION ( 'NONE',  ( 0.000000000000000000, -0.000000000000000000, -1.000000000000000000 ) ) ;
#37093 = EDGE_LOOP ( 'NONE', ( #11965, #31016, #7110, #9908 ) ) ;
#37094 = CARTESIAN_POINT ( 'NONE',  ( -14.98890122036483419, -28.67928442680469203, -4.999999999999999112 ) ) ;
#37095 = VECTOR ( 'NONE', #35709, 1000.000000000000000 ) ;
#37096 = CARTESIAN_POINT ( 'NONE',  ( -19.26948696230206082, 27.85601271560033965, 22.99999999999999645 ) ) ;
#37097 = DIRECTION ( 'NONE',  ( -0.9781476007338042455, 0.2079116908177664758, 0.000000000000000000 ) ) ;
#37098 = ADVANCED_FACE ( 'NONE', ( #12682 ), #27724, .F. ) ;
#37099 = CARTESIAN_POINT ( 'NONE',  ( 2.591799644895701693, 25.51815422415490531, -19.65972820106781072 ) ) ;
#37100 = DIRECTION ( 'NONE',  ( 0.000000000000000000, 0.000000000000000000, 1.000000000000000000 ) ) ;
#37101 = ADVANCED_FACE ( 'NONE', ( #18197 ), #25077, .F. ) ;
#37102 = DIRECTION ( 'NONE',  ( -0.000000000000000000, -0.000000000000000000, -1.000000000000000000 ) ) ;
#37103 = EDGE_CURVE ( 'NONE', #16182, #7701, #11829, .T. ) ;
#37104 = DIRECTION ( 'NONE',  ( -0.9986295347545740553, 0.05233595624294183624, -1.941170045126910451E-16 ) ) ;
#37105 = LINE ( 'NONE', #37502, #39405 ) ;
#37106 = CARTESIAN_POINT ( 'NONE',  ( 11.96428041830149169, 31.54822188126892613, 7.102474990965860435 ) ) ;
#37107 = SURFACE_SIDE_STYLE ('',( #14970 ) ) ;
#37108 = CARTESIAN_POINT ( 'NONE',  ( 10.49180330207988554, 18.23678832236204883, -26.15052258653890149 ) ) ;
#37109 = CARTESIAN_POINT ( 'NONE',  ( 9.303655249773111535, 10.73386218874820663, 7.500000000000000888 ) ) ;
#37110 = ORIENTED_EDGE ( 'NONE', *, *, #17569, .F. ) ;
#37112 = DIRECTION ( 'NONE',  ( 0.000000000000000000, -0.5778781230733920360, -0.8161230758122046680 ) ) ;
#37111 = CARTESIAN_POINT ( 'NONE',  ( -16.84514298104724617, 16.73865939197028396, -15.83090985262360739 ) ) ;
#37113 = CARTESIAN_POINT ( 'NONE',  ( 8.796116341590819232, 23.42450908139080568, 9.000000000000001776 ) ) ;
#37114 = CIRCLE ( 'NONE', #29983, 0.5000000000000004441 ) ;
#37115 = CARTESIAN_POINT ( 'NONE',  ( 15.48852768438595362, -26.74270545139661337, -5.000000000000000888 ) ) ;
#37116 = CARTESIAN_POINT ( 'NONE',  ( -12.29725303649800594, -16.76881851035475890, -27.24954791347179395 ) ) ;
#37117 = DIRECTION ( 'NONE',  ( 1.000000000000000000, 0.000000000000000000, 0.000000000000000000 ) ) ;
#37118 = CARTESIAN_POINT ( 'NONE',  ( 12.92139572017179461, 21.66467470877940826, -17.43601754788530656 ) ) ;
#37119 = ORIENTED_EDGE ( 'NONE', *, *, #38079, .T. ) ;
#37120 = DIRECTION ( 'NONE',  ( 0.000000000000000000, 0.000000000000000000, 1.000000000000000000 ) ) ;
#37121 = CARTESIAN_POINT ( 'NONE',  ( -15.33721547441370170, -26.62960585016953985, -6.417084653855770426 ) ) ;
#37122 = CARTESIAN_POINT ( 'NONE',  ( -36.26963650278440099, -7.248637393401118345, 14.53008259253934220 ) ) ;
#37123 = CARTESIAN_POINT ( 'NONE',  ( -25.99964108865075829, -21.70810690337949111, -12.01446658603936868 ) ) ;
#37124 = CARTESIAN_POINT ( 'NONE',  ( -0.2709479841607694284, -20.69534288464836180, -26.62127205292360443 ) ) ;
#37125 = CARTESIAN_POINT ( 'NONE',  ( 15.16228493941223476, 25.10766862421788659, -9.719789186029419881 ) ) ;
#37126 = CARTESIAN_POINT ( 'NONE',  ( 19.31451997534437837, 9.825694766287540460, -21.17302188312822508 ) ) ;
#37127 = DIRECTION ( 'NONE',  ( 1.000000000000000000, -4.163336342344304841E-14, 0.000000000000000000 ) ) ;
#37128 = CARTESIAN_POINT ( 'NONE',  ( -3.578418739405598181, 25.33586860667721297, -19.68557914504843964 ) ) ;
#37129 = ORIENTED_EDGE ( 'NONE', *, *, #18958, .T. ) ;
#37130 = CARTESIAN_POINT ( 'NONE',  ( -27.98118135240622095, -5.186583525525977123, -15.94789710196255150 ) ) ;
#37131 = ADVANCED_FACE ( 'NONE', ( #6576 ), #34426, .F. ) ;
#37132 = CARTESIAN_POINT ( 'NONE',  ( -18.50792845154007438, 22.38468038563317108, 12.73282698326878304 ) ) ;
#37133 = ORIENTED_EDGE ( 'NONE', *, *, #15603, .F. ) ;
#37134 = CARTESIAN_POINT ( 'NONE',  ( -19.48557158514985588, -11.25000000000002309, 3.000000000000000000 ) ) ;
#37135 = CARTESIAN_POINT ( 'NONE',  ( 23.20071485358947783, -14.64063822049746477, 23.00000000000000711 ) ) ;
#37136 = CARTESIAN_POINT ( 'NONE',  ( -29.78651012600981218, 0.8611516314391640670, -7.362443450658839872 ) ) ;
#37137 = CARTESIAN_POINT ( 'NONE',  ( 20.25988315325368205, -6.799842207391387561, -25.67160698062978952 ) ) ;
#37138 = ORIENTED_EDGE ( 'NONE', *, *, #27423, .T. ) ;
#37139 = CIRCLE ( 'NONE', #24807, 0.5000000000000004441 ) ;
#37140 = DIRECTION ( 'NONE',  ( 0.000000000000000000, 0.000000000000000000, -1.000000000000000000 ) ) ;
#37141 = EDGE_LOOP ( 'NONE', ( #14395, #7781 ) ) ;
#37142 = DIRECTION ( 'NONE',  ( 0.8090169943749426773, -0.5877852522924796874, -0.000000000000000000 ) ) ;
#37143 = CARTESIAN_POINT ( 'NONE',  ( 22.48079666814720667, 18.61591633950847324, 11.00000000000000000 ) ) ;
#37144 = AXIS2_PLACEMENT_3D ( 'NONE', #13682, #35427, #22415 ) ;
#37145 = DIRECTION ( 'NONE',  ( -0.000000000000000000, -0.000000000000000000, -1.000000000000000000 ) ) ;
#37146 = ORIENTED_EDGE ( 'NONE', *, *, #8143, .F. ) ;
#37147 = CARTESIAN_POINT ( 'NONE',  ( -2.236895112781582817, 20.38702974553298830, -29.21783655675459102 ) ) ;
#37148 = DIRECTION ( 'NONE',  ( -0.7431448254773953543, -0.6691306063588570163, 0.000000000000000000 ) ) ;
#37149 = DIRECTION ( 'NONE',  ( 0.000000000000000000, 0.000000000000000000, 1.000000000000000000 ) ) ;
#37150 = EDGE_CURVE ( 'NONE', #21371, #22721, #33837, .T. ) ;
#37151 = CARTESIAN_POINT ( 'NONE',  ( 12.64210930126479937, 24.20081211342298744, 12.00000000000000000 ) ) ;
#37152 = CARTESIAN_POINT ( 'NONE',  ( 19.49879619062026137, -14.97211638113389398, -20.74291969904744803 ) ) ;
#37153 = EDGE_CURVE ( 'NONE', #31037, #29721, #21628, .T. ) ;
#37154 = CARTESIAN_POINT ( 'NONE',  ( 18.53780643774816994, 14.90836240266203738, -13.87402227025345525 ) ) ;
#37155 = CARTESIAN_POINT ( 'NONE',  ( 12.95609944032581673, 31.22932257616612972, -7.688727340897671958 ) ) ;
#37156 = ORIENTED_EDGE ( 'NONE', *, *, #19689, .T. ) ;
#37157 = CARTESIAN_POINT ( 'NONE',  ( -17.63234478075006706, 10.48641262593123535, -29.42979450428692090 ) ) ;
#37158 = CARTESIAN_POINT ( 'NONE',  ( -4.817371740575545402, 23.83900317890010001, 23.00000000000000000 ) ) ;
#37159 = CARTESIAN_POINT ( 'NONE',  ( 10.92341448429028361, -19.97047823036292158, -21.60572769884808153 ) ) ;
#37160 = LINE ( 'NONE', #21911, #20413 ) ;
#37161 = CARTESIAN_POINT ( 'NONE',  ( 15.72991998290128990, -16.18894361744929000, -20.11584339644706887 ) ) ;
#37162 = CARTESIAN_POINT ( 'NONE',  ( -10.72501808743014884, 33.00580893829974372, 10.49999999999999645 ) ) ;
#37163 = AXIS2_PLACEMENT_3D ( 'NONE', #34205, #33816, #30566 ) ;
#37164 = CARTESIAN_POINT ( 'NONE',  ( -11.66180094259661182, 18.93490399102544686, -22.73092985986360404 ) ) ;
#37165 = CARTESIAN_POINT ( 'NONE',  ( -24.43784849675204285, -25.81124019920631696, -8.053843953535672284 ) ) ;
#37166 = CARTESIAN_POINT ( 'NONE',  ( 10.37471708997861164, -24.99497222897499782, -9.781170498600573637 ) ) ;
#37167 = AXIS2_PLACEMENT_3D ( 'NONE', #16530, #28913, #12611 ) ;
#37168 = CARTESIAN_POINT ( 'NONE',  ( 11.58426073497340880, 31.66040656113755603, 10.49999999999999822 ) ) ;
#37169 = ORIENTED_EDGE ( 'NONE', *, *, #16006, .T. ) ;
#37170 = CARTESIAN_POINT ( 'NONE',  ( -9.313421446828321848, 28.11428578405463341, -14.94527526474085732 ) ) ;
#37171 = DIRECTION ( 'NONE',  ( -0.4999999999999933942, 0.8660254037844425934, 0.000000000000000000 ) ) ;
#37172 = ADVANCED_FACE ( 'NONE', ( #2747 ), #24815, .T. ) ;
#37173 = CARTESIAN_POINT ( 'NONE',  ( -8.169448529985462670, 9.961039561530412811, 10.49999999999999467 ) ) ;
#37174 = VECTOR ( 'NONE', #26682, 1000.000000000000114 ) ;
#37175 = CARTESIAN_POINT ( 'NONE',  ( -9.331903152615897312, 11.35703883385580859, 10.49999999999999822 ) ) ;
#37176 = ORIENTED_EDGE ( 'NONE', *, *, #37229, .T. ) ;
#37177 = CARTESIAN_POINT ( 'NONE',  ( 25.85566401745649756, 0.3314906535464867132, -16.44492392060781327 ) ) ;
#37178 = EDGE_CURVE ( 'NONE', #21244, #17938, #35326, .T. ) ;
#37179 = DIRECTION ( 'NONE',  ( -0.2079116908177533474, 0.9781476007338067991, -0.000000000000000000 ) ) ;
#37180 = EDGE_CURVE ( 'NONE', #481, #14680, #9134, .T. ) ;
#37181 = CARTESIAN_POINT ( 'NONE',  ( 4.527363138135212850, 36.35651410043141141, 7.000000000000000000 ) ) ;
#37182 = ORIENTED_EDGE ( 'NONE', *, *, #25517, .T. ) ;
#37183 = CARTESIAN_POINT ( 'NONE',  ( -20.60872544724836786, 0.8785077229891553596, -28.07890803345969388 ) ) ;
#37184 = DIRECTION ( 'NONE',  ( -0.1470157664651947915, 0.6916548014802283983, -0.7071067811865455743 ) ) ;
#37185 = AXIS2_PLACEMENT_3D ( 'NONE', #7410, #10066, #19817 ) ;
#37186 = VERTEX_POINT ( 'NONE', #30978 ) ;
#37187 = CARTESIAN_POINT ( 'NONE',  ( 27.13811364924229963, -5.609222319042479477, -16.88217377438804689 ) ) ;
#37188 = EDGE_CURVE ( 'NONE', #1779, #13010, #3144, .T. ) ;
#37189 = EDGE_LOOP ( 'NONE', ( #17912, #33519, #31639, #3695, #28861 ) ) ;
#37190 = CARTESIAN_POINT ( 'NONE',  ( -5.682704777077058900, 39.36960561607953935, 12.73282698324852902 ) ) ;
#37191 = CARTESIAN_POINT ( 'NONE',  ( -11.87696897075269042, -16.96707895830268598, 20.82122704794084456 ) ) ;
#37192 = DIRECTION ( 'NONE',  ( 0.000000000000000000, 0.000000000000000000, 1.000000000000000000 ) ) ;
#37193 = CARTESIAN_POINT ( 'NONE',  ( -2.325696902088870921, 33.04389473401317900, 19.99202127657102679 ) ) ;
#37194 = AXIS2_PLACEMENT_3D ( 'NONE', #7058, #38144, #16415 ) ;
#37195 = CYLINDRICAL_SURFACE ( 'NONE', #10349, 1.000000000000000888 ) ;
#37196 = ORIENTED_EDGE ( 'NONE', *, *, #15393, .T. ) ;
#37197 = CARTESIAN_POINT ( 'NONE',  ( -13.63581098909220479, 27.45627467658446008, 7.499999999999993783 ) ) ;
#37198 = CARTESIAN_POINT ( 'NONE',  ( -10.54700836463452340, 22.39697303105802106, 10.50000000000000000 ) ) ;
#37199 = DIRECTION ( 'NONE',  ( 1.000000000000000000, 0.000000000000000000, 0.000000000000000000 ) ) ;
#37200 = EDGE_CURVE ( 'NONE', #31380, #18974, #18788, .T. ) ;
#37201 = EDGE_CURVE ( 'NONE', #24961, #2306, #9254, .T. ) ;
#37202 = LINE ( 'NONE', #35554, #35734 ) ;
#37203 = EDGE_CURVE ( 'NONE', #2033, #23095, #34620, .T. ) ;
#37204 = CARTESIAN_POINT ( 'NONE',  ( 7.308504912602463932, 28.32893145372440813, -15.82008540585032641 ) ) ;
#37205 = AXIS2_PLACEMENT_3D ( 'NONE', #1737, #33029, #23864 ) ;
#37206 = CARTESIAN_POINT ( 'NONE',  ( 14.21603707476194067, -21.19223970495677634, -18.18584086863970128 ) ) ;
#37207 =( LENGTH_UNIT ( ) NAMED_UNIT ( * ) SI_UNIT ( .MILLI., .METRE. ) );
#37208 = FACE_OUTER_BOUND ( 'NONE', #25516, .T. ) ;
#37209 = CARTESIAN_POINT ( 'NONE',  ( -4.987329993433320396E-14, 13.65543219052647927, 9.000000000000001776 ) ) ;
#37210 = EDGE_LOOP ( 'NONE', ( #31519, #35335, #26190, #1688 ) ) ;
#37211 = CARTESIAN_POINT ( 'NONE',  ( -13.78507581919008196, 23.36291329981870035, -14.47800459695361397 ) ) ;
#37212 = CIRCLE ( 'NONE', #22939, 1.000000000000000000 ) ;
#37213 = CARTESIAN_POINT ( 'NONE',  ( -31.65150718622412995, -20.14649908112938803, 17.42190598798354628 ) ) ;
#37214 = CARTESIAN_POINT ( 'NONE',  ( 9.346475367005044887, -18.24555389153483631, -29.35143642865414648 ) ) ;
#37215 = LINE ( 'NONE', #21375, #6843 ) ;
#37216 = ORIENTED_EDGE ( 'NONE', *, *, #34083, .T. ) ;
#37217 = ORIENTED_EDGE ( 'NONE', *, *, #29513, .F. ) ;
#37218 = CARTESIAN_POINT ( 'NONE',  ( -13.78620412469754974, 30.29238551392001000, -6.816998145928632624 ) ) ;
#37219 = CARTESIAN_POINT ( 'NONE',  ( -11.05369788186578539, -17.27790053512912039, -29.31532796641473837 ) ) ;
#37220 = EDGE_CURVE ( 'NONE', #24016, #32625, #22216, .T. ) ;
#37221 = FACE_BOUND ( 'NONE', #27035, .T. ) ;
#37222 = CIRCLE ( 'NONE', #24255, 16.00000000000000000 ) ;
#37223 = ORIENTED_EDGE ( 'NONE', *, *, #20816, .T. ) ;
#37224 = CARTESIAN_POINT ( 'NONE',  ( -33.72291166692595255, -10.47593345224562533, -9.784983549797274804 ) ) ;
#37225 = CARTESIAN_POINT ( 'NONE',  ( -14.42315031391927604, -25.58824056110956846, -10.18640137108187105 ) ) ;
#37226 = CARTESIAN_POINT ( 'NONE',  ( 14.84160187385922036, 20.32586711126977619, 7.500000000000010658 ) ) ;
#37227 = ORIENTED_EDGE ( 'NONE', *, *, #35456, .F. ) ;
#37228 = CARTESIAN_POINT ( 'NONE',  ( 23.84616085791028439, 0.7114667219658915576, -19.52213106094174933 ) ) ;
#37229 = EDGE_CURVE ( 'NONE', #13902, #12954, #25868, .T. ) ;
#37230 = CARTESIAN_POINT ( 'NONE',  ( -14.36830325120615548, 20.48707633493503621, 9.000000000000001776 ) ) ;
#37231 = LINE ( 'NONE', #9002, #25130 ) ;
#37232 = EDGE_LOOP ( 'NONE', ( #826, #356 ) ) ;
#37233 = CARTESIAN_POINT ( 'NONE',  ( -28.36098518925343015, 0.1130484564961234811, -12.54774101850605206 ) ) ;
#37234 = EDGE_LOOP ( 'NONE', ( #9587, #39904, #12186, #38734 ) ) ;
#37235 = CARTESIAN_POINT ( 'NONE',  ( 22.53479768705193109, -0.8417541303772992922, -22.54520765563958307 ) ) ;
#37236 = VECTOR ( 'NONE', #39188, 1000.000000000000000 ) ;
#37237 = CARTESIAN_POINT ( 'NONE',  ( 10.50003573332661411, -17.62042850385381243, -30.00000000000000000 ) ) ;
#37238 = CARTESIAN_POINT ( 'NONE',  ( 32.46232039045683138, -18.74212941594987214, 17.42190598798392642 ) ) ;
#37239 = ORIENTED_EDGE ( 'NONE', *, *, #30649, .T. ) ;
#37240 = CARTESIAN_POINT ( 'NONE',  ( -20.19374099270470779, 4.300116008667979273, -27.62586759252641144 ) ) ;
#37241 = CARTESIAN_POINT ( 'NONE',  ( -14.61143855090110932, 25.89393895760251851, 7.097463131219505783 ) ) ;
#37242 = CARTESIAN_POINT ( 'NONE',  ( 4.817371740575538297, 23.83900317890011067, 20.99999999999999645 ) ) ;
#37243 = VECTOR ( 'NONE', #7668, 1000.000000000000000 ) ;
#37244 = FACE_OUTER_BOUND ( 'NONE', #13344, .T. ) ;
#37245 = CARTESIAN_POINT ( 'NONE',  ( 8.118377661053324701, 10.47536095541698486, 7.000000000000000000 ) ) ;
#37246 = B_SPLINE_SURFACE_WITH_KNOTS ( 'NONE', 1, 3, ( 
 ( #17428, #38947, #36501, #8264, #23904, #11718, #35902, #36306, #33469, #8469 ),
 ( #20263, #11119, #11322, #39139, #23503, #7858, #5611, #23705, #29598, #4818 ) ),
 .UNSPECIFIED., .F., .F., .F.,
 ( 2, 2 ),
 ( 4, 2, 2, 2, 4 ),
 ( 0.000000000000000000, 1.000000000000000000 ),
 ( 1.875797233020323640, 2.268496314719047557, 2.661195396417771697, 3.053894478116495836, 3.446593559815219976 ),
 .UNSPECIFIED. ) ;
#37247 = CARTESIAN_POINT ( 'NONE',  ( -6.330077540933487512, 17.71145523154927659, 12.00000000000000000 ) ) ;
#37248 = CARTESIAN_POINT ( 'NONE',  ( 3.835130509701798918, 15.55077355964573904, 6.000000000000000000 ) ) ;
#37249 = CARTESIAN_POINT ( 'NONE',  ( -19.55289733891971693, 6.410511261044660181, -28.26509928457950949 ) ) ;
#37250 = LINE ( 'NONE', #34404, #31966 ) ;
#37251 = CYLINDRICAL_SURFACE ( 'NONE', #8434, 1.000000000000000000 ) ;
#37252 = CARTESIAN_POINT ( 'NONE',  ( 14.35507674797322153, -14.94651742297148722, -27.81134915278669340 ) ) ;
#37253 = CARTESIAN_POINT ( 'NONE',  ( -2.140527761532693418, 7.619874298175171035, 11.00000000000000000 ) ) ;
#37254 = CARTESIAN_POINT ( 'NONE',  ( 10.79262732167511274, 17.48354943385782079, -28.69806840933970804 ) ) ;
#37255 = VERTEX_POINT ( 'NONE', #7180 ) ;
#37256 = AXIS2_PLACEMENT_3D ( 'NONE', #32860, #5014, #29800 ) ;
#37257 = CARTESIAN_POINT ( 'NONE',  ( -12.82984808660655318, 16.00373636590108362, -30.00000000000000355 ) ) ;
#37258 = CARTESIAN_POINT ( 'NONE',  ( -28.60147806546170202, -12.08038679647151348, 20.50957957746030758 ) ) ;
#37259 = CYLINDRICAL_SURFACE ( 'NONE', #39940, 19.99999999999993250 ) ;
#37260 = CARTESIAN_POINT ( 'NONE',  ( 11.01299302568612859, 17.29057472414998742, -30.00000000000000000 ) ) ;
#37261 = VERTEX_POINT ( 'NONE', #23027 ) ;
#37262 = DIRECTION ( 'NONE',  ( 0.000000000000000000, 0.000000000000000000, 1.000000000000000000 ) ) ;
#37263 = VERTEX_POINT ( 'NONE', #19578 ) ;
#37265 = DIRECTION ( 'NONE',  ( 0.000000000000000000, 0.000000000000000000, 1.000000000000000000 ) ) ;
#37264 = CARTESIAN_POINT ( 'NONE',  ( -10.92223089246044587, 17.60308047634757500, -27.43605944492403381 ) ) ;
#37266 = CARTESIAN_POINT ( 'NONE',  ( -10.97957011535166494, -19.95710388766885401, -21.59818507530883025 ) ) ;
#37267 = CARTESIAN_POINT ( 'NONE',  ( 12.74038105676654453, 14.56698729810772264, 10.50000000000000178 ) ) ;
#37268 = ORIENTED_EDGE ( 'NONE', *, *, #29419, .F. ) ;
#37269 = CARTESIAN_POINT ( 'NONE',  ( -34.41005778243852120, -16.71535200144834832, -6.277988090640136853 ) ) ;
#37270 = VECTOR ( 'NONE', #36508, 1000.000000000000114 ) ;
#37271 = CARTESIAN_POINT ( 'NONE',  ( -7.523214604281919904, -19.21852453499634450, -28.17917537356595403 ) ) ;
#37272 = DIRECTION ( 'NONE',  ( -0.5877852522924796874, -0.8090169943749426773, 0.000000000000000000 ) ) ;
#37273 = CARTESIAN_POINT ( 'NONE',  ( 16.83483527457651974, 22.12433461383112032, -6.427118072085295175 ) ) ;
#37274 = ORIENTED_EDGE ( 'NONE', *, *, #31204, .T. ) ;
#37275 = CARTESIAN_POINT ( 'NONE',  ( 19.90454223993690874, 5.930672848293738753, -26.54186067485865053 ) ) ;
#37276 = DIRECTION ( 'NONE',  ( -0.000000000000000000, -0.000000000000000000, -1.000000000000000000 ) ) ;
#37277 = DIRECTION ( 'NONE',  ( 0.000000000000000000, 0.000000000000000000, -1.000000000000000000 ) ) ;
#37278 = CARTESIAN_POINT ( 'NONE',  ( 4.100636323082810009, 29.29593658752792962, 13.00000000000000178 ) ) ;
#37279 = ORIENTED_EDGE ( 'NONE', *, *, #8863, .F. ) ;
#37280 = CARTESIAN_POINT ( 'NONE',  ( -31.08811179967121419, -0.4156326309829680432, -6.876971461052154844 ) ) ;
#37281 = AXIS2_PLACEMENT_3D ( 'NONE', #36562, #21124, #8936 ) ;
#37282 = CARTESIAN_POINT ( 'NONE',  ( 20.48743909015156106, 0.7225425954259894201, -29.34587392400671391 ) ) ;
#37283 = CARTESIAN_POINT ( 'NONE',  ( -34.03019007953001562, -25.06168574969261797, 11.00000000000000000 ) ) ;
#37284 = CARTESIAN_POINT ( 'NONE',  ( 27.31307666897629360, -8.451821295062190487, 20.69868183039763565 ) ) ;
#37285 = ORIENTED_EDGE ( 'NONE', *, *, #24651, .F. ) ;
#37286 = AXIS2_PLACEMENT_3D ( 'NONE', #39101, #16573, #38907 ) ;
#37287 = CARTESIAN_POINT ( 'NONE',  ( -15.72991998290134141, -16.18894361744923316, -20.11584339644716479 ) ) ;
#37288 = LINE ( 'NONE', #5812, #27091 ) ;
#37289 = AXIS2_PLACEMENT_3D ( 'NONE', #27449, #2873, #15461 ) ;
#37290 = ORIENTED_EDGE ( 'NONE', *, *, #442, .T. ) ;
#37291 = CARTESIAN_POINT ( 'NONE',  ( -6.576253646258509278, 14.29921418520934218, 10.50000000000000000 ) ) ;
#37292 = CARTESIAN_POINT ( 'NONE',  ( -30.33922525721619223, 6.243664897686377557, 11.00000000000000000 ) ) ;
#37293 = CARTESIAN_POINT ( 'NONE',  ( 12.97403502154100607, 15.97168783648697499, 10.66666666666666252 ) ) ;
#37294 = CARTESIAN_POINT ( 'NONE',  ( 2.684628480821892982, 37.27707400732953857, -8.408764988529911832 ) ) ;
#37295 = CARTESIAN_POINT ( 'NONE',  ( 9.788939752379329562, 23.27376113029817617, 6.000000000000000000 ) ) ;
#37296 = EDGE_CURVE ( 'NONE', #11885, #27294, #35171, .T. ) ;
#37297 = LINE ( 'NONE', #9471, #39621 ) ;
#37298 = DIRECTION ( 'NONE',  ( 1.000000000000000000, 0.000000000000000000, 0.000000000000000000 ) ) ;
#37299 = FACE_OUTER_BOUND ( 'NONE', #7405, .T. ) ;
#37300 = DIRECTION ( 'NONE',  ( -0.000000000000000000, -0.000000000000000000, -1.000000000000000000 ) ) ;
#37301 =( NAMED_UNIT ( * ) PLANE_ANGLE_UNIT ( ) SI_UNIT ( $, .RADIAN. ) );
#37302 = VECTOR ( 'NONE', #1250, 1000.000000000000000 ) ;
#37303 = CARTESIAN_POINT ( 'NONE',  ( 10.35162965265407387, 18.32793675510878728, -26.13581186062965145 ) ) ;
#37304 = DIRECTION ( 'NONE',  ( 1.000000000000000000, 0.000000000000000000, 0.000000000000000000 ) ) ;
#37305 = VERTEX_POINT ( 'NONE', #9838 ) ;
#37307 = LINE ( 'NONE', #11930, #24610 ) ;
#37306 = CARTESIAN_POINT ( 'NONE',  ( -17.05325914272468779, 17.02370371989225006, -14.81479654505746169 ) ) ;
#37308 = ADVANCED_FACE ( 'NONE', ( #35220 ), #19174, .F. ) ;
#37309 = CARTESIAN_POINT ( 'NONE',  ( 12.97058434440062769, 15.58877990640313449, 10.96580508970283141 ) ) ;
#37310 = CARTESIAN_POINT ( 'NONE',  ( 9.495448100151719473, -18.16828483302926145, -29.34839842954884048 ) ) ;
#37311 = ADVANCED_FACE ( 'NONE', ( #16540 ), #7587, .T. ) ;
#37312 = CARTESIAN_POINT ( 'NONE',  ( -17.08966005492841944, -22.85233455301158756, -15.10154554800658744 ) ) ;
#37313 = CARTESIAN_POINT ( 'NONE',  ( 11.00500201062592076, 17.34882336543233450, -28.70691125584460934 ) ) ;
#37314 = CARTESIAN_POINT ( 'NONE',  ( 11.46769351692955752, 18.45166467387952380, -23.85133428991321125 ) ) ;
#37315 = ORIENTED_EDGE ( 'NONE', *, *, #6394, .F. ) ;
#37316 = VECTOR ( 'NONE', #8027, 1000.000000000000000 ) ;
#37317 = DIRECTION ( 'NONE',  ( 1.000000000000000000, 0.000000000000000000, 0.000000000000000000 ) ) ;
#37318 = CARTESIAN_POINT ( 'NONE',  ( -14.27994367031277001, -25.05694730131601133, -11.60121664921379114 ) ) ;
#37319 = CARTESIAN_POINT ( 'NONE',  ( -35.97875289183299685, -7.317948980264791459, 15.13084544680133270 ) ) ;
#37320 = CIRCLE ( 'NONE', #21738, 1.000000000000000000 ) ;
#37321 = CONICAL_SURFACE ( 'NONE', #19804, 1.000000000000002665, 0.7853981633974579379 ) ;
#37322 = CARTESIAN_POINT ( 'NONE',  ( -31.58328445775233106, -21.78494312990649462, -5.000000000000002665 ) ) ;
#37323 = CARTESIAN_POINT ( 'NONE',  ( -2.574564127703440786, -24.67429484068291146, -7.426918231604072496 ) ) ;
#37324 = CARTESIAN_POINT ( 'NONE',  ( 14.72309051804893798, 24.45547455918983459, -11.61434635058594900 ) ) ;
#37325 = CARTESIAN_POINT ( 'NONE',  ( 18.23997498585743671, 9.357756550322328337, -29.42875180487423847 ) ) ;
#37326 = DIRECTION ( 'NONE',  ( -1.000000000000000000, -1.224646799147353947E-16, 0.000000000000000000 ) ) ;
#37327 = ORIENTED_EDGE ( 'NONE', *, *, #3320, .F. ) ;
#37328 = CARTESIAN_POINT ( 'NONE',  ( -33.31713789998030251, -3.466154907495874848, -6.811614906419716675 ) ) ;
#37329 = CARTESIAN_POINT ( 'NONE',  ( -27.14644468510207531, -3.730463242937111179, 19.99202127657103389 ) ) ;
#37330 = ORIENTED_EDGE ( 'NONE', *, *, #39241, .T. ) ;
#37331 = DIRECTION ( 'NONE',  ( 1.000000000000000000, 0.000000000000000000, 0.000000000000000000 ) ) ;
#37332 = EDGE_CURVE ( 'NONE', #13142, #6492, #40135, .T. ) ;
#37333 = CARTESIAN_POINT ( 'NONE',  ( 18.23649648353767461, -16.09146789626181118, 23.00000000000000000 ) ) ;
#37334 = EDGE_CURVE ( 'NONE', #18400, #5055, #33259, .T. ) ;
#37335 = CARTESIAN_POINT ( 'NONE',  ( -29.73804506707628192, 0.6556055609695065067, -8.304321593376053912 ) ) ;
#37336 = CARTESIAN_POINT ( 'NONE',  ( 35.42505292462669786, -13.05524145712385042, -5.000000000000000000 ) ) ;
#37337 = VECTOR ( 'NONE', #23583, 999.9999999999998863 ) ;
#37338 = CARTESIAN_POINT ( 'NONE',  ( 22.63195743522303260, -28.51917808483202066, 13.92931973827781711 ) ) ;
#37339 = ORIENTED_EDGE ( 'NONE', *, *, #31335, .T. ) ;
#37340 = DIRECTION ( 'NONE',  ( 1.000000000000000000, 0.000000000000000000, 0.000000000000000000 ) ) ;
#37341 = ORIENTED_EDGE ( 'NONE', *, *, #31848, .F. ) ;
#37342 = CARTESIAN_POINT ( 'NONE',  ( -2.229437847141422679, 24.50739181907689712, 6.000000000000000000 ) ) ;
#37343 = CARTESIAN_POINT ( 'NONE',  ( -14.26585111513660031, 17.86474508437623143, 12.00000000000000000 ) ) ;
#37344 = AXIS2_PLACEMENT_3D ( 'NONE', #32411, #14109, #4971 ) ;
#37345 = VECTOR ( 'NONE', #8993, 1000.000000000000000 ) ;
#37346 = FACE_OUTER_BOUND ( 'NONE', #30582, .T. ) ;
#37347 = ORIENTED_EDGE ( 'NONE', *, *, #13870, .F. ) ;
#37348 = CARTESIAN_POINT ( 'NONE',  ( -3.330156562440208745, 29.86612940616478440, -15.70309549552822226 ) ) ;
#37349 = CARTESIAN_POINT ( 'NONE',  ( 8.412270287199559604, 10.07085245822951158, 10.63089969389957545 ) ) ;
#37350 = DIRECTION ( 'NONE',  ( 0.000000000000000000, 0.000000000000000000, 1.000000000000000000 ) ) ;
#37351 = LINE ( 'NONE', #6852, #22776 ) ;
#37352 = EDGE_CURVE ( 'NONE', #7643, #10090, #3387, .T. ) ;
#37353 = CARTESIAN_POINT ( 'NONE',  ( -10.81260707898136708, 32.90853150812170469, 10.49999999999999822 ) ) ;
#37354 = CARTESIAN_POINT ( 'NONE',  ( 12.83000963327528865, 28.50739036967297224, -11.36264415545698370 ) ) ;
#37355 = VERTEX_POINT ( 'NONE', #32179 ) ;
#37356 = CARTESIAN_POINT ( 'NONE',  ( -18.62251848404639176, 10.14620980242720272, -23.33001570770051103 ) ) ;
#37357 = CARTESIAN_POINT ( 'NONE',  ( 10.37659644360199707, 39.73422260060728206, 23.00000000000000000 ) ) ;
#37358 = CARTESIAN_POINT ( 'NONE',  ( 15.36705230571556946, -26.32838276033183789, -8.290462328652061785 ) ) ;
#37359 = DIRECTION ( 'NONE',  ( 0.9945218953682746221, 0.1045284632676422437, 0.000000000000000000 ) ) ;
#37360 = CARTESIAN_POINT ( 'NONE',  ( 14.50667584134738775, 25.04428483107196968, -11.59352418477084434 ) ) ;
#37361 = CARTESIAN_POINT ( 'NONE',  ( -26.31271763591399804, -28.25584584496044727, -14.26382729546507555 ) ) ;
#37362 = CARTESIAN_POINT ( 'NONE',  ( 9.427394655416197367, 11.16786596286755362, 10.49999999999999822 ) ) ;
#37363 = CARTESIAN_POINT ( 'NONE',  ( -13.19593879056965591, 22.26071678948836308, -16.44094010185055765 ) ) ;
#37364 = CARTESIAN_POINT ( 'NONE',  ( -14.57624227410516404, -14.53651728905030183, -28.50876045855337892 ) ) ;
#37365 = CARTESIAN_POINT ( 'NONE',  ( 13.06131125295109996, -26.10018571120846431, -6.421009571025454221 ) ) ;
#37366 = CARTESIAN_POINT ( 'NONE',  ( 15.38983201598744266, 26.43745849338104037, -6.888277659600019476 ) ) ;
#37367 = CARTESIAN_POINT ( 'NONE',  ( 17.51558450279301837, -11.83370107486374501, -26.26684009027794175 ) ) ;
#37368 = CARTESIAN_POINT ( 'NONE',  ( -9.625795778762141097, 10.95253033666833886, 10.49999999999999822 ) ) ;
#37369 = EDGE_LOOP ( 'NONE', ( #2238, #37619, #3358 ) ) ;
#37370 = CARTESIAN_POINT ( 'NONE',  ( -9.589722423178423938, 32.07510805956650302, -11.18595533578888279 ) ) ;
#37371 = CIRCLE ( 'NONE', #9473, 0.9999999999999986677 ) ;
#37372 = CARTESIAN_POINT ( 'NONE',  ( 0.9461134518049061359, 37.26099332938164821, 10.49999999999999467 ) ) ;
#37373 = LINE ( 'NONE', #37575, #31636 ) ;
#37374 = CIRCLE ( 'NONE', #30248, 15.00000000000000000 ) ;
#37375 = CYLINDRICAL_SURFACE ( 'NONE', #5958, 0.5000000000000004441 ) ;
#37376 = EDGE_LOOP ( 'NONE', ( #10803, #7081, #25390, #31049 ) ) ;
#37377 = CARTESIAN_POINT ( 'NONE',  ( 22.72129020795306786, 0.6420447253098271467, -21.62132452122856918 ) ) ;
#37378 = CARTESIAN_POINT ( 'NONE',  ( -14.42035624161473883, 26.65972665747678860, 10.49999999999999822 ) ) ;
#37379 = CIRCLE ( 'NONE', #6228, 1.000000000000000000 ) ;
#37380 = CARTESIAN_POINT ( 'NONE',  ( 75.15099915297797395, 43.38844959084117647, 23.00000000000000000 ) ) ;
#37381 = EDGE_CURVE ( 'NONE', #11157, #15047, #33283, .T. ) ;
#37382 = ORIENTED_EDGE ( 'NONE', *, *, #13287, .T. ) ;
#37383 = CARTESIAN_POINT ( 'NONE',  ( -28.31117062388397443, 0.1748750734513740968, -12.55189785114625245 ) ) ;
#37384 = CARTESIAN_POINT ( 'NONE',  ( -14.09933648065464062, 26.02968990214173317, 7.499999999999993783 ) ) ;
#37385 = ORIENTED_EDGE ( 'NONE', *, *, #35993, .F. ) ;
#37386 = CARTESIAN_POINT ( 'NONE',  ( 34.68475117796653251, -6.257323052730294322, -5.891097102607844249 ) ) ;
#37387 = VERTEX_POINT ( 'NONE', #4135 ) ;
#37388 = CARTESIAN_POINT ( 'NONE',  ( -16.63496159152044385, 29.12310921430476185, 12.73282698324768880 ) ) ;
#37389 = CARTESIAN_POINT ( 'NONE',  ( 11.48173768534036121, 32.16538668264416145, 11.00000000000000000 ) ) ;
#37390 = CARTESIAN_POINT ( 'NONE',  ( -32.33143948541797386, 1.358872982501901472, 23.00000000000000000 ) ) ;
#37391 = CARTESIAN_POINT ( 'NONE',  ( -10.90978760418654758, 28.29414058874172255, 19.27171037444159296 ) ) ;
#37392 = DIRECTION ( 'NONE',  ( 0.8660254037844362651, -0.5000000000000041078, 0.000000000000000000 ) ) ;
#37393 = ORIENTED_EDGE ( 'NONE', *, *, #17865, .T. ) ;
#37394 = CARTESIAN_POINT ( 'NONE',  ( 3.992867117591238468, 8.524771480177550487, 10.49999999999999822 ) ) ;
#37395 = CARTESIAN_POINT ( 'NONE',  ( -7.292293556685349287, 19.17084528979847491, -29.99999999999998224 ) ) ;
#37396 = DIRECTION ( 'NONE',  ( 0.000000000000000000, 0.000000000000000000, 1.000000000000000000 ) ) ;
#37397 = DIRECTION ( 'NONE',  ( 1.000000000000000000, 0.000000000000000000, 0.000000000000000000 ) ) ;
#37398 = EDGE_CURVE ( 'NONE', #12832, #24820, #13147, .T. ) ;
#37399 = CARTESIAN_POINT ( 'NONE',  ( 9.020565442340009454, 35.12981360116603469, -7.597900073285591915 ) ) ;
#37400 = CIRCLE ( 'NONE', #10145, 0.5000000000000000000 ) ;
#37401 = ADVANCED_FACE ( 'NONE', ( #13275 ), #25667, .F. ) ;
#37402 = CIRCLE ( 'NONE', #10150, 0.4999999999999998335 ) ;
#37403 = ADVANCED_FACE ( 'NONE', ( #38065 ), #29127, .T. ) ;
#37404 = CARTESIAN_POINT ( 'NONE',  ( 12.61212348447421228, -20.17736113527566744, -20.35657553128955755 ) ) ;
#37405 = SURFACE_STYLE_FILL_AREA ( #39845 ) ;
#37406 = CARTESIAN_POINT ( 'NONE',  ( -0.3582326297815359162, 33.31072022568110924, 12.00000000000000000 ) ) ;
#37407 = VERTEX_POINT ( 'NONE', #695 ) ;
#37408 = CARTESIAN_POINT ( 'NONE',  ( -11.63857042517895835, 18.30432797884460783, -23.87741341467080147 ) ) ;
#37409 = EDGE_CURVE ( 'NONE', #39304, #25736, #19647, .T. ) ;
#37410 = CARTESIAN_POINT ( 'NONE',  ( -30.60828605274471670, -21.42068866018134088, 17.42190598798391221 ) ) ;
#37411 = CARTESIAN_POINT ( 'NONE',  ( 10.14633863637189393, -19.19177985329903535, -23.86353120736796640 ) ) ;
#37412 = CARTESIAN_POINT ( 'NONE',  ( -2.587667106213709101, 35.31811204475769728, 6.000000000000000000 ) ) ;
#37413 = VERTEX_POINT ( 'NONE', #25463 ) ;
#37414 = ORIENTED_EDGE ( 'NONE', *, *, #3069, .T. ) ;
#37415 = CARTESIAN_POINT ( 'NONE',  ( -13.68010871116744731, 25.96172115623508603, -12.42778920982119928 ) ) ;
#37416 = CARTESIAN_POINT ( 'NONE',  ( -20.35363307782489883, -26.94962879673899181, -7.247870004610525108 ) ) ;
#37417 = FACE_BOUND ( 'NONE', #11130, .T. ) ;
#37418 = VERTEX_POINT ( 'NONE', #11053 ) ;
#37419 = CARTESIAN_POINT ( 'NONE',  ( -23.37192198891547434, -6.525024743817787076, -20.88787227384175083 ) ) ;
#37420 = CARTESIAN_POINT ( 'NONE',  ( -10.43671498305923606, -19.60464466685017015, -22.74714329939464363 ) ) ;
#37421 = LINE ( 'NONE', #9597, #170 ) ;
#37422 = ORIENTED_EDGE ( 'NONE', *, *, #8934, .T. ) ;
#37423 = CARTESIAN_POINT ( 'NONE',  ( 29.94912702968606055, 0.2658994707610922714, -8.770941407747322671 ) ) ;
#37424 = LINE ( 'NONE', #255, #2494 ) ;
#37425 = LINE ( 'NONE', #9601, #34210 ) ;
#37426 = ORIENTED_EDGE ( 'NONE', *, *, #17315, .F. ) ;
#37427 = EDGE_CURVE ( 'NONE', #5336, #12231, #32793, .T. ) ;
#37428 = CARTESIAN_POINT ( 'NONE',  ( -26.52412813069345532, 0.2470591091748601809, -15.44714408431404173 ) ) ;
#37430 = EDGE_CURVE ( 'NONE', #18869, #19973, #17556, .T. ) ;
#37429 = EDGE_LOOP ( 'NONE', ( #19055, #7752, #1774 ) ) ;
#37431 = CARTESIAN_POINT ( 'NONE',  ( 27.47914625674854250, -1.352420133889514764, -15.26936114680716550 ) ) ;
#37432 = VECTOR ( 'NONE', #23292, 1000.000000000000000 ) ;
#37433 = VECTOR ( 'NONE', #13884, 1000.000000000000000 ) ;
#37434 = CARTESIAN_POINT ( 'NONE',  ( 2.793143654148522170, -20.31935452177206969, -30.00000000000001421 ) ) ;
#37435 = CARTESIAN_POINT ( 'NONE',  ( 33.78274305024982738, -17.56282548559263290, 16.87380292611442556 ) ) ;
#37436 = EDGE_LOOP ( 'NONE', ( #24836, #28646, #4964 ) ) ;
#37437 = CARTESIAN_POINT ( 'NONE',  ( -21.90799695884349774, 4.299728261586824196, -20.92328423790911884 ) ) ;
#37438 = CARTESIAN_POINT ( 'NONE',  ( 9.343266739736582949, 17.68301270189218855, 10.50000000000000000 ) ) ;
#37439 = CARTESIAN_POINT ( 'NONE',  ( 3.456468065139975732, 26.15323006594241306, 20.99999999999999645 ) ) ;
#37440 = VECTOR ( 'NONE', #24906, 1000.000000000000114 ) ;
#37441 = DIRECTION ( 'NONE',  ( -0.8660254037844432595, -0.4999999999999921729, 0.000000000000000000 ) ) ;
#37442 = DIRECTION ( 'NONE',  ( -1.000000000000000000, 0.000000000000000000, 0.000000000000000000 ) ) ;
#37443 =( BOUNDED_SURFACE ( )  B_SPLINE_SURFACE ( 2, 3, ( 
 ( #17161, #6976, #35034, #29536, #903, #26488, #4140, #13485, #13687, #1711, #38477, #38276, #13280, #32184, #19997, #4346, #16752, #29132 ),
 ( #1305, #26076, #7592, #32394, #4550, #16952, #11254, #30141, #20404, #29738, #8199, #5750, #7993, #32799, #35834, #2514, #17765, #4956 ),
 ( #36039, #39076, #36435, #5352, #14295, #11850, #23841, #15093, #21194, #30343, #2115, #17362, #20998, #1917, #14495, #24239, #8806, #26687 ) ),
 .UNSPECIFIED., .F., .F., .T. ) 
 B_SPLINE_SURFACE_WITH_KNOTS ( ( 3, 3 ),
 ( 4, 2, 2, 2, 2, 2, 2, 2, 4 ),
 ( 0.000000000000000000, 1.000000000000000000 ),
 ( 2.365504664328351048, 2.690426355543287240, 3.015348046758223433, 3.340269737973159181, 3.665191429188095373, 3.990113120403031566, 4.315034811617967314, 4.639956502832903951, 4.964878194047839699 ),
 .UNSPECIFIED. ) 
 GEOMETRIC_REPRESENTATION_ITEM ( )  RATIONAL_B_SPLINE_SURFACE ( (
 ( 1.000000000000000000, 1.000000000000000000, 1.000000000000000000, 1.000000000000000000, 1.000000000000000000, 1.000000000000000000, 1.000000000000000000, 1.000000000000000000, 1.000000000000000000, 1.000000000000000000, 1.000000000000000000, 1.000000000000000000, 1.000000000000000000, 1.000000000000000000, 1.000000000000000000, 1.000000000000000000, 1.000000000000000000, 1.000000000000000000),
 ( 0.7071067811865475727, 0.7071067811865475727, 0.7071067811865474617, 0.7071067811865474617, 0.7071067811865474617, 0.7071067811865474617, 0.7071067811865474617, 0.7071067811865474617, 0.7071067811865476838, 0.7071067811865476838, 0.7071067811865475727, 0.7071067811865475727, 0.7071067811865475727, 0.7071067811865475727, 0.7071067811865474617, 0.7071067811865474617, 0.7071067811865474617, 0.7071067811865474617),
 ( 1.000000000000000000, 1.000000000000000000, 1.000000000000000000, 1.000000000000000000, 1.000000000000000000, 1.000000000000000000, 1.000000000000000000, 1.000000000000000000, 1.000000000000000000, 1.000000000000000000, 1.000000000000000000, 1.000000000000000000, 1.000000000000000000, 1.000000000000000000, 1.000000000000000000, 1.000000000000000000, 1.000000000000000000, 1.000000000000000000) ) ) 
 REPRESENTATION_ITEM ( '' )  SURFACE ( )  );
#37444 = EDGE_CURVE ( 'NONE', #19849, #34816, #35829, .T. ) ;
#37445 = FACE_BOUND ( 'NONE', #8176, .T. ) ;
#37446 = EDGE_CURVE ( 'NONE', #20131, #9944, #7986, .T. ) ;
#37447 = CARTESIAN_POINT ( 'NONE',  ( 25.01795332078024359, 8.530037020299428008, 14.53008259254034407 ) ) ;
#37448 = CARTESIAN_POINT ( 'NONE',  ( -23.24656352754010769, 7.851391979896635398, -11.84231981378251497 ) ) ;
#37449 = CARTESIAN_POINT ( 'NONE',  ( -19.48557158514988785, -11.24999999999987743, 10.00000000000000000 ) ) ;
#37450 = CARTESIAN_POINT ( 'NONE',  ( 16.99999999999999645, 22.50000000000000711, 6.000000000000000000 ) ) ;
#37451 = CARTESIAN_POINT ( 'NONE',  ( 23.11526344011869938, -26.83253816688370819, -5.000000000000002665 ) ) ;
#37452 = CARTESIAN_POINT ( 'NONE',  ( -14.47283171447380035, 21.48159823030330884, 7.000000000000000000 ) ) ;
#37453 = CARTESIAN_POINT ( 'NONE',  ( 11.52907589320744464, 19.06142540582696654, -22.70785398504575170 ) ) ;
#37454 = AXIS2_PLACEMENT_3D ( 'NONE', #1107, #35637, #35432 ) ;
#37455 = ORIENTED_EDGE ( 'NONE', *, *, #4660, .F. ) ;
#37457 = CIRCLE ( 'NONE', #16704, 0.5000000000000000000 ) ;
#37456 = CARTESIAN_POINT ( 'NONE',  ( -15.71345004126338907, 23.14940864091746064, -10.22852350719944958 ) ) ;
#37458 = EDGE_CURVE ( 'NONE', #4655, #17743, #39071, .T. ) ;
#37459 = CARTESIAN_POINT ( 'NONE',  ( -19.16156146161704399, -20.39791387780022092, 20.50957957746050653 ) ) ;
#37460 = DIRECTION ( 'NONE',  ( 0.000000000000000000, 0.000000000000000000, -1.000000000000000000 ) ) ;
#37461 = CARTESIAN_POINT ( 'NONE',  ( 12.16656640916057697, 19.88180003594682788, -20.54734239706648680 ) ) ;
#37462 = ORIENTED_EDGE ( 'NONE', *, *, #14214, .F. ) ;
#37463 = DIRECTION ( 'NONE',  ( 1.000000000000000000, 0.000000000000000000, -0.000000000000000000 ) ) ;
#37464 = EDGE_LOOP ( 'NONE', ( #29774, #4249, #32571 ) ) ;
#37466 = CARTESIAN_POINT ( 'NONE',  ( -6.082607396026893376, 23.58034083595207875, 12.00000000000000000 ) ) ;
#37465 = CARTESIAN_POINT ( 'NONE',  ( -14.93646167759306387, 26.23028568784196324, -9.225374686410800606 ) ) ;
#37467 = CARTESIAN_POINT ( 'NONE',  ( -13.50903009133150334, -23.63675682006747891, -14.46352174718241024 ) ) ;
#37468 = CARTESIAN_POINT ( 'NONE',  ( -5.440908595777639079, 35.94977745735568675, 9.500000000000000000 ) ) ;
#37469 = CIRCLE ( 'NONE', #7596, 1.000000000000000888 ) ;
#37470 = ORIENTED_EDGE ( 'NONE', *, *, #2137, .F. ) ;
#37471 = CARTESIAN_POINT ( 'NONE',  ( -24.11028944448099054, -11.71693609780529677, -18.62405750076642619 ) ) ;
#37472 = CARTESIAN_POINT ( 'NONE',  ( -9.288864052834329144, -19.07931708185379449, -25.08847946617766667 ) ) ;
#37473 = DIRECTION ( 'NONE',  ( -0.000000000000000000, -0.000000000000000000, 1.000000000000000000 ) ) ;
#37474 = CARTESIAN_POINT ( 'NONE',  ( 16.42302884132381635, 23.18804532280490704, -6.898824423637220704 ) ) ;
#37475 = ORIENTED_EDGE ( 'NONE', *, *, #13303, .F. ) ;
#37476 = CARTESIAN_POINT ( 'NONE',  ( 26.52510315481259440, 4.669929872087335454, -7.390039225938844325 ) ) ;
#37477 = CARTESIAN_POINT ( 'NONE',  ( -7.353987181296344211, 35.57359447655193208, 7.000000000000000000 ) ) ;
#37478 = CARTESIAN_POINT ( 'NONE',  ( -6.330077540933487512, 17.71145523154927659, 13.00000000000000178 ) ) ;
#37479 = CARTESIAN_POINT ( 'NONE',  ( 2.525645716490518833, 8.212903943950921715, 7.499999999999990230 ) ) ;
#37480 = ORIENTED_EDGE ( 'NONE', *, *, #4369, .F. ) ;
#37481 = EDGE_CURVE ( 'NONE', #36809, #22627, #14462, .T. ) ;
#37482 = CARTESIAN_POINT ( 'NONE',  ( -31.16128978838004215, -0.4216671695662963515, -6.408873994583965228 ) ) ;
#37483 = EDGE_CURVE ( 'NONE', #32345, #35666, #24036, .T. ) ;
#37484 = CARTESIAN_POINT ( 'NONE',  ( 30.50596941830245967, -0.3378608342927111874, -8.747934072216118295 ) ) ;
#37485 = CARTESIAN_POINT ( 'NONE',  ( 26.92296394334098153, -7.646625634048409559, 20.69868183039782394 ) ) ;
#37486 = VERTEX_POINT ( 'NONE', #26279 ) ;
#37487 = CARTESIAN_POINT ( 'NONE',  ( -19.54664213359414404, -11.28525909758381829, -30.00000000000000711 ) ) ;
#37488 = CARTESIAN_POINT ( 'NONE',  ( 1.000000000000000000, 37.00000000000000711, 10.50000000000000178 ) ) ;
#37489 = CONICAL_SURFACE ( 'NONE', #8959, 1.000000000000007772, 0.7853981633974557175 ) ;
#37490 = CONICAL_SURFACE ( 'NONE', #25159, 1.000000000000000444, 0.7853981633974482790 ) ;
#37491 = EDGE_LOOP ( 'NONE', ( #3278, #17766 ) ) ;
#37492 = CARTESIAN_POINT ( 'NONE',  ( -11.77929587896040786, 31.08767655398749596, 7.000000000000000000 ) ) ;
#37493 = AXIS2_PLACEMENT_3D ( 'NONE', #31149, #30753, #14913 ) ;
#37494 = CIRCLE ( 'NONE', #22548, 1.000000000000000888 ) ;
#37495 = CARTESIAN_POINT ( 'NONE',  ( -15.00309677617818771, 1.567672476163657125, 23.00000000000000000 ) ) ;
#37496 = CARTESIAN_POINT ( 'NONE',  ( 37.57549957648898697, 32.94422479542058824, 0.000000000000000000 ) ) ;
#37497 = CARTESIAN_POINT ( 'NONE',  ( 2.599036944496103452, 35.98214420759691734, -10.17776264407841857 ) ) ;
#37498 = EDGE_CURVE ( 'NONE', #8563, #12781, #29733, .T. ) ;
#37499 = CARTESIAN_POINT ( 'NONE',  ( -5.187504188494229673, 36.60991850771488743, 10.50000000000000533 ) ) ;
#37500 = FACE_OUTER_BOUND ( 'NONE', #38115, .T. ) ;
#37501 = DIRECTION ( 'NONE',  ( 0.9781476007338036904, -0.2079116908177680301, 0.000000000000000000 ) ) ;
#37502 = CARTESIAN_POINT ( 'NONE',  ( 0.5000000000000006661, 32.50000000000000000, 10.00000000000000000 ) ) ;
#37503 = CARTESIAN_POINT ( 'NONE',  ( -0.4999999999999998890, 37.50000000000000711, 10.49999999999999822 ) ) ;
#37504 = DIRECTION ( 'NONE',  ( -0.000000000000000000, -0.000000000000000000, -1.000000000000000000 ) ) ;
#37505 = CARTESIAN_POINT ( 'NONE',  ( 12.09704535053124097, 21.84084311221952746, -18.33700071698500977 ) ) ;
#37506 = DIRECTION ( 'NONE',  ( 0.000000000000000000, 0.000000000000000000, 1.000000000000000000 ) ) ;
#37507 = ORIENTED_EDGE ( 'NONE', *, *, #21575, .T. ) ;
#37509 = CARTESIAN_POINT ( 'NONE',  ( 13.97557076678965693, 21.53386246193694475, 7.500000000000010658 ) ) ;
#37508 = CARTESIAN_POINT ( 'NONE',  ( -18.27253818691323062, 18.69021931283398530, -5.478664268103901946 ) ) ;
#37510 = CARTESIAN_POINT ( 'NONE',  ( 14.36830325120613061, 20.48707633493482660, 11.00000000000000000 ) ) ;
#37511 = CARTESIAN_POINT ( 'NONE',  ( 9.602585878379885642, -18.34980316067541750, -27.44912381818026859 ) ) ;
#37512 = CARTESIAN_POINT ( 'NONE',  ( -22.64013887523591606, -26.77760336401204100, -6.771740173302402077 ) ) ;
#37513 = CARTESIAN_POINT ( 'NONE',  ( 12.39760697099640652, 20.48158002049096282, -19.49775760875778019 ) ) ;
#37514 = CARTESIAN_POINT ( 'NONE',  ( 15.01370201814430061, 25.98344539277131204, -9.237562102240422846 ) ) ;
#37515 = VERTEX_POINT ( 'NONE', #13891 ) ;
#37516 = DIRECTION ( 'NONE',  ( 0.000000000000000000, 0.000000000000000000, 1.000000000000000000 ) ) ;
#37517 = CARTESIAN_POINT ( 'NONE',  ( -9.458459612945102180, -18.23765197637141711, -28.70940629815209633 ) ) ;
#37518 = CARTESIAN_POINT ( 'NONE',  ( -36.80210562958730236, -14.73639196410522345, 13.32518128616608699 ) ) ;
#37519 = AXIS2_PLACEMENT_3D ( 'NONE', #25732, #961, #4203 ) ;
#37520 = AXIS2_PLACEMENT_3D ( 'NONE', #3296, #15688, #9400 ) ;
#37521 = CARTESIAN_POINT ( 'NONE',  ( -16.85969849069656590, -12.36963956004071186, -26.98632881526714655 ) ) ;
#37522 = CARTESIAN_POINT ( 'NONE',  ( -0.3846874604185267499, -24.60652018611802205, -7.918091565281228483 ) ) ;
#37523 = CARTESIAN_POINT ( 'NONE',  ( 14.68761894541005475, 23.48803088349838220, -12.58875248005314873 ) ) ;
#37524 = EDGE_LOOP ( 'NONE', ( #9257, #21227, #20771, #7442 ) ) ;
#37525 = CARTESIAN_POINT ( 'NONE',  ( 19.48270368550455700, 8.998075144385749624, -22.23371150557425935 ) ) ;
#37526 = CARTESIAN_POINT ( 'NONE',  ( 13.49038105676655164, 15.86602540378438064, 11.00000000000000000 ) ) ;
#37527 = CIRCLE ( 'NONE', #17447, 1.000000000000000000 ) ;
#37528 = ORIENTED_EDGE ( 'NONE', *, *, #29476, .T. ) ;
#37529 = CARTESIAN_POINT ( 'NONE',  ( -20.34904904974839468, -3.057566804462165777, -28.57235194868102113 ) ) ;
#37530 = VECTOR ( 'NONE', #30886, 1000.000000000000000 ) ;
#37531 = CARTESIAN_POINT ( 'NONE',  ( -29.73172958077111971, -1.192874570362842057, 17.92354375535250810 ) ) ;
#37532 = VERTEX_POINT ( 'NONE', #36431 ) ;
#37533 = LINE ( 'NONE', #12346, #29753 ) ;
#37534 = EDGE_CURVE ( 'NONE', #23608, #36809, #2154, .T. ) ;
#37535 = CARTESIAN_POINT ( 'NONE',  ( 24.22334197529778521, -9.561459978639769375, 22.99999999999999645 ) ) ;
#37536 = ADVANCED_FACE ( 'NONE', ( #14290 ), #2919, .T. ) ;
#37537 = CARTESIAN_POINT ( 'NONE',  ( -26.12154978825257956, 0.8729768346659233513, -15.49655606007314113 ) ) ;
#37538 = CARTESIAN_POINT ( 'NONE',  ( 25.90986923523073315, -9.535114592619988727, -17.67153410330361041 ) ) ;
#37539 = CARTESIAN_POINT ( 'NONE',  ( 35.38210723591825513, -3.548218742174890750, 13.32518128616608344 ) ) ;
#37540 = ORIENTED_EDGE ( 'NONE', *, *, #3139, .T. ) ;
#37541 = DIRECTION ( 'NONE',  ( 1.000000000000000000, 0.000000000000000000, 0.000000000000000000 ) ) ;
#37542 = ORIENTED_EDGE ( 'NONE', *, *, #18359, .F. ) ;
#37543 = EDGE_CURVE ( 'NONE', #28556, #9089, #12505, .T. ) ;
#37544 = CARTESIAN_POINT ( 'NONE',  ( 2.476901250629512941, 26.36149378532653031, 12.00000000000000000 ) ) ;
#37545 = CARTESIAN_POINT ( 'NONE',  ( -10.47804177580193041, 33.28010392086039104, 11.00000000000000000 ) ) ;
#37546 = CIRCLE ( 'NONE', #2524, 1.000000000000000000 ) ;
#37547 = AXIS2_PLACEMENT_3D ( 'NONE', #10396, #32745, #10800 ) ;
#37548 = CARTESIAN_POINT ( 'NONE',  ( 3.863783140547853712E-14, -86.77689918168233874, 23.00000000000000000 ) ) ;
#37549 = ORIENTED_EDGE ( 'NONE', *, *, #8377, .T. ) ;
#37550 = CARTESIAN_POINT ( 'NONE',  ( -2.819557190764113930, 25.49732518862137454, -19.66265949721264761 ) ) ;
#37551 = CARTESIAN_POINT ( 'NONE',  ( -4.524139159579194214, 31.43208625488816566, 10.50000000000000711 ) ) ;
#37552 = CARTESIAN_POINT ( 'NONE',  ( 13.39463915635820790, 18.33192650902018883, 13.00000000000000178 ) ) ;
#37553 = DIRECTION ( 'NONE',  ( 0.000000000000000000, 0.000000000000000000, 1.000000000000000000 ) ) ;
#37554 = LINE ( 'NONE', #12959, #33372 ) ;
#37555 = CARTESIAN_POINT ( 'NONE',  ( -2.525645716490712012, 8.212903943950955465, 7.000000000000000000 ) ) ;
#37556 = CARTESIAN_POINT ( 'NONE',  ( 8.851496467661105427, 18.99526148928798719, -26.62540179812685892 ) ) ;
#37557 = EDGE_LOOP ( 'NONE', ( #34529, #23755, #13385, #40098 ) ) ;
#37558 = CARTESIAN_POINT ( 'NONE',  ( -17.63234478075006706, 10.48641262593123535, -29.99999999999998934 ) ) ;
#37559 = CARTESIAN_POINT ( 'NONE',  ( 15.33540832684151134, 35.51988609203956315, 11.00000000000000000 ) ) ;
#37560 = EDGE_CURVE ( 'NONE', #6246, #13267, #31311, .T. ) ;
#37561 = CARTESIAN_POINT ( 'NONE',  ( 9.659365752239464697, -18.32200075079210322, -27.44504324438285892 ) ) ;
#37562 = DIRECTION ( 'NONE',  ( -0.5720614028176850274, 0.4156269377774632345, -0.7071067811865411334 ) ) ;
#37563 = CARTESIAN_POINT ( 'NONE',  ( 15.37658843025399413, 26.83106350242916704, -5.945231630724503447 ) ) ;
#37564 = CARTESIAN_POINT ( 'NONE',  ( 22.45323650136968396, -2.382502413133517738, -29.99999999999998934 ) ) ;
#37565 = LINE ( 'NONE', #21718, #16791 ) ;
#37566 = CARTESIAN_POINT ( 'NONE',  ( -27.04961384508420608, -25.34883885810744886, -5.441318665117593767 ) ) ;
#37567 = CARTESIAN_POINT ( 'NONE',  ( 9.100901191155434944, -19.97180529156877782, -22.89666456064600908 ) ) ;
#37568 = CARTESIAN_POINT ( 'NONE',  ( 15.43128619640941857, 26.46390025712458183, -6.417237675877188963 ) ) ;
#37569 = CARTESIAN_POINT ( 'NONE',  ( 22.18477674033645286, -15.00887286453208169, -18.62664606145825275 ) ) ;
#37570 = CARTESIAN_POINT ( 'NONE',  ( 7.713869163865845202, 10.18146832927074641, 10.49999999999999822 ) ) ;
#37571 = DIRECTION ( 'NONE',  ( -0.1045284632676422437, 0.9945218953682746221, 0.000000000000000000 ) ) ;
#37572 = EDGE_LOOP ( 'NONE', ( #20760, #33143 ) ) ;
#37573 = CARTESIAN_POINT ( 'NONE',  ( -5.489946483366239249, 20.60753015119807330, -25.73531879562920111 ) ) ;
#37574 = CARTESIAN_POINT ( 'NONE',  ( -12.47973198054747890, 14.17771442864374443, 7.339470489435493405 ) ) ;
#37575 = CARTESIAN_POINT ( 'NONE',  ( 5.167086843766643511, 44.40436517110171621, 11.00000000000000000 ) ) ;
#37576 = AXIS2_PLACEMENT_3D ( 'NONE', #10271, #39052, #732 ) ;
#37577 = AXIS2_PLACEMENT_3D ( 'NONE', #5224, #23910, #24505 ) ;
#37578 = DIRECTION ( 'NONE',  ( 0.000000000000000000, 0.000000000000000000, 1.000000000000000000 ) ) ;
#37579 = ORIENTED_EDGE ( 'NONE', *, *, #21941, .F. ) ;
#37580 = CARTESIAN_POINT ( 'NONE',  ( 30.89317523684279010, -0.03095884371312799394, -5.000000000000000000 ) ) ;
#37581 = DIRECTION ( 'NONE',  ( -0.8090169943749497827, -0.5877852522924698064, 0.000000000000000000 ) ) ;
#37582 = EDGE_CURVE ( 'NONE', #34828, #26924, #32382, .T. ) ;
#37583 = CARTESIAN_POINT ( 'NONE',  ( -37.48557158514985588, -11.24999999999982414, 6.000000000000000000 ) ) ;
#37584 = VECTOR ( 'NONE', #8321, 1000.000000000000000 ) ;
#37585 = PRODUCT_DEFINITION_SHAPE ( 'NONE', 'NONE',  #40204 ) ;
#37586 = ORIENTED_EDGE ( 'NONE', *, *, #12511, .F. ) ;
#37587 = CARTESIAN_POINT ( 'NONE',  ( -30.81224694139058329, 0.01613667459859374764, -5.946089668811439743 ) ) ;
#37588 = EDGE_CURVE ( 'NONE', #15880, #25686, #9913, .T. ) ;
#37589 = CARTESIAN_POINT ( 'NONE',  ( -20.35363302287704101, -26.94962880062152877, -7.247870005599446053 ) ) ;
#37590 = EDGE_LOOP ( 'NONE', ( #39461, #1442 ) ) ;
#37591 = CARTESIAN_POINT ( 'NONE',  ( 27.93478377975757354, -4.930528639082491615, -15.96261009728761060 ) ) ;
#37592 = EDGE_CURVE ( 'NONE', #31950, #5290, #17706, .T. ) ;
#37593 = VERTEX_POINT ( 'NONE', #30932 ) ;
#37594 = CARTESIAN_POINT ( 'NONE',  ( -1.450054154221040505E-13, 40.30103163374182174, 12.73282698324853257 ) ) ;
#37595 = EDGE_CURVE ( 'NONE', #13490, #28177, #10556, .T. ) ;
#37596 = CARTESIAN_POINT ( 'NONE',  ( 9.997483185316555776, 21.95197631500757041, 10.50000000000000355 ) ) ;
#37597 = DIRECTION ( 'NONE',  ( 0.000000000000000000, 0.000000000000000000, 1.000000000000000000 ) ) ;
#37598 = CARTESIAN_POINT ( 'NONE',  ( 2.823200210931128940, 35.29864485453420286, 18.87996532025784902 ) ) ;
#37599 = CARTESIAN_POINT ( 'NONE',  ( 5.184280209938512129, 31.68549066217151022, 10.50000000000000000 ) ) ;
#37600 = VERTEX_POINT ( 'NONE', #37226 ) ;
#37601 = CARTESIAN_POINT ( 'NONE',  ( 3.601976756503082910, 7.958898870085707067, 10.68306085400107186 ) ) ;
#37602 = CARTESIAN_POINT ( 'NONE',  ( -4.769256462637533112, 19.93975062605538184, -29.99999999999996803 ) ) ;
#37603 = DIRECTION ( 'NONE',  ( 0.000000000000000000, 0.000000000000000000, 1.000000000000000000 ) ) ;
#37604 = FACE_OUTER_BOUND ( 'NONE', #7291, .T. ) ;
#37605 = CARTESIAN_POINT ( 'NONE',  ( 14.52284994691540554, 15.12055744848739458, -25.35930744202923393 ) ) ;
#37607 = CIRCLE ( 'NONE', #6448, 0.5000000000000013323 ) ;
#37606 = CARTESIAN_POINT ( 'NONE',  ( 8.493348210982047064, 32.87541910339748341, -11.15327735273583620 ) ) ;
#37608 = ADVANCED_FACE ( 'NONE', ( #34180 ), #35194, .T. ) ;
#37609 = EDGE_CURVE ( 'NONE', #9898, #22876, #30016, .T. ) ;
#37610 = CARTESIAN_POINT ( 'NONE',  ( 17.77051926636400836, -26.05666342080411013, -10.02570539512946901 ) ) ;
#37611 = CARTESIAN_POINT ( 'NONE',  ( -3.833852081710639848, 25.75497152300896886, 20.99999999999999645 ) ) ;
#37612 = VECTOR ( 'NONE', #22489, 1000.000000000000000 ) ;
#37613 = CARTESIAN_POINT ( 'NONE',  ( -10.10646936306323518, 32.94553861768095970, 11.00000000000000000 ) ) ;
#37614 = ORIENTED_EDGE ( 'NONE', *, *, #4895, .F. ) ;
#37615 = CARTESIAN_POINT ( 'NONE',  ( -11.07958958704495167, 17.49807219138947545, -27.44831219198803396 ) ) ;
#37616 = CARTESIAN_POINT ( 'NONE',  ( -32.46232039045670348, -18.74212941594990767, 17.42190598798392642 ) ) ;
#37617 = CARTESIAN_POINT ( 'NONE',  ( 15.18788860438108124, -26.66571922823320051, -5.474128979186436261 ) ) ;
#37618 = DIRECTION ( 'NONE',  ( 0.000000000000000000, 0.000000000000000000, 1.000000000000000000 ) ) ;
#37619 = ORIENTED_EDGE ( 'NONE', *, *, #25976, .T. ) ;
#37620 = EDGE_LOOP ( 'NONE', ( #8637, #37627 ) ) ;
#37621 = CARTESIAN_POINT ( 'NONE',  ( -10.01402912130534162, 17.90039694996872655, -29.32746991544585313 ) ) ;
#37622 = CARTESIAN_POINT ( 'NONE',  ( -6.535904741238326210, 35.95058573176953587, 10.76099332938163400 ) ) ;
#37623 = FACE_BOUND ( 'NONE', #34217, .T. ) ;
#37624 = CARTESIAN_POINT ( 'NONE',  ( -19.56896045557411767, -6.106514739740910969, -29.23677687923446911 ) ) ;
#37625 = CARTESIAN_POINT ( 'NONE',  ( -15.36059797614417199, -26.70982037388659691, -5.000000000000000888 ) ) ;
#37626 = DIRECTION ( 'NONE',  ( -0.9335804264971983013, -0.3583679495453093722, 6.429803227988806504E-16 ) ) ;
#37627 = ORIENTED_EDGE ( 'NONE', *, *, #618, .F. ) ;
#37628 = CARTESIAN_POINT ( 'NONE',  ( 30.61281600001173686, 0.2212781233926191804, -5.946150247221624774 ) ) ;
#37629 = CARTESIAN_POINT ( 'NONE',  ( -1.358232629781535916, 33.31072022568110924, 13.00000000000000178 ) ) ;
#37630 = CARTESIAN_POINT ( 'NONE',  ( 3.597409820281487480, 14.42008525284347087, 9.000000000000001776 ) ) ;
#37631 = VERTEX_POINT ( 'NONE', #24234 ) ;
#37632 = CARTESIAN_POINT ( 'NONE',  ( -30.02005750921860638, -0.001135212662567658751, -9.236802755891959649 ) ) ;
#37633 = EDGE_CURVE ( 'NONE', #5601, #6401, #37421, .T. ) ;
#37634 = ORIENTED_EDGE ( 'NONE', *, *, #86, .F. ) ;
#37635 = CARTESIAN_POINT ( 'NONE',  ( 23.05089902286179893, -0.5612348335507770791, -21.46137821024467840 ) ) ;
#37636 = AXIS2_PLACEMENT_3D ( 'NONE', #24261, #14921, #11872 ) ;
#37637 = CARTESIAN_POINT ( 'NONE',  ( 23.54493052986452284, -14.21898406159493966, 20.99999999999999645 ) ) ;
#37638 = CARTESIAN_POINT ( 'NONE',  ( 33.46894051142319881, -4.475137156697218899, 16.87380292611441845 ) ) ;
#37639 = ORIENTED_EDGE ( 'NONE', *, *, #20865, .F. ) ;
#37640 = AXIS2_PLACEMENT_3D ( 'NONE', #34642, #35244, #10057 ) ;
#37641 = CARTESIAN_POINT ( 'NONE',  ( -14.98890122036483419, -28.67928442680469203, -4.999999999999999112 ) ) ;
#37642 = CARTESIAN_POINT ( 'NONE',  ( -0.6269669233417689558, 28.28960257232501974, 20.99999999999998934 ) ) ;
#37643 = CARTESIAN_POINT ( 'NONE',  ( -15.48853126089653642, -26.74269726827072446, -4.999999999999999112 ) ) ;
#37644 = DIRECTION ( 'NONE',  ( 1.000000000000000000, 0.000000000000000000, 0.000000000000000000 ) ) ;
#37645 = AXIS2_PLACEMENT_3D ( 'NONE', #2228, #14613, #24149 ) ;
#37646 = FACE_BOUND ( 'NONE', #16491, .T. ) ;
#37647 = CARTESIAN_POINT ( 'NONE',  ( 20.66414367075948277, 17.76245163070629829, 10.99999999999897859 ) ) ;
#37648 = CARTESIAN_POINT ( 'NONE',  ( -20.30282733015013363, 7.292259425124786532, -22.18016511663011059 ) ) ;
#37649 = CARTESIAN_POINT ( 'NONE',  ( 21.74762051904238191, -24.00969798870548644, -12.12483235932745984 ) ) ;
#37650 = CARTESIAN_POINT ( 'NONE',  ( -0.4999999999999950040, -6.123233995736694545E-17, 11.00000000000000000 ) ) ;
#37651 = EDGE_CURVE ( 'NONE', #26489, #39789, #36633, .T. ) ;
#37652 = CARTESIAN_POINT ( 'NONE',  ( 12.28203363025439288, 20.63554315272105555, -19.47339641021015311 ) ) ;
#37653 = VERTEX_POINT ( 'NONE', #15890 ) ;
#37654 = CARTESIAN_POINT ( 'NONE',  ( -13.08623023714802258, 18.08879695936160203, -21.80946885493514031 ) ) ;
#37655 = CARTESIAN_POINT ( 'NONE',  ( -28.63766977552542770, -11.08150102882335375, 20.50957957746073390 ) ) ;
#37656 = CARTESIAN_POINT ( 'NONE',  ( 10.14084140100273146, 32.97648733965218071, 10.49999999999999822 ) ) ;
#37657 = CARTESIAN_POINT ( 'NONE',  ( 11.03147510093559269, 17.33177591260932715, -28.70801338942442982 ) ) ;
#37658 = ORIENTED_EDGE ( 'NONE', *, *, #4814, .F. ) ;
#37659 = CARTESIAN_POINT ( 'NONE',  ( -32.33143948541797386, 1.358872982501901472, 2.999999999999999112 ) ) ;
#37660 = CIRCLE ( 'NONE', #6535, 1.000000000000005329 ) ;
#37661 = ORIENTED_EDGE ( 'NONE', *, *, #25378, .T. ) ;
#37663 = CARTESIAN_POINT ( 'NONE',  ( 12.80736835487433289, 15.68301270189216545, 7.000000000000000000 ) ) ;
#37662 = CARTESIAN_POINT ( 'NONE',  ( -15.26899636581957687, 27.02509300740851472, -6.411569543597564369 ) ) ;
#37664 = CARTESIAN_POINT ( 'NONE',  ( -13.14311512211350852, -23.10060485217718096, -15.43729266571827097 ) ) ;
#37665 = FACE_OUTER_BOUND ( 'NONE', #19617, .T. ) ;
#37666 = ORIENTED_EDGE ( 'NONE', *, *, #1427, .F. ) ;
#37667 = CARTESIAN_POINT ( 'NONE',  ( -33.45518794257092310, -14.98363075432738789, -9.291991822186489003 ) ) ;
#37668 = CARTESIAN_POINT ( 'NONE',  ( -12.02413919917706764, -23.04697477249095883, -15.51450891573247048 ) ) ;
#37669 = DIRECTION ( 'NONE',  ( 0.000000000000000000, 0.000000000000000000, 1.000000000000000000 ) ) ;
#37670 = CARTESIAN_POINT ( 'NONE',  ( 12.38972167065434782, 16.33584955698245977, -30.00000000000000711 ) ) ;
#37671 = EDGE_LOOP ( 'NONE', ( #17326, #20612, #38478, #23052 ) ) ;
#37672 = CARTESIAN_POINT ( 'NONE',  ( 25.47574744270427516, 5.541576092252077146, -9.334551064280120158 ) ) ;
#37673 = CARTESIAN_POINT ( 'NONE',  ( -3.992867117591420545, 8.524771480177605554, 7.499999999999997335 ) ) ;
#37674 = CARTESIAN_POINT ( 'NONE',  ( 15.48853125999100833, -26.74269726803731118, -5.000000000000000000 ) ) ;
#37675 = FACE_OUTER_BOUND ( 'NONE', #27713, .T. ) ;
#37676 = EDGE_LOOP ( 'NONE', ( #11552, #34173, #12805, #36866 ) ) ;
#37677 = CARTESIAN_POINT ( 'NONE',  ( -26.07300228947948284, -0.03011411378347995590, -16.39941592429670081 ) ) ;
#37678 = ADVANCED_FACE ( 'NONE', ( #25618 ), #1050, .F. ) ;
#37679 = CARTESIAN_POINT ( 'NONE',  ( 20.82749634169985953, 0.6853679382005627430, -26.81932549163500568 ) ) ;
#37680 = AXIS2_PLACEMENT_3D ( 'NONE', #11670, #12260, #2329 ) ;
#37681 = EDGE_CURVE ( 'NONE', #16160, #40105, #21597, .T. ) ;
#37682 = CARTESIAN_POINT ( 'NONE',  ( 28.41077021456689522, -6.925791943819275431, 20.25080042701566541 ) ) ;
#37683 = AXIS2_PLACEMENT_3D ( 'NONE', #16971, #10670, #38700 ) ;
#37684 = ORIENTED_EDGE ( 'NONE', *, *, #20314, .F. ) ;
#37685 = CARTESIAN_POINT ( 'NONE',  ( -26.31271763591404422, -28.25584584496042240, -5.000000000000000888 ) ) ;
#37686 = FACE_OUTER_BOUND ( 'NONE', #289, .T. ) ;
#37687 = EDGE_CURVE ( 'NONE', #5736, #17675, #1476, .T. ) ;
#37688 = ORIENTED_EDGE ( 'NONE', *, *, #2798, .F. ) ;
#37689 = AXIS2_PLACEMENT_3D ( 'NONE', #31061, #30664, #39990 ) ;
#37690 = DIRECTION ( 'NONE',  ( 1.000000000000000000, 0.000000000000000000, 0.000000000000000000 ) ) ;
#37691 = CARTESIAN_POINT ( 'NONE',  ( -11.46110488303199126, 32.14680882400074324, 10.68306159501106656 ) ) ;
#37692 = CARTESIAN_POINT ( 'NONE',  ( 12.53024597560964537, 27.62278594035691626, 9.500000000000000000 ) ) ;
#37693 = CARTESIAN_POINT ( 'NONE',  ( 4.646098203774434943, 34.72221286985408284, -11.08844531243078890 ) ) ;
#37694 = CARTESIAN_POINT ( 'NONE',  ( -7.766013557953296953, 28.81973365084997951, 10.00000000000000000 ) ) ;
#37695 = CARTESIAN_POINT ( 'NONE',  ( 14.60528968261095173, 20.46216805729368460, 10.94387467463493380 ) ) ;
#37696 = CARTESIAN_POINT ( 'NONE',  ( 14.26584437371809777, 27.13525491562438319, 6.000000000000000000 ) ) ;
#37697 = EDGE_CURVE ( 'NONE', #29830, #11555, #39115, .T. ) ;
#37698 = CYLINDRICAL_SURFACE ( 'NONE', #39138, 0.5000000000000004441 ) ;
#37699 = DIRECTION ( 'NONE',  ( 0.7431448254773953543, 0.6691306063588570163, 0.000000000000000000 ) ) ;
#37700 = DIRECTION ( 'NONE',  ( -0.000000000000000000, -0.000000000000000000, -1.000000000000000000 ) ) ;
#37701 = EDGE_CURVE ( 'NONE', #22687, #7627, #25419, .T. ) ;
#37702 = CARTESIAN_POINT ( 'NONE',  ( 14.60593664522046353, 26.75915035538402265, -9.657648197979836979 ) ) ;
#37703 = DIRECTION ( 'NONE',  ( -0.000000000000000000, -0.000000000000000000, -1.000000000000000000 ) ) ;
#37704 = ORIENTED_EDGE ( 'NONE', *, *, #16957, .T. ) ;
#37705 = VECTOR ( 'NONE', #30512, 1000.000000000000114 ) ;
#37707 = CARTESIAN_POINT ( 'NONE',  ( -4.118678732975735279, 7.827785988993307242, 12.00000000000000000 ) ) ;
#37706 = CARTESIAN_POINT ( 'NONE',  ( -18.18070401533917035, 18.56346265111594462, -7.404067847983029083 ) ) ;
#37708 = CARTESIAN_POINT ( 'NONE',  ( 34.83525826321754693, -1.648928274806292116, 10.99999999999991829 ) ) ;
#37709 = VECTOR ( 'NONE', #3860, 1000.000000000000000 ) ;
#37710 = CARTESIAN_POINT ( 'NONE',  ( 11.89284648857719695, -21.48584275349674400, -18.45356361586392779 ) ) ;
#37711 = DIRECTION ( 'NONE',  ( 1.000000000000000000, 0.000000000000000000, 0.000000000000000000 ) ) ;
#37712 = CARTESIAN_POINT ( 'NONE',  ( 14.94089887612034673, 25.78092154341846864, -9.709267021671619702 ) ) ;
#37713 = ORIENTED_EDGE ( 'NONE', *, *, #33660, .T. ) ;
#37714 = CARTESIAN_POINT ( 'NONE',  ( 11.28971518877922264, 18.05388930042798634, -25.01178682049573609 ) ) ;
#37715 = VERTEX_POINT ( 'NONE', #19133 ) ;
#37716 = DIRECTION ( 'NONE',  ( 0.000000000000000000, 0.000000000000000000, 1.000000000000000000 ) ) ;
#37717 = CARTESIAN_POINT ( 'NONE',  ( -14.67000517685553440, -25.63834831813752047, -10.18194144610326468 ) ) ;
#37718 = CARTESIAN_POINT ( 'NONE',  ( -32.69891748962417921, -23.33280782878161830, 12.73282698324838691 ) ) ;
#37719 = CARTESIAN_POINT ( 'NONE',  ( -30.45757913935707961, -22.41806408542251816, -7.125453223155250093 ) ) ;
#37720 = CARTESIAN_POINT ( 'NONE',  ( -2.095722264221089315, -22.15702150879218024, -19.05869434001748886 ) ) ;
#37721 = CARTESIAN_POINT ( 'NONE',  ( 13.54937698026857262, 21.63598032874356036, -16.49571944579557936 ) ) ;
#37722 = VERTEX_POINT ( 'NONE', #3689 ) ;
#37723 = CARTESIAN_POINT ( 'NONE',  ( 18.58241799660420668, 8.688807075854512618, -29.99999999999999645 ) ) ;
#37724 = DIRECTION ( 'NONE',  ( -1.000000000000000000, 0.000000000000000000, 0.000000000000000000 ) ) ;
#37725 = CARTESIAN_POINT ( 'NONE',  ( -12.75386240996836484, 29.27369326522011050, 17.92354375535251876 ) ) ;
#37726 = ORIENTED_EDGE ( 'NONE', *, *, #9525, .F. ) ;
#37727 = CARTESIAN_POINT ( 'NONE',  ( -20.65377969610915443, -2.455125782780259502, -27.23826263681096549 ) ) ;
#37728 = EDGE_CURVE ( 'NONE', #9701, #12080, #28671, .T. ) ;
#37729 = CARTESIAN_POINT ( 'NONE',  ( -30.57450045107345460, -0.3656520783135125963, 16.87380292611441845 ) ) ;
#37730 = VERTEX_POINT ( 'NONE', #13028 ) ;
#37731 = ADVANCED_FACE ( 'NONE', ( #9794 ), #31724, .T. ) ;
#37732 = CARTESIAN_POINT ( 'NONE',  ( 19.26948696230199687, 27.85601271560034675, 11.00000000000000000 ) ) ;
#37733 = DIRECTION ( 'NONE',  ( -0.000000000000000000, -0.000000000000000000, -1.000000000000000000 ) ) ;
#37734 = CARTESIAN_POINT ( 'NONE',  ( -20.67119347756820602, 2.193161261697490705, -26.92867794748204702 ) ) ;
#37735 = CARTESIAN_POINT ( 'NONE',  ( 21.94494290708799866, -8.860422532852833655, -21.89653876190107340 ) ) ;
#37736 = CARTESIAN_POINT ( 'NONE',  ( 34.59909889755208923, -19.97579906221994506, 13.92931973827808712 ) ) ;
#37737 = CIRCLE ( 'NONE', #8534, 6.000000000000012434 ) ;
#37738 = CIRCLE ( 'NONE', #20229, 0.5000000000000004441 ) ;
#37739 = ORIENTED_EDGE ( 'NONE', *, *, #34847, .T. ) ;
#37740 = VERTEX_POINT ( 'NONE', #16087 ) ;
#37741 = CARTESIAN_POINT ( 'NONE',  ( -13.05736835487441994, 16.11602540378456183, 7.499999999999993783 ) ) ;
#37742 = CARTESIAN_POINT ( 'NONE',  ( -0.6666666666666682950, 37.00000000000000711, 10.83333333333333215 ) ) ;
#37743 = FACE_OUTER_BOUND ( 'NONE', #29876, .T. ) ;
#37744 = ORIENTED_EDGE ( 'NONE', *, *, #35816, .F. ) ;
#37745 = CARTESIAN_POINT ( 'NONE',  ( -1.902173617953080376, 37.83571591983437088, -7.545775875163593049 ) ) ;
#37746 = CARTESIAN_POINT ( 'NONE',  ( 8.271785691010562047, 10.26421291652873968, 10.94611345180490680 ) ) ;
#37747 = CARTESIAN_POINT ( 'NONE',  ( -6.811226782241546651, 35.33967249274200384, 7.500000000000000888 ) ) ;
#37748 = AXIS2_PLACEMENT_3D ( 'NONE', #39019, #23782, #11197 ) ;
#37749 = DIRECTION ( 'NONE',  ( 0.7431448254773862505, -0.6691306063588670083, -0.000000000000000000 ) ) ;
#37750 = DIRECTION ( 'NONE',  ( -0.5254827454987616164, -0.4731467892558160471, -0.7071067811865446862 ) ) ;
#37751 = DIRECTION ( 'NONE',  ( 0.000000000000000000, 0.000000000000000000, 1.000000000000000000 ) ) ;
#37752 = CARTESIAN_POINT ( 'NONE',  ( 13.61253233593243550, 30.46620566788191198, -7.261355557076043965 ) ) ;
#37753 = CARTESIAN_POINT ( 'NONE',  ( 3.503793317224327186, 8.420815634768674229, 11.00000000000000000 ) ) ;
#37754 = VERTEX_POINT ( 'NONE', #38223 ) ;
#37755 = CARTESIAN_POINT ( 'NONE',  ( -18.11210683354745044, 9.887672296931658167, -27.17641187830589189 ) ) ;
#37756 = CARTESIAN_POINT ( 'NONE',  ( -12.39464589777671044, 26.66807349098043289, 12.00000000000000000 ) ) ;
#37757 = CARTESIAN_POINT ( 'NONE',  ( 13.07450261122289881, -23.09593886341139779, -15.44440162208020872 ) ) ;
#37758 = DIRECTION ( 'NONE',  ( -0.000000000000000000, -0.000000000000000000, -1.000000000000000000 ) ) ;
#37759 = ADVANCED_FACE ( 'NONE', ( #647 ), #34980, .F. ) ;
#37760 = CARTESIAN_POINT ( 'NONE',  ( 12.89273306925234586, 21.71245797589364912, -17.42948357415733796 ) ) ;
#37761 = CARTESIAN_POINT ( 'NONE',  ( 20.90924525106828114, -8.502318254486461058, -19.80438750953544513 ) ) ;
#37762 = DIRECTION ( 'NONE',  ( 0.000000000000000000, 0.000000000000000000, 1.000000000000000000 ) ) ;
#37763 = CARTESIAN_POINT ( 'NONE',  ( -23.45180357993919884, -24.82439038927461183, -10.28237032673689733 ) ) ;
#37764 = CARTESIAN_POINT ( 'NONE',  ( 5.727881898942783323, -19.93915831793329119, -27.08029247955964891 ) ) ;
#37765 = CARTESIAN_POINT ( 'NONE',  ( 11.99126504055620224, 19.27700041912028084, -21.63417993446100240 ) ) ;
#37766 = CARTESIAN_POINT ( 'NONE',  ( 18.50037648924358891, -13.33006404268201273, -23.01361493332205299 ) ) ;
#37767 = CARTESIAN_POINT ( 'NONE',  ( 14.02836544648986994, 27.77630492435572407, 10.49999999999999822 ) ) ;
#37768 = CARTESIAN_POINT ( 'NONE',  ( 75.15099915297797395, 43.38844959084117647, 2.999999999999999112 ) ) ;
#37769 = EDGE_LOOP ( 'NONE', ( #32054, #25147, #38817, #4547 ) ) ;
#37770 = CARTESIAN_POINT ( 'NONE',  ( -8.976254749716225945, 33.67889951363163448, -9.809507123318200073 ) ) ;
#37771 = CARTESIAN_POINT ( 'NONE',  ( 14.94248101481482038, 21.43223609974773325, 10.68306085400105232 ) ) ;
#37772 = ORIENTED_EDGE ( 'NONE', *, *, #35133, .F. ) ;
#37773 = CARTESIAN_POINT ( 'NONE',  ( 30.90370714462332202, -0.07739494692734212589, -5.945536237155164550 ) ) ;
#37774 = FACE_OUTER_BOUND ( 'NONE', #1696, .T. ) ;
#37775 = CIRCLE ( 'NONE', #20268, 15.00000000000000000 ) ;
#37776 = CARTESIAN_POINT ( 'NONE',  ( 22.42900687741999732, 24.35462947583786075, 11.00000000000000000 ) ) ;
#37777 = ORIENTED_EDGE ( 'NONE', *, *, #210, .F. ) ;
#37778 = CARTESIAN_POINT ( 'NONE',  ( -22.72062348006680921, 0.6442621738748725013, -21.62159724769585267 ) ) ;
#37779 = CARTESIAN_POINT ( 'NONE',  ( -8.796116341590805021, 23.42450908139092647, 9.000000000000001776 ) ) ;
#37780 = VERTEX_POINT ( 'NONE', #38017 ) ;
#37781 = CARTESIAN_POINT ( 'NONE',  ( 19.94806447466153543, -4.723319992639698484, -29.99999999999998579 ) ) ;
#37782 = AXIS2_PLACEMENT_3D ( 'NONE', #31373, #11895, #21235 ) ;
#37783 = ORIENTED_EDGE ( 'NONE', *, *, #15504, .T. ) ;
#37784 = CARTESIAN_POINT ( 'NONE',  ( -10.89111091687340682, 36.83121428896946981, 11.55979286843934339 ) ) ;
#37785 = CARTESIAN_POINT ( 'NONE',  ( 19.48557158514982746, -11.25000000000009415, 3.000000000000000000 ) ) ;
#37786 = CARTESIAN_POINT ( 'NONE',  ( -20.71630303010418572, -29.20803740758281464, -4.999999999999997335 ) ) ;
#37787 = CARTESIAN_POINT ( 'NONE',  ( -11.83264664767379948, 25.78892025138465272, 19.27171037444156454 ) ) ;
#37788 = DIRECTION ( 'NONE',  ( 0.000000000000000000, 0.000000000000000000, 1.000000000000000000 ) ) ;
#37789 = ORIENTED_EDGE ( 'NONE', *, *, #3200, .T. ) ;
#37790 = CARTESIAN_POINT ( 'NONE',  ( -5.408911131318492771, 19.77578011155457816, -29.99999999999996803 ) ) ;
#37791 = CARTESIAN_POINT ( 'NONE',  ( 12.30253635578773341, 13.91734747557917728, 7.102474990965858659 ) ) ;
#37792 = LINE ( 'NONE', #31303, #10430 ) ;
#37793 = CARTESIAN_POINT ( 'NONE',  ( 14.28645338827841726, 14.73924105482272751, -28.81583157955228458 ) ) ;
#37794 = AXIS2_PLACEMENT_3D ( 'NONE', #30162, #11277, #23661 ) ;
#37795 = CARTESIAN_POINT ( 'NONE',  ( 6.508078574177585729, 28.74780359284325826, -15.78726989322525398 ) ) ;
#37796 = ORIENTED_EDGE ( 'NONE', *, *, #22897, .T. ) ;
#37797 = EDGE_CURVE ( 'NONE', #11320, #25929, #1253, .T. ) ;
#37798 = TOROIDAL_SURFACE ( 'NONE', #13790, 1.000000000000000000, 0.5000000000000000000 ) ;
#37799 = CARTESIAN_POINT ( 'NONE',  ( 16.20692150584794078, -26.83310280674016468, -6.404917216296185600 ) ) ;
#37800 = DIRECTION ( 'NONE',  ( 0.2079116908177533474, -0.9781476007338067991, 0.000000000000000000 ) ) ;
#37801 = CARTESIAN_POINT ( 'NONE',  ( 1.160606217761757097, 37.45558278363897386, 7.202682876670053247 ) ) ;
#37802 = ORIENTED_EDGE ( 'NONE', *, *, #26513, .F. ) ;
#37803 = CARTESIAN_POINT ( 'NONE',  ( -15.41471391286399317, 26.78795929021520550, -5.474190302194672952 ) ) ;
#37804 = AXIS2_PLACEMENT_3D ( 'NONE', #28875, #31919, #13226 ) ;
#37805 = CARTESIAN_POINT ( 'NONE',  ( -31.72870305971091298, -3.591698066951732216, 17.92354375535209954 ) ) ;
#37806 = CARTESIAN_POINT ( 'NONE',  ( 14.40512807539449547, -25.86522860305755600, -9.245460395081696703 ) ) ;
#37807 = EDGE_CURVE ( 'NONE', #26812, #22931, #22571, .T. ) ;
#37808 = DIRECTION ( 'NONE',  ( 1.000000000000000000, 0.000000000000000000, 0.000000000000000000 ) ) ;
#37809 = ADVANCED_FACE ( 'NONE', ( #19528 ), #9988, .F. ) ;
#37810 = EDGE_LOOP ( 'NONE', ( #9037, #9787 ) ) ;
#37811 = ORIENTED_EDGE ( 'NONE', *, *, #30745, .F. ) ;
#37812 = CARTESIAN_POINT ( 'NONE',  ( -13.19605298241623714, 31.11796965224743516, -7.247223247613001185 ) ) ;
#37813 = LINE ( 'NONE', #38416, #16549 ) ;
#37814 = FACE_BOUND ( 'NONE', #20999, .T. ) ;
#37815 = CARTESIAN_POINT ( 'NONE',  ( -30.13885734736032518, -8.367891793043197524, -13.92058473770290661 ) ) ;
#37816 = DIRECTION ( 'NONE',  ( 0.6691306063588569053, -0.7431448254773954654, 0.000000000000000000 ) ) ;
#37817 = ORIENTED_EDGE ( 'NONE', *, *, #16535, .F. ) ;
#37818 = CARTESIAN_POINT ( 'NONE',  ( 20.80626354190386351, 0.9384790171570499551, -26.83885795680234310 ) ) ;
#37819 = LINE ( 'NONE', #7332, #1859 ) ;
#37820 = CARTESIAN_POINT ( 'NONE',  ( 14.52509594610761923, 21.97885917798724975, 10.50000000000000355 ) ) ;
#37821 = ORIENTED_EDGE ( 'NONE', *, *, #6746, .T. ) ;
#37822 = CARTESIAN_POINT ( 'NONE',  ( -27.16660938874878539, 0.1989104985245108981, -14.47297071791797052 ) ) ;
#37823 = ORIENTED_EDGE ( 'NONE', *, *, #35953, .F. ) ;
#37824 = CARTESIAN_POINT ( 'NONE',  ( 28.64846384017765502, -1.091167704362612678, -13.38480877307776851 ) ) ;
#37825 = CARTESIAN_POINT ( 'NONE',  ( 0.04788021487524250774, -20.50383365384739776, -30.00000000000000711 ) ) ;
#37826 = CARTESIAN_POINT ( 'NONE',  ( 28.49608467062326156, -24.01994641533507036, 16.87380292611404897 ) ) ;
#37827 = EDGE_CURVE ( 'NONE', #16446, #22627, #7099, .T. ) ;
#37828 = ORIENTED_EDGE ( 'NONE', *, *, #38418, .F. ) ;
#37829 = CIRCLE ( 'NONE', #4753, 1.000000000000000000 ) ;
#37830 = EDGE_CURVE ( 'NONE', #18426, #19145, #4075, .T. ) ;
#37831 = CARTESIAN_POINT ( 'NONE',  ( 9.201548168576595188, 26.54122646004460861, 10.50000000000000533 ) ) ;
#37832 = CARTESIAN_POINT ( 'NONE',  ( -5.578133564216450679, 24.05045924978193739, 20.99999999999999645 ) ) ;
#37833 = CIRCLE ( 'NONE', #25498, 21.00000000000002842 ) ;
#37834 = FACE_OUTER_BOUND ( 'NONE', #26072, .T. ) ;
#37835 = CARTESIAN_POINT ( 'NONE',  ( -15.34554945454190467, 9.014796822355112482, 10.00000000000000000 ) ) ;
#37836 = CIRCLE ( 'NONE', #23584, 1.000000000000000888 ) ;
#37837 = FACE_BOUND ( 'NONE', #39234, .T. ) ;
#37838 = CARTESIAN_POINT ( 'NONE',  ( 20.60789226802129548, 17.73598670052725623, 12.14047268033019300 ) ) ;
#37839 = CARTESIAN_POINT ( 'NONE',  ( -22.59715888466356049, 9.764328767929328023, -9.387076417448387389 ) ) ;
#37840 = CARTESIAN_POINT ( 'NONE',  ( 13.26265854479622419, -15.63203989815269779, -29.26899939535988437 ) ) ;
#37841 = DIRECTION ( 'NONE',  ( 0.000000000000000000, 0.000000000000000000, 1.000000000000000000 ) ) ;
#37842 = EDGE_CURVE ( 'NONE', #634, #29140, #18994, .T. ) ;
#37843 = CARTESIAN_POINT ( 'NONE',  ( 15.17653370639157728, 26.59493482429561340, -7.821537767519052053 ) ) ;
#37844 = ORIENTED_EDGE ( 'NONE', *, *, #25976, .F. ) ;
#37845 = CARTESIAN_POINT ( 'NONE',  ( -14.56238555350499020, 22.71997793191525616, -13.57281493169755571 ) ) ;
#37846 = CARTESIAN_POINT ( 'NONE',  ( -21.85869495254141270, -19.21667513322701382, 20.69868183039799447 ) ) ;
#37847 = AXIS2_PLACEMENT_3D ( 'NONE', #1218, #7094, #20108 ) ;
#37848 = CYLINDRICAL_SURFACE ( 'NONE', #4921, 0.5000000000000004441 ) ;
#37849 = CARTESIAN_POINT ( 'NONE',  ( 13.50802936482910610, 22.78328071161119794, -15.45283427980578139 ) ) ;
#37850 = B_SPLINE_CURVE_WITH_KNOTS ( 'NONE', 3,
 ( #9143, #12981, #6677, #37173, #201, #33931 ),
 .UNSPECIFIED., .F., .F.,
 ( 4, 2, 4 ),
 ( 0.000000000000000000, 0.5000000000000000000, 1.000000000000000000 ),
 .UNSPECIFIED. ) ;
#37851 = ORIENTED_EDGE ( 'NONE', *, *, #13593, .F. ) ;
#37852 = CARTESIAN_POINT ( 'NONE',  ( 18.02495589071083160, -9.945986095653781334, -28.44476012898337203 ) ) ;
#37853 = DIRECTION ( 'NONE',  ( 0.000000000000000000, 0.000000000000000000, 1.000000000000000000 ) ) ;
#37854 = ORIENTED_EDGE ( 'NONE', *, *, #28729, .F. ) ;
#37856 = DIRECTION ( 'NONE',  ( 0.000000000000000000, 0.000000000000000000, 1.000000000000000000 ) ) ;
#37855 = CARTESIAN_POINT ( 'NONE',  ( -15.11187235763720160, 27.11521598415787437, -7.341895426520673062 ) ) ;
#37857 = CARTESIAN_POINT ( 'NONE',  ( -13.24241402396536849, -21.98623490292562721, -17.32878092716321561 ) ) ;
#37858 = CARTESIAN_POINT ( 'NONE',  ( -9.541476348891238857, 27.59512447410525127, 6.000000000000000000 ) ) ;
#37859 = AXIS2_PLACEMENT_3D ( 'NONE', #16007, #371, #25535 ) ;
#37860 = ORIENTED_EDGE ( 'NONE', *, *, #4683, .F. ) ;
#37861 = CARTESIAN_POINT ( 'NONE',  ( -30.04644516860189185, -14.57369536713954083, -12.89617642488422966 ) ) ;
#37862 = CARTESIAN_POINT ( 'NONE',  ( -10.24989465074190420, -20.12788835074411864, -21.68738911211123721 ) ) ;
#37863 = DIRECTION ( 'NONE',  ( 0.000000000000000000, 0.000000000000000000, -1.000000000000000000 ) ) ;
#37864 = CARTESIAN_POINT ( 'NONE',  ( 16.87377372029358469, 22.19217076240406428, -5.475293046584253531 ) ) ;
#37865 = EDGE_LOOP ( 'NONE', ( #34534, #39576, #7438, #12043, #29237 ) ) ;
#37866 = CARTESIAN_POINT ( 'NONE',  ( 19.90281409743823815, 5.211047685906170734, -28.23787101014183420 ) ) ;
#37867 = DIRECTION ( 'NONE',  ( 1.000000000000000000, 0.000000000000000000, 0.000000000000000000 ) ) ;
#37868 = CARTESIAN_POINT ( 'NONE',  ( 7.249670636309310190, 35.63227325353309283, 7.102474990965859547 ) ) ;
#37869 = CARTESIAN_POINT ( 'NONE',  ( -10.51560177358055803, 33.07492339674077186, 10.49999999999999822 ) ) ;
#37870 = EDGE_LOOP ( 'NONE', ( #6501, #36668, #1925 ) ) ;
#37871 = CARTESIAN_POINT ( 'NONE',  ( -30.89143654367048342, -0.3087187454278746968, -7.347449338435406929 ) ) ;
#37872 = CARTESIAN_POINT ( 'NONE',  ( 26.66507754537762409, 0.03537578240675859353, -15.42101455173288649 ) ) ;
#37873 = CIRCLE ( 'NONE', #20374, 0.5000000000000004441 ) ;
#37874 = CARTESIAN_POINT ( 'NONE',  ( 26.58217467610746354, -19.30423083005467078, 19.99202127657103389 ) ) ;
#37875 = ORIENTED_EDGE ( 'NONE', *, *, #15094, .F. ) ;
#37876 = EDGE_CURVE ( 'NONE', #25343, #18018, #34574, .T. ) ;
#37877 = CARTESIAN_POINT ( 'NONE',  ( 17.81784622497951176, -13.85677843414110555, -19.80438750953540961 ) ) ;
#37878 = CIRCLE ( 'NONE', #27500, 1.000000000000000888 ) ;
#37879 = DIRECTION ( 'NONE',  ( 1.000000000000000000, 0.000000000000000000, 0.000000000000000000 ) ) ;
#37880 = ORIENTED_EDGE ( 'NONE', *, *, #10113, .F. ) ;
#37881 = LINE ( 'NONE', #119, #21025 ) ;
#37882 = CIRCLE ( 'NONE', #19074, 57.00000000000003553 ) ;
#37883 = CARTESIAN_POINT ( 'NONE',  ( -11.28725060478854303, 31.99026972875184427, 10.94387467463334396 ) ) ;
#37884 = DIRECTION ( 'NONE',  ( -0.000000000000000000, -0.000000000000000000, -1.000000000000000000 ) ) ;
#37885 = CARTESIAN_POINT ( 'NONE',  ( 5.962758689501411524, 36.33297212300762880, -8.430188468140666913 ) ) ;
#37886 = PLANE ( 'NONE',  #36050 ) ;
#37887 = ORIENTED_EDGE ( 'NONE', *, *, #29990, .T. ) ;
#37888 = FACE_OUTER_BOUND ( 'NONE', #11621, .T. ) ;
#37889 = DIRECTION ( 'NONE',  ( 0.9781476007338067991, 0.2079116908177533751, 0.000000000000000000 ) ) ;
#37890 = CARTESIAN_POINT ( 'NONE',  ( 16.99588821486303303, -13.03532880417942508, -25.61570463410847154 ) ) ;
#37891 = DIRECTION ( 'NONE',  ( -0.4067366430757888840, 0.9135454576426058626, 0.000000000000000000 ) ) ;
#37892 = PLANE ( 'NONE',  #31984 ) ;
#37893 = EDGE_CURVE ( 'NONE', #15410, #761, #15108, .T. ) ;
#37894 = CARTESIAN_POINT ( 'NONE',  ( -15.41558956984166251, 26.78481017248024898, -5.000000000000000000 ) ) ;
#37895 = CARTESIAN_POINT ( 'NONE',  ( 10.43719446462658240, 17.70184934034695345, -28.68331232917914164 ) ) ;
#37896 = CARTESIAN_POINT ( 'NONE',  ( -6.913051850451354952, 35.81219556108709412, 7.382773698552463237 ) ) ;
#37897 = VERTEX_POINT ( 'NONE', #38823 ) ;
#37899 = CARTESIAN_POINT ( 'NONE',  ( 2.538198952020652044, 7.704401919100519081, 10.49999999999999822 ) ) ;
#37898 = CARTESIAN_POINT ( 'NONE',  ( -14.97620661933688346, 15.43604710290467708, -23.16381367993152907 ) ) ;
#37900 = AXIS2_PLACEMENT_3D ( 'NONE', #34903, #31651, #26358 ) ;
#37901 = CARTESIAN_POINT ( 'NONE',  ( 13.30684945990800649, 15.76689945427723138, 10.49999999999999822 ) ) ;
#37902 = EDGE_CURVE ( 'NONE', #3653, #16261, #17061, .T. ) ;
#37903 = CARTESIAN_POINT ( 'NONE',  ( 9.684905122972589098, -18.44378311763584577, -26.83090883577152397 ) ) ;
#37904 = FACE_OUTER_BOUND ( 'NONE', #30095, .T. ) ;
#37905 = CARTESIAN_POINT ( 'NONE',  ( 13.49439698208447602, 22.80992317807017500, -15.45087343220999010 ) ) ;
#37906 = ORIENTED_EDGE ( 'NONE', *, *, #7689, .T. ) ;
#37907 = CARTESIAN_POINT ( 'NONE',  ( 11.11724078106343683, 17.61836477313612193, -26.82968543565921848 ) ) ;
#37908 = PRODUCT ( 'Protective Travel Cap', 'Protective Travel Cap', '', ( #13191 ) ) ;
#37909 = ORIENTED_EDGE ( 'NONE', *, *, #23072, .T. ) ;
#37910 = LINE ( 'NONE', #741, #6877 ) ;
#37911 = CARTESIAN_POINT ( 'NONE',  ( -9.759121109861677468, -18.57581161978397688, -26.22736366997701651 ) ) ;
#37912 = CARTESIAN_POINT ( 'NONE',  ( -36.47501240582165849, -5.175470059597266470, 12.14047268033136362 ) ) ;
#37913 = AXIS2_PLACEMENT_3D ( 'NONE', #5477, #8734, #24762 ) ;
#37914 = ADVANCED_FACE ( 'NONE', ( #17506 ), #16899, .F. ) ;
#37915 = CARTESIAN_POINT ( 'NONE',  ( -21.53702042946260420, -15.83689332051200616, -18.64419367562588192 ) ) ;
#37916 = CARTESIAN_POINT ( 'NONE',  ( -3.457094704751060288, -20.82358164328624639, -24.37237690483107855 ) ) ;
#37917 = CARTESIAN_POINT ( 'NONE',  ( 11.59920991657710942, 17.45000162638225660, -26.26810536156576603 ) ) ;
#37918 = ORIENTED_EDGE ( 'NONE', *, *, #30628, .T. ) ;
#37919 = CARTESIAN_POINT ( 'NONE',  ( 18.58241799660420668, 8.688807075854512618, -29.42769849846112606 ) ) ;
#37920 = CARTESIAN_POINT ( 'NONE',  ( 19.26948696230199687, 27.85601271560034675, 11.00000000000000000 ) ) ;
#37921 = CARTESIAN_POINT ( 'NONE',  ( -6.553841457909052259, 36.68830644081907622, 16.87380292611438648 ) ) ;
#37922 = ORIENTED_EDGE ( 'NONE', *, *, #6409, .T. ) ;
#37923 = CARTESIAN_POINT ( 'NONE',  ( -20.59263868462731750, -3.100282240389482080, -27.20017962400196865 ) ) ;
#37924 = AXIS2_PLACEMENT_3D ( 'NONE', #8370, #23805, #33166 ) ;
#37925 = CARTESIAN_POINT ( 'NONE',  ( -16.81914744117433003, 21.75867863388409873, 16.30093088680929370 ) ) ;
#37926 = ORIENTED_EDGE ( 'NONE', *, *, #37150, .T. ) ;
#37927 = CARTESIAN_POINT ( 'NONE',  ( 11.11016527260166420, 31.83082137946473367, 7.000000000000000000 ) ) ;
#37928 = DIRECTION ( 'NONE',  ( 1.000000000000000000, 0.000000000000000000, 0.000000000000000000 ) ) ;
#37929 = ADVANCED_FACE ( 'NONE', ( #5295 ), #11002, .T. ) ;
#37930 = EDGE_CURVE ( 'NONE', #22181, #9989, #1449, .T. ) ;
#37931 = CARTESIAN_POINT ( 'NONE',  ( 27.50296097836364240, -12.04087961669551987, -15.70514145711053899 ) ) ;
#37932 = EDGE_CURVE ( 'NONE', #26220, #26306, #17101, .T. ) ;
#37933 = CARTESIAN_POINT ( 'NONE',  ( 32.28722999652137560, 1.315479119631175697, 12.14047268033097460 ) ) ;
#37934 = VERTEX_POINT ( 'NONE', #11601 ) ;
#37935 = ORIENTED_EDGE ( 'NONE', *, *, #18466, .T. ) ;
#37936 = PLANE ( 'NONE',  #37859 ) ;
#37937 = DIRECTION ( 'NONE',  ( -0.000000000000000000, -0.000000000000000000, 1.000000000000000000 ) ) ;
#37938 = B_SPLINE_CURVE_WITH_KNOTS ( 'NONE', 3,
 ( #19878, #29616, #14584, #11137, #8284, #17650 ),
 .UNSPECIFIED., .F., .F.,
 ( 4, 2, 4 ),
 ( 0.000000000000000000, 0.5000000000000000000, 1.000000000000000000 ),
 .UNSPECIFIED. ) ;
#37939 = CARTESIAN_POINT ( 'NONE',  ( 5.644276917315718123, 36.40655018617690786, 10.63089969389957368 ) ) ;
#37940 = ORIENTED_EDGE ( 'NONE', *, *, #39089, .T. ) ;
#37941 = CARTESIAN_POINT ( 'NONE',  ( -0.7532367600618588011, 38.47464941728308929, -5.855549327213532607 ) ) ;
#37942 = CARTESIAN_POINT ( 'NONE',  ( 8.195318570657093460, 10.36946087849375076, 11.00000000000000000 ) ) ;
#37943 = CARTESIAN_POINT ( 'NONE',  ( -4.724378136954611840, 12.76962061027129458, 12.00000000000000000 ) ) ;
#37944 = CIRCLE ( 'NONE', #2918, 1.000000000000000000 ) ;
#37945 = CARTESIAN_POINT ( 'NONE',  ( -3.835137251120299684, 29.44922644035488446, 13.00000000000000178 ) ) ;
#37946 = DIRECTION ( 'NONE',  ( 1.000000000000000000, 0.000000000000000000, 0.000000000000000000 ) ) ;
#37947 = ADVANCED_FACE ( 'NONE', ( #13834 ), #23387, .F. ) ;
#37948 = CARTESIAN_POINT ( 'NONE',  ( 10.72918489117954088, 32.98258515686300996, 7.000000000000000000 ) ) ;
#37949 = CARTESIAN_POINT ( 'NONE',  ( 13.30718649135118348, 26.63099661339894197, -12.38017239920473678 ) ) ;
#37951 = AXIS2_PLACEMENT_3D ( 'NONE', #8063, #29805, #7862 ) ;
#37950 = DIRECTION ( 'NONE',  ( -0.000000000000000000, -0.000000000000000000, 1.000000000000000000 ) ) ;
#37952 = ORIENTED_EDGE ( 'NONE', *, *, #36703, .F. ) ;
#37954 = LINE ( 'NONE', #34708, #19386 ) ;
#37953 = CARTESIAN_POINT ( 'NONE',  ( -18.82575331703998955, 11.22376865745672880, -20.12444327678071332 ) ) ;
#37955 = CARTESIAN_POINT ( 'NONE',  ( -10.37659644360344835, 39.73422260060537781, 22.99999999999811351 ) ) ;
#37956 = EDGE_CURVE ( 'NONE', #22041, #9605, #7936, .T. ) ;
#37957 = CARTESIAN_POINT ( 'NONE',  ( 14.80057364270156484, -25.66573095307622054, -10.17772232356911211 ) ) ;
#37958 = CARTESIAN_POINT ( 'NONE',  ( -0.9999999999999993339, 33.00000000000000000, 10.50000000000000178 ) ) ;
#37959 = CARTESIAN_POINT ( 'NONE',  ( 15.14564224390120373, 26.37900145172237032, -8.294075276387847140 ) ) ;
#37960 = CARTESIAN_POINT ( 'NONE',  ( -16.24796006241077961, 15.88921519459651499, -21.50719306941234876 ) ) ;
#37961 = CARTESIAN_POINT ( 'NONE',  ( 6.557822374958316658, 35.99981354310111215, 10.49999999999999822 ) ) ;
#37962 = CARTESIAN_POINT ( 'NONE',  ( -19.94212141337140665, -19.90605279271622408, -16.79278165465914796 ) ) ;
#37963 = CARTESIAN_POINT ( 'NONE',  ( 8.467881093281681260, -25.26349163305798839, -6.435158416897623468 ) ) ;
#37964 = CARTESIAN_POINT ( 'NONE',  ( 11.81931059556923103, 18.78345403663103852, -22.75672908190094645 ) ) ;
#37965 = CARTESIAN_POINT ( 'NONE',  ( 29.70735205375613219, -21.47756445264377589, -9.292127997619706647 ) ) ;
#37966 = DIRECTION ( 'NONE',  ( -0.000000000000000000, -0.000000000000000000, 1.000000000000000000 ) ) ;
#37967 = CARTESIAN_POINT ( 'NONE',  ( -34.66483173867272427, 1.836754817265617623, 11.00000000000000000 ) ) ;
#37968 = ORIENTED_EDGE ( 'NONE', *, *, #1665, .F. ) ;
#37969 = CARTESIAN_POINT ( 'NONE',  ( -6.748174487910753250, 28.62818041414330850, -15.79635236281668931 ) ) ;
#37970 = VECTOR ( 'NONE', #31859, 1000.000000000000114 ) ;
#37971 = CARTESIAN_POINT ( 'NONE',  ( 14.97986028244560508, 21.52226669793674318, 10.49999999999999822 ) ) ;
#37972 = VERTEX_POINT ( 'NONE', #17707 ) ;
#37973 = CARTESIAN_POINT ( 'NONE',  ( 30.50043281132222717, -0.02822430422811177814, -7.827654197346148202 ) ) ;
#37974 = CARTESIAN_POINT ( 'NONE',  ( 14.63635198741554788, 25.78286467897733303, 7.000000000000000000 ) ) ;
#37975 = DIRECTION ( 'NONE',  ( -0.000000000000000000, -0.000000000000000000, -1.000000000000000000 ) ) ;
#37976 = VERTEX_POINT ( 'NONE', #14238 ) ;
#37977 = AXIS2_PLACEMENT_3D ( 'NONE', #1952, #13924, #14125 ) ;
#37978 = CARTESIAN_POINT ( 'NONE',  ( -28.76033270383555518, 0.2571929453871795168, -11.60468438384830847 ) ) ;
#37979 = DIRECTION ( 'NONE',  ( 0.000000000000000000, 0.000000000000000000, 1.000000000000000000 ) ) ;
#37980 = ORIENTED_EDGE ( 'NONE', *, *, #25561, .F. ) ;
#37981 = CARTESIAN_POINT ( 'NONE',  ( 35.01769949592260645, -8.410817939179214164, -6.748082837904874509 ) ) ;
#37982 = EDGE_CURVE ( 'NONE', #481, #4731, #35380, .T. ) ;
#37983 = VECTOR ( 'NONE', #27306, 1000.000000000000000 ) ;
#37984 = CONICAL_SURFACE ( 'NONE', #375, 1.000000000000013101, 0.7853981633974579379 ) ;
#37985 = ORIENTED_EDGE ( 'NONE', *, *, #8762, .T. ) ;
#37986 = DIRECTION ( 'NONE',  ( 0.000000000000000000, 0.000000000000000000, 1.000000000000000000 ) ) ;
#37987 = CARTESIAN_POINT ( 'NONE',  ( 10.89111091687315813, 36.83121428896965455, 11.55979286843934695 ) ) ;
#37988 = DIRECTION ( 'NONE',  ( 1.000000000000000000, 0.000000000000000000, 0.000000000000000000 ) ) ;
#37989 = DIRECTION ( 'NONE',  ( 0.000000000000000000, 0.000000000000000000, 1.000000000000000000 ) ) ;
#37990 = CARTESIAN_POINT ( 'NONE',  ( 5.496198527381090493, 34.39821714758473803, 18.87996532025784902 ) ) ;
#37991 = DIRECTION ( 'NONE',  ( -0.000000000000000000, -0.000000000000000000, -1.000000000000000000 ) ) ;
#37992 = VERTEX_POINT ( 'NONE', #4898 ) ;
#37993 = SURFACE_STYLE_USAGE ( .BOTH. , #22542 ) ;
#37994 = LINE ( 'NONE', #10364, #35996 ) ;
#37995 = CARTESIAN_POINT ( 'NONE',  ( 4.817371740575539185, 23.83900317890011422, 23.00000000000000000 ) ) ;
#37996 = CARTESIAN_POINT ( 'NONE',  ( -4.096822963000303019, 8.035697679810709815, 10.50000000000000533 ) ) ;
#37997 = CARTESIAN_POINT ( 'NONE',  ( 15.17757647933641785, 16.16795567397082678, -20.97689461799007304 ) ) ;
#37998 = CARTESIAN_POINT ( 'NONE',  ( 9.968257018404958814, 34.74234079311501233, -6.744892496327541842 ) ) ;
#37999 = VERTEX_POINT ( 'NONE', #29478 ) ;
#38000 = CARTESIAN_POINT ( 'NONE',  ( 12.67385491020283439, -21.41802064514664750, -18.35960277857459033 ) ) ;
#38001 = DIRECTION ( 'NONE',  ( 0.3535533905932766174, 0.6123724356957975790, -0.7071067811865433539 ) ) ;
#38002 = CIRCLE ( 'NONE', #17263, 1.000000000000000000 ) ;
#38003 = CARTESIAN_POINT ( 'NONE',  ( 10.44103466624280685, 32.57396620494213124, 7.000000000000000000 ) ) ;
#38004 = VERTEX_POINT ( 'NONE', #17305 ) ;
#38005 = CIRCLE ( 'NONE', #10783, 0.5000000000000004441 ) ;
#38006 = CARTESIAN_POINT ( 'NONE',  ( -15.34056339507122324, 26.60929180672939509, -6.888178519148794976 ) ) ;
#38007 = AXIS2_PLACEMENT_3D ( 'NONE', #18832, #2994, #31220 ) ;
#38008 = CARTESIAN_POINT ( 'NONE',  ( -20.64393337882609103, -27.21432092515239631, 16.30093088680190405 ) ) ;
#38009 = CARTESIAN_POINT ( 'NONE',  ( 13.52481987067865532, -24.53642209463285084, -12.56943988586981398 ) ) ;
#38010 = CARTESIAN_POINT ( 'NONE',  ( 19.48557158514982746, -11.25000000000009415, 3.000000000000000000 ) ) ;
#38011 = EDGE_LOOP ( 'NONE', ( #9201, #28672, #17347, #13235 ) ) ;
#38012 = ORIENTED_EDGE ( 'NONE', *, *, #9790, .T. ) ;
#38013 = CARTESIAN_POINT ( 'NONE',  ( -8.267738057345434655, 18.77097771606736032, -29.29219651185118067 ) ) ;
#38014 = CARTESIAN_POINT ( 'NONE',  ( -17.60052854559279467, -23.51059659377553501, -14.14515744271393238 ) ) ;
#38015 = FACE_BOUND ( 'NONE', #23288, .T. ) ;
#38016 = CARTESIAN_POINT ( 'NONE',  ( -20.25697106145711146, -4.992088383670172824, -27.10335080208274050 ) ) ;
#38017 = CARTESIAN_POINT ( 'NONE',  ( 9.593266739736579396, 18.11602540378440196, 10.50000000000000000 ) ) ;
#38018 = ORIENTED_EDGE ( 'NONE', *, *, #36090, .F. ) ;
#38019 = CARTESIAN_POINT ( 'NONE',  ( 24.47508212618827628, 0.6084701833738710430, -18.47132725458562419 ) ) ;
#38020 = CARTESIAN_POINT ( 'NONE',  ( 6.572794801194151049, 16.58182897866491956, 9.000000000000001776 ) ) ;
#38021 = DIRECTION ( 'NONE',  ( 1.000000000000000000, 0.000000000000000000, 0.000000000000000000 ) ) ;
#38022 = EDGE_LOOP ( 'NONE', ( #16005, #31442, #30459, #24842, #12936, #35573, #12252 ) ) ;
#38023 = CARTESIAN_POINT ( 'NONE',  ( -28.90304507515644517, 0.08656617661839061117, -11.59782457920430687 ) ) ;
#38024 = DIRECTION ( 'NONE',  ( 0.000000000000000000, 0.000000000000000000, 1.000000000000000000 ) ) ;
#38025 = ORIENTED_EDGE ( 'NONE', *, *, #18834, .T. ) ;
#38026 = CARTESIAN_POINT ( 'NONE',  ( 20.50882952253471103, -1.590216141173560249, -28.62054632307110680 ) ) ;
#38027 = CARTESIAN_POINT ( 'NONE',  ( 20.46225145915602894, 1.418922334520018591, -30.00000000000000355 ) ) ;
#38028 = CARTESIAN_POINT ( 'NONE',  ( 15.37000524124839274, -27.20210912714561857, 15.72805884748939498 ) ) ;
#38029 = EDGE_CURVE ( 'NONE', #42, #18984, #24120, .T. ) ;
#38030 = ORIENTED_EDGE ( 'NONE', *, *, #10865, .F. ) ;
#38031 = CARTESIAN_POINT ( 'NONE',  ( 1.824109939551872506, 39.35700678546974274, 15.13084544680213916 ) ) ;
#38032 = CONICAL_SURFACE ( 'NONE', #22444, 0.4999999999999980571, 0.7853981633974552734 ) ;
#38033 = DIRECTION ( 'NONE',  ( -0.6691306063588570163, 0.7431448254773952433, 0.000000000000000000 ) ) ;
#38034 = CARTESIAN_POINT ( 'NONE',  ( -5.410216727984581198, 24.65457866814584165, 20.99999999999995026 ) ) ;
#38035 = AXIS2_PLACEMENT_3D ( 'NONE', #29971, #26726, #14938 ) ;
#38036 = DIRECTION ( 'NONE',  ( 0.5000000000000038858, 0.8660254037844364872, -0.000000000000000000 ) ) ;
#38037 = EDGE_CURVE ( 'NONE', #1841, #8501, #14379, .T. ) ;
#38038 = AXIS2_PLACEMENT_3D ( 'NONE', #24873, #495, #25072 ) ;
#38039 = CYLINDRICAL_SURFACE ( 'NONE', #1997, 0.5000000000000004441 ) ;
#38040 = EDGE_CURVE ( 'NONE', #4736, #22293, #30626, .T. ) ;
#38041 = FACE_BOUND ( 'NONE', #8235, .T. ) ;
#38042 = CARTESIAN_POINT ( 'NONE',  ( 26.46356280838283936, 3.031871643931095317, 17.42190598799536616 ) ) ;
#38043 = CARTESIAN_POINT ( 'NONE',  ( -23.26956309474883966, 8.880304990950326882, -8.885970393110802945 ) ) ;
#38044 = CARTESIAN_POINT ( 'NONE',  ( 21.65887295875352692, -26.69628545518032325, -7.666996354092982635 ) ) ;
#38045 = DIRECTION ( 'NONE',  ( 0.9781476007338042455, -0.2079116908177664758, 0.000000000000000000 ) ) ;
#38046 = CARTESIAN_POINT ( 'NONE',  ( 13.41755757912196323, 22.96584331339203544, -15.43348952276526731 ) ) ;
#38047 = ORIENTED_EDGE ( 'NONE', *, *, #9565, .T. ) ;
#38048 = CARTESIAN_POINT ( 'NONE',  ( -15.41005911881606849, 24.37590047215257982, -9.731608369055816610 ) ) ;
#38049 = CARTESIAN_POINT ( 'NONE',  ( -28.40703083259910855, -13.04618529600556442, 20.50957957746029692 ) ) ;
#38050 = EDGE_CURVE ( 'NONE', #22627, #22029, #8548, .T. ) ;
#38051 = CARTESIAN_POINT ( 'NONE',  ( 10.75008043808897185, 32.97797437800703335, 10.49999999999999822 ) ) ;
#38052 = CARTESIAN_POINT ( 'NONE',  ( 13.79295119906300116, 23.34604900139666483, -14.47902606294586469 ) ) ;
#38053 = ORIENTED_EDGE ( 'NONE', *, *, #18908, .T. ) ;
#38054 = CARTESIAN_POINT ( 'NONE',  ( 26.45322076532816524, -14.58567879916042287, -15.67905774910988193 ) ) ;
#38055 = DIRECTION ( 'NONE',  ( 1.000000000000000000, -3.469446951953598806E-15, 0.000000000000000000 ) ) ;
#38056 = ORIENTED_EDGE ( 'NONE', *, *, #15225, .F. ) ;
#38058 = CARTESIAN_POINT ( 'NONE',  ( -7.312041872459064784, 25.58773265502866678, 6.000000000000000000 ) ) ;
#38057 = CARTESIAN_POINT ( 'NONE',  ( -12.79458690931549292, 21.87333156960552927, -17.40760258954136219 ) ) ;
#38059 = CARTESIAN_POINT ( 'NONE',  ( -16.75447718561904864, -27.02424154557581915, -5.468381619150384232 ) ) ;
#38060 = CARTESIAN_POINT ( 'NONE',  ( 12.41469063302487363, 14.32475803611739273, 10.49999999999999822 ) ) ;
#38061 = CIRCLE ( 'NONE', #17986, 0.9999999999999988898 ) ;
#38062 = ORIENTED_EDGE ( 'NONE', *, *, #13443, .F. ) ;
#38063 = CARTESIAN_POINT ( 'NONE',  ( -34.61197078468903499, -14.29155545462818111, -7.558879141708873206 ) ) ;
#38064 = CARTESIAN_POINT ( 'NONE',  ( -13.74012441838748622, -25.29379767668099888, -10.67230615080171496 ) ) ;
#38065 = FACE_OUTER_BOUND ( 'NONE', #3086, .T. ) ;
#38066 = CARTESIAN_POINT ( 'NONE',  ( 14.83232221668444595, 20.29379547517063997, -15.62825253669702263 ) ) ;
#38067 = ORIENTED_EDGE ( 'NONE', *, *, #19596, .T. ) ;
#38068 = CARTESIAN_POINT ( 'NONE',  ( 27.20667665144295455, 2.902151610605352872, -10.24982003146635812 ) ) ;
#38069 = CARTESIAN_POINT ( 'NONE',  ( 13.94482798346721353, 26.50521816028912525, 7.000000000000000000 ) ) ;
#38070 = CARTESIAN_POINT ( 'NONE',  ( 10.72918489117958174, 32.98258515686296732, 7.499999999999997335 ) ) ;
#38071 = ORIENTED_EDGE ( 'NONE', *, *, #37427, .T. ) ;
#38072 = CARTESIAN_POINT ( 'NONE',  ( -30.45015951236765517, -0.2748756232826376489, -8.751359642228980107 ) ) ;
#38073 = CARTESIAN_POINT ( 'NONE',  ( 30.48202640438653432, -0.5154105689507647581, -9.204797512474263144 ) ) ;
#38074 = CARTESIAN_POINT ( 'NONE',  ( 21.27405569407545372, -21.06385914081313970, 20.25080042701566896 ) ) ;
#38075 = ORIENTED_EDGE ( 'NONE', *, *, #8309, .T. ) ;
#38076 = EDGE_CURVE ( 'NONE', #17093, #38149, #30082, .T. ) ;
#38077 = CARTESIAN_POINT ( 'NONE',  ( 31.47283671532267846, -25.12609584734865464, -14.45070082761209207 ) ) ;
#38078 = CARTESIAN_POINT ( 'NONE',  ( -12.67417846324126174, 14.47720745114824226, 7.000000000000000000 ) ) ;
#38079 = EDGE_CURVE ( 'NONE', #28707, #36352, #21506, .T. ) ;
#38080 = CARTESIAN_POINT ( 'NONE',  ( -10.36702044712415116, 31.16169077310601665, 9.500000000000000000 ) ) ;
#38081 = AXIS2_PLACEMENT_3D ( 'NONE', #30739, #54, #9401 ) ;
#38082 = AXIS2_PLACEMENT_3D ( 'NONE', #550, #22079, #28575 ) ;
#38083 = CARTESIAN_POINT ( 'NONE',  ( -11.48173768534043404, 32.16538668264409040, 10.59344404201838152 ) ) ;
#38084 = CARTESIAN_POINT ( 'NONE',  ( 12.01837422881150275, 21.26636931122159169, 6.000000000000000000 ) ) ;
#38085 = CARTESIAN_POINT ( 'NONE',  ( -9.541476348891238857, 27.59512447410525127, 6.000000000000000000 ) ) ;
#38086 = ORIENTED_EDGE ( 'NONE', *, *, #33717, .T. ) ;
#38087 = CARTESIAN_POINT ( 'NONE',  ( 5.947717410344607103, 34.62949535663720724, 9.500000000000000000 ) ) ;
#38088 = DIRECTION ( 'NONE',  ( 0.000000000000000000, -0.000000000000000000, -1.000000000000000000 ) ) ;
#38089 = CARTESIAN_POINT ( 'NONE',  ( 19.98643085710752132, -17.36878015847262446, -18.71496154814925461 ) ) ;
#38090 = VECTOR ( 'NONE', #1161, 1000.000000000000000 ) ;
#38091 = FACE_OUTER_BOUND ( 'NONE', #34617, .T. ) ;
#38092 = DIRECTION ( 'NONE',  ( 1.000000000000000000, 0.000000000000000000, 0.000000000000000000 ) ) ;
#38093 = CARTESIAN_POINT ( 'NONE',  ( 14.32388773374254320, 25.53991067870101972, -11.55678267441725460 ) ) ;
#38094 = AXIS2_PLACEMENT_3D ( 'NONE', #3368, #34454, #5825 ) ;
#38095 = FACE_OUTER_BOUND ( 'NONE', #33989, .T. ) ;
#38096 = VERTEX_POINT ( 'NONE', #7536 ) ;
#38098 = DIRECTION ( 'NONE',  ( 1.000000000000000000, 0.000000000000000000, 0.000000000000000000 ) ) ;
#38097 = CARTESIAN_POINT ( 'NONE',  ( -14.58236326528782989, 14.81821449170132787, -26.51297324595556759 ) ) ;
#38099 = FACE_OUTER_BOUND ( 'NONE', #35603, .T. ) ;
#38100 = ADVANCED_FACE ( 'NONE', ( #14645 ), #19939, .F. ) ;
#38101 = CARTESIAN_POINT ( 'NONE',  ( 15.01285564717599463, -26.13052058328588956, -8.768336206249326636 ) ) ;
#38102 = ADVANCED_FACE ( 'NONE', ( #39618 ), #9353, .T. ) ;
#38103 = PLANE ( 'NONE',  #30853 ) ;
#38104 = CARTESIAN_POINT ( 'NONE',  ( 11.18751224735468597, 17.75405741225261735, -26.22522718368986361 ) ) ;
#38105 = ORIENTED_EDGE ( 'NONE', *, *, #39843, .F. ) ;
#38106 = CARTESIAN_POINT ( 'NONE',  ( 15.41298789278284964, 26.79417030376202291, -5.000000000000000000 ) ) ;
#38107 = VERTEX_POINT ( 'NONE', #9348 ) ;
#38109 = CARTESIAN_POINT ( 'NONE',  ( 14.26729173199937861, 26.60999298350824560, 10.87262190629280845 ) ) ;
#38108 = CARTESIAN_POINT ( 'NONE',  ( -15.31337224364676430, 26.70488253798198031, -6.886087685327574093 ) ) ;
#38110 = CARTESIAN_POINT ( 'NONE',  ( -11.86903598408506610, -21.48771982887699750, -18.45589563282124601 ) ) ;
#38111 = CARTESIAN_POINT ( 'NONE',  ( -22.63199090478729403, -28.51917565629995721, 13.92931973827765901 ) ) ;
#38112 = CARTESIAN_POINT ( 'NONE',  ( -31.37628010478545804, -21.64920164695394789, -6.699869314472419290 ) ) ;
#38113 = CARTESIAN_POINT ( 'NONE',  ( -2.493492096549495773, -24.25124555584876518, -10.38337496618507849 ) ) ;
#38114 = CARTESIAN_POINT ( 'NONE',  ( 11.41005643133681957, 17.03110932016596735, -30.00000000000000000 ) ) ;
#38115 = EDGE_LOOP ( 'NONE', ( #24623, #6437, #25033, #15172 ) ) ;
#38116 = CARTESIAN_POINT ( 'NONE',  ( 22.83139634148907504, 9.074226536428001921, -10.36981227567709318 ) ) ;
#38117 = CARTESIAN_POINT ( 'NONE',  ( 34.79718219320302097, -16.04917476651427677, -4.999999999999997335 ) ) ;
#38118 = CARTESIAN_POINT ( 'NONE',  ( 11.49020332972282432, 32.25361022348394613, 17.42190598798394774 ) ) ;
#38119 = ORIENTED_EDGE ( 'NONE', *, *, #25740, .F. ) ;
#38120 = CARTESIAN_POINT ( 'NONE',  ( -32.45035485798955222, -3.331808296535164970, -9.070745509778980420 ) ) ;
#38121 = AXIS2_PLACEMENT_3D ( 'NONE', #29285, #25827, #10397 ) ;
#38122 = AXIS2_PLACEMENT_3D ( 'NONE', #9653, #31180, #15340 ) ;
#38123 = CARTESIAN_POINT ( 'NONE',  ( -20.38546294303667139, 5.309590202434897321, 19.66345542862530138 ) ) ;
#38124 = ORIENTED_EDGE ( 'NONE', *, *, #33997, .T. ) ;
#38125 = LINE ( 'NONE', #19236, #38191 ) ;
#38126 = CARTESIAN_POINT ( 'NONE',  ( 3.485571585149744411, -11.24999999999998224, 10.00000000000000000 ) ) ;
#38127 = CIRCLE ( 'NONE', #23199, 0.5000000000000004441 ) ;
#38128 = EDGE_CURVE ( 'NONE', #30397, #4798, #2651, .T. ) ;
#38129 = CARTESIAN_POINT ( 'NONE',  ( 19.59228734373462899, -7.919684095842580263, -26.29579143822741827 ) ) ;
#38131 = AXIS2_PLACEMENT_3D ( 'NONE', #37479, #29481, #25470 ) ;
#38130 = CARTESIAN_POINT ( 'NONE',  ( 36.90241796781165107, -7.097865958169077061, 12.73282698324860007 ) ) ;
#38132 = ORIENTED_EDGE ( 'NONE', *, *, #35993, .T. ) ;
#38133 = ORIENTED_EDGE ( 'NONE', *, *, #26435, .F. ) ;
#38134 = DIRECTION ( 'NONE',  ( 1.000000000000000000, 0.000000000000000000, 0.000000000000000000 ) ) ;
#38135 = DIRECTION ( 'NONE',  ( 0.000000000000000000, 0.000000000000000000, 1.000000000000000000 ) ) ;
#38136 = DIRECTION ( 'NONE',  ( 1.000000000000000000, 0.000000000000000000, 0.000000000000000000 ) ) ;
#38137 = ORIENTED_EDGE ( 'NONE', *, *, #25292, .F. ) ;
#38138 = CARTESIAN_POINT ( 'NONE',  ( -0.4159103488080192479, 21.44268089392220134, -25.57552980935893672 ) ) ;
#38139 = FACE_OUTER_BOUND ( 'NONE', #8803, .T. ) ;
#38140 = CARTESIAN_POINT ( 'NONE',  ( -4.141337746071314996, 43.73298676078094616, 10.00000000000000000 ) ) ;
#38141 = AXIS2_PLACEMENT_3D ( 'NONE', #33, #16271, #436 ) ;
#38142 = PLANE ( 'NONE',  #3323 ) ;
#38143 = CARTESIAN_POINT ( 'NONE',  ( -3.295881626406750975, 9.398963235502531433, 10.50000000000000000 ) ) ;
#38144 = DIRECTION ( 'NONE',  ( 0.1277282058446098378, 0.8064441531181054668, 0.5773502691896305050 ) ) ;
#38145 = VECTOR ( 'NONE', #1610, 1000.000000000000000 ) ;
#38146 = CARTESIAN_POINT ( 'NONE',  ( 13.64911103968386108, 28.40416279045285108, -10.02753699536989451 ) ) ;
#38147 = CARTESIAN_POINT ( 'NONE',  ( -9.331903152615899089, 11.35703883385581037, 11.00000000000000000 ) ) ;
#38148 = AXIS2_PLACEMENT_3D ( 'NONE', #34624, #6777, #19179 ) ;
#38149 = VERTEX_POINT ( 'NONE', #15641 ) ;
#38151 = DIRECTION ( 'NONE',  ( -0.7275037805840933736, 0.3706816908110012188, 0.5773502691896389427 ) ) ;
#38150 = CARTESIAN_POINT ( 'NONE',  ( -19.84768973869175923, 14.36017750439766871, -9.881426833975718083 ) ) ;
#38152 = CARTESIAN_POINT ( 'NONE',  ( -17.76739295965093390, 31.93461338995377830, 22.99999999999999289 ) ) ;
#38153 = CARTESIAN_POINT ( 'NONE',  ( 12.32002675448889661, -22.02230990502341967, -17.43383621429965302 ) ) ;
#38154 = LINE ( 'NONE', #34914, #34726 ) ;
#38155 = CARTESIAN_POINT ( 'NONE',  ( 15.27745585280835705, 26.57502206593006022, -7.356517642319687411 ) ) ;
#38156 = CIRCLE ( 'NONE', #13499, 1.000000000000000888 ) ;
#38157 = CARTESIAN_POINT ( 'NONE',  ( -35.84808252048276955, -3.038699442442200027, -5.000000000000002665 ) ) ;
#38158 = DIRECTION ( 'NONE',  ( 0.000000000000000000, 0.000000000000000000, 1.000000000000000000 ) ) ;
#38159 = EDGE_CURVE ( 'NONE', #29611, #16505, #8748, .T. ) ;
#38160 = VECTOR ( 'NONE', #30689, 1000.000000000000000 ) ;
#38161 = CARTESIAN_POINT ( 'NONE',  ( -26.03722647915365584, -25.89241862741840094, -5.442903191855394063 ) ) ;
#38162 = CARTESIAN_POINT ( 'NONE',  ( 5.759131531303930629, -23.85034579298850232, -12.81924329913233152 ) ) ;
#38163 = CARTESIAN_POINT ( 'NONE',  ( 13.56948375875568580, 22.66347568585478101, -15.46163780264717147 ) ) ;
#38164 = B_SPLINE_CURVE_WITH_KNOTS ( 'NONE', 3,
 ( #15053, #27644, #11417, #33363, #39831, #14660, #36790, #27051, #40026, #39436 ),
 .UNSPECIFIED., .F., .F.,
 ( 4, 1, 1, 1, 1, 1, 1, 4 ),
 ( 0.1282122296533009798, 0.2500000000108080211, 0.3749999999994781952, 0.4999999999881489243, 0.6249999999768196535, 0.7499999999654909377, 0.8749999999541600015, 1.000000000000000000 ),
 .UNSPECIFIED. ) ;
#38165 = CARTESIAN_POINT ( 'NONE',  ( 31.11517615530266667, -21.06909056454590612, -7.976281376848859850 ) ) ;
#38166 = CARTESIAN_POINT ( 'NONE',  ( -19.48557158514998022, -11.24999999999982414, 2.999999999999999112 ) ) ;
#38167 = DIRECTION ( 'NONE',  ( 0.000000000000000000, 0.000000000000000000, 1.000000000000000000 ) ) ;
#38168 = ORIENTED_EDGE ( 'NONE', *, *, #33215, .F. ) ;
#38169 = CARTESIAN_POINT ( 'NONE',  ( -5.552924998094717957, 23.69300943437540852, -20.85599012649669959 ) ) ;
#38170 = ORIENTED_EDGE ( 'NONE', *, *, #4307, .F. ) ;
#38171 = DIRECTION ( 'NONE',  ( 1.000000000000000000, 0.000000000000000000, 0.000000000000000000 ) ) ;
#38172 = ORIENTED_EDGE ( 'NONE', *, *, #2619, .F. ) ;
#38173 = CARTESIAN_POINT ( 'NONE',  ( 28.37209621850218610, 0.09959924578248532945, -12.54634125719528370 ) ) ;
#38174 = DIRECTION ( 'NONE',  ( 0.5000000000000039968, 0.8660254037844363761, 0.000000000000000000 ) ) ;
#38175 = LINE ( 'NONE', #28428, #24554 ) ;
#38176 = ORIENTED_EDGE ( 'NONE', *, *, #37430, .F. ) ;
#38177 = CARTESIAN_POINT ( 'NONE',  ( -20.47826699597012023, 0.9446083685552523201, -30.00000000000000000 ) ) ;
#38178 = DIRECTION ( 'NONE',  ( -0.4067366430757888840, 0.9135454576426058626, 0.000000000000000000 ) ) ;
#38179 = EDGE_CURVE ( 'NONE', #40188, #14045, #7230, .T. ) ;
#38180 = ORIENTED_EDGE ( 'NONE', *, *, #17341, .T. ) ;
#38181 = CARTESIAN_POINT ( 'NONE',  ( 21.88878013244432097, -5.201535098629216591, -23.24105192260414654 ) ) ;
#38182 = AXIS2_PLACEMENT_3D ( 'NONE', #28614, #9338, #22507 ) ;
#38183 = EDGE_CURVE ( 'NONE', #24444, #18928, #31084, .T. ) ;
#38184 = ORIENTED_EDGE ( 'NONE', *, *, #3166, .T. ) ;
#38185 = DIRECTION ( 'NONE',  ( 0.000000000000000000, 0.000000000000000000, 1.000000000000000000 ) ) ;
#38186 = CARTESIAN_POINT ( 'NONE',  ( -17.34253826607193361, 27.32041144404004385, 11.55979286843934872 ) ) ;
#38187 = AXIS2_PLACEMENT_3D ( 'NONE', #27303, #5166, #11466 ) ;
#38188 = DIRECTION ( 'NONE',  ( -0.3090169943749434545, 0.9510565162951548634, 0.000000000000000000 ) ) ;
#38189 = DIRECTION ( 'NONE',  ( 0.9135454576426059736, 0.4067366430757888285, 0.000000000000000000 ) ) ;
#38190 = CARTESIAN_POINT ( 'NONE',  ( 9.417371715876635463, 30.49428522466168090, 19.27171037444157875 ) ) ;
#38191 = VECTOR ( 'NONE', #3797, 999.9999999999997726 ) ;
#38192 = EDGE_CURVE ( 'NONE', #27233, #27267, #36576, .T. ) ;
#38193 = DIRECTION ( 'NONE',  ( 1.000000000000000000, 0.000000000000000000, 0.000000000000000000 ) ) ;
#38194 = VERTEX_POINT ( 'NONE', #21138 ) ;
#38195 = FILL_AREA_STYLE ('',( #19910 ) ) ;
#38196 = DIRECTION ( 'NONE',  ( -0.000000000000000000, 0.000000000000000000, -1.000000000000000000 ) ) ;
#38197 = DIRECTION ( 'NONE',  ( 0.4999999999999919509, -0.8660254037844432595, 0.000000000000000000 ) ) ;
#38198 = DIRECTION ( 'NONE',  ( 1.000000000000000000, 0.000000000000000000, 0.000000000000000000 ) ) ;
#38199 = CARTESIAN_POINT ( 'NONE',  ( 17.52599447534131727, 19.76765755371411615, -8.359901029784603921 ) ) ;
#38200 = CARTESIAN_POINT ( 'NONE',  ( 11.51234731484127138, 32.76683130581704972, -8.088018125610085818 ) ) ;
#38201 = EDGE_LOOP ( 'NONE', ( #4347, #38170, #1957 ) ) ;
#38202 = CARTESIAN_POINT ( 'NONE',  ( 12.01837422881150275, 21.26636931122159169, 12.00000000000000000 ) ) ;
#38203 = CARTESIAN_POINT ( 'NONE',  ( 2.835130509701798918, 15.55077355964573904, 6.000000000000000000 ) ) ;
#38204 = CARTESIAN_POINT ( 'NONE',  ( 11.52690546367544222, -19.81741541769655512, -21.52521232598608947 ) ) ;
#38205 = CARTESIAN_POINT ( 'NONE',  ( 15.12590024503159292, -28.14827041158713072, 13.92931973827808712 ) ) ;
#38206 = EDGE_CURVE ( 'NONE', #33852, #36571, #5929, .T. ) ;
#38207 = DIRECTION ( 'NONE',  ( 0.000000000000000000, 0.000000000000000000, 1.000000000000000000 ) ) ;
#38208 = ADVANCED_FACE ( 'NONE', ( #36381 ), #32566, .T. ) ;
#38209 = CIRCLE ( 'NONE', #14869, 1.000000000000000000 ) ;
#38210 = ORIENTED_EDGE ( 'NONE', *, *, #19815, .F. ) ;
#38212 = AXIS2_PLACEMENT_3D ( 'NONE', #39154, #2193, #2392 ) ;
#38211 = CARTESIAN_POINT ( 'NONE',  ( -11.49511999468828272, 18.42800739041194902, -23.85559909385690247 ) ) ;
#38213 = CARTESIAN_POINT ( 'NONE',  ( -35.17699530642141781, -14.40920341950810268, 16.30093088680190050 ) ) ;
#38214 = CARTESIAN_POINT ( 'NONE',  ( 14.94022627794961089, -26.48256000415716471, -6.888844992090954911 ) ) ;
#38215 = DIRECTION ( 'NONE',  ( -0.9945218953682729568, 0.1045284632676569958, 0.000000000000000000 ) ) ;
#38216 = ORIENTED_EDGE ( 'NONE', *, *, #23647, .T. ) ;
#38217 = ORIENTED_EDGE ( 'NONE', *, *, #21800, .T. ) ;
#38218 = AXIS2_PLACEMENT_3D ( 'NONE', #31542, #3707, #22385 ) ;
#38219 = CARTESIAN_POINT ( 'NONE',  ( -8.958378443170586181, 18.74800665029167135, -27.28932216422303370 ) ) ;
#38220 = CARTESIAN_POINT ( 'NONE',  ( -18.91388186588683240, 35.25980436007201035, 10.00000000000000000 ) ) ;
#38221 = FACE_BOUND ( 'NONE', #15439, .T. ) ;
#38222 = CARTESIAN_POINT ( 'NONE',  ( -35.03892046201376331, -7.681061316508860592, -5.883781484302339493 ) ) ;
#38223 = CARTESIAN_POINT ( 'NONE',  ( -10.44103466624267540, 32.57396620494226624, 11.00000000000000000 ) ) ;
#38224 = ORIENTED_EDGE ( 'NONE', *, *, #40163, .T. ) ;
#38225 = CARTESIAN_POINT ( 'NONE',  ( 20.68604710019807769, 0.9517672083310861897, -27.45507450208132738 ) ) ;
#38226 = CARTESIAN_POINT ( 'NONE',  ( 8.118377661053333583, 10.47536095541699197, 11.00000000000000000 ) ) ;
#38227 = DIRECTION ( 'NONE',  ( -1.000000000000000000, 0.000000000000000000, 0.000000000000000000 ) ) ;
#38228 = ORIENTED_EDGE ( 'NONE', *, *, #32101, .F. ) ;
#38229 = CARTESIAN_POINT ( 'NONE',  ( -27.15044877466180751, 0.2209970037928831732, -14.47560764752908824 ) ) ;
#38230 = DIRECTION ( 'NONE',  ( -0.9135454576426059736, -0.4067366430757887730, 0.000000000000000000 ) ) ;
#38231 = EDGE_CURVE ( 'NONE', #38004, #25412, #8948, .T. ) ;
#38232 = ORIENTED_EDGE ( 'NONE', *, *, #23281, .T. ) ;
#38233 = CARTESIAN_POINT ( 'NONE',  ( 21.07461541020998297, -1.002319088913975476, -26.06574103777582962 ) ) ;
#38234 = CARTESIAN_POINT ( 'NONE',  ( 20.16769042714938109, -3.693422412194586446, -29.99999999999997868 ) ) ;
#38235 = CARTESIAN_POINT ( 'NONE',  ( 35.04992612853292400, -12.66836002548405382, 16.87380292611442201 ) ) ;
#38236 = EDGE_CURVE ( 'NONE', #14728, #17047, #2851, .T. ) ;
#38237 = ORIENTED_EDGE ( 'NONE', *, *, #6469, .F. ) ;
#38238 = CARTESIAN_POINT ( 'NONE',  ( 5.381339405376090568, 38.47497618056186042, 15.13084544680213561 ) ) ;
#38239 = DIRECTION ( 'NONE',  ( 1.000000000000000000, 0.000000000000000000, 0.000000000000000000 ) ) ;
#38240 = CARTESIAN_POINT ( 'NONE',  ( -3.428976547227685856, 28.19475011768389905, 20.94377226548358450 ) ) ;
#38241 = CIRCLE ( 'NONE', #18784, 6.000000000000003553 ) ;
#38242 = CARTESIAN_POINT ( 'NONE',  ( 5.724371395536106633, 32.23037938972932892, 6.000000000000000000 ) ) ;
#38243 = DIRECTION ( 'NONE',  ( 1.000000000000000000, 0.000000000000000000, 0.000000000000000000 ) ) ;
#38244 = CIRCLE ( 'NONE', #29172, 0.5000000000000011102 ) ;
#38245 = B_SPLINE_SURFACE_WITH_KNOTS ( 'NONE', 3, 3, ( 
 ( #5961, #34203, #37647, #12858, #16111, #9817, #28497 ),
 ( #22194, #34597, #9623, #6750, #19154, #670, #75 ),
 ( #25439, #31546, #37838, #18366, #3710, #27899, #15708 ),
 ( #24852, #6165, #10013, #30761, #2922, #15310, #27696 ),
 ( #12265, #12459, #18764, #40088, #22003, #24653, #37047 ),
 ( #31153, #9217, #34402, #21602, #3317, #34007, #18567 ),
 ( #28096, #275, #30952, #12660, #37447, #10211, #7766 ),
 ( #31750, #35608, #32156, #3912, #31944, #35005, #26047 ),
 ( #20169, #1077, #38447, #4316, #35404, #16922, #23001 ),
 ( #25846, #10620, #26453, #38853, #32565, #4110, #38247 ),
 ( #11029, #35197, #10415, #4724, #13453, #16517, #1683 ),
 ( #7563, #22797, #13252, #34796, #7355, #38042, #16311 ),
 ( #26254, #28900, #28694, #17131, #19758, #38650, #16719 ),
 ( #29103, #873, #22596, #1276, #23211, #13658, #4523 ),
 ( #19964, #14060, #32364, #29306, #29506, #1478, #6946 ),
 ( #13865, #10822, #25644, #19353, #7154, #19553, #36213 ),
 ( #5126, #23413, #33373, #39247, #11427, #23811, #24011 ),
 ( #14465, #27062, #15065, #27455, #36606, #20575, #26858 ),
 ( #39841, #8378, #20776, #8772, #29906, #32971, #30518 ),
 ( #11819, #39447, #2085, #1888, #35806, #33171, #26656 ),
 ( #18129, #14873, #17532, #32768, #21164, #5322, #27258 ),
 ( #8170, #11628, #33569, #7962, #17734, #2484, #8568 ),
 ( #39646, #5719, #24207, #5516, #20968, #30111, #17930 ),
 ( #29706, #11224, #20375, #2282, #2678, #14672, #36406 ),
 ( #30314, #4926, #17332, #14267, #39046, #23615, #36011 ) ),
 .UNSPECIFIED., .F., .F., .F.,
 ( 4, 3, 3, 3, 3, 3, 3, 3, 4 ),
 ( 4, 3, 4 ),
 ( 0.000000000000000000, 0.1250000000000000000, 0.2500000000000000000, 0.3750000000000000000, 0.5000000000000000000, 0.6250000000000000000, 0.7500000000000000000, 0.8750000000000000000, 1.000000000000000000 ),
 ( 3.412702215524944904, 3.665191429188091377, 3.917680642851237405 ),
 .UNSPECIFIED. ) ;
#38246 = FACE_BOUND ( 'NONE', #34866, .T. ) ;
#38247 = CARTESIAN_POINT ( 'NONE',  ( 30.90861030616866856, -0.03770625498867555270, 16.30093088680190405 ) ) ;
#38248 = CARTESIAN_POINT ( 'NONE',  ( -19.05143584731581186, 7.817709358104996120, -27.71748753264345311 ) ) ;
#38249 = CARTESIAN_POINT ( 'NONE',  ( 13.24265028322465731, -16.59376028717886342, -25.88933090075440191 ) ) ;
#38250 = CARTESIAN_POINT ( 'NONE',  ( 6.953805871968278929, 30.22298757065274444, 12.00000000000000000 ) ) ;
#38251 = ORIENTED_EDGE ( 'NONE', *, *, #24420, .T. ) ;
#38252 = CARTESIAN_POINT ( 'NONE',  ( 15.04512796001890074, 26.32317767946528164, -8.759451899191230240 ) ) ;
#38253 = EDGE_LOOP ( 'NONE', ( #11218, #6464, #39214, #34220 ) ) ;
#38254 = CARTESIAN_POINT ( 'NONE',  ( -15.85862229823199776, 25.25472105652747246, -5.474027676197895431 ) ) ;
#38255 = CARTESIAN_POINT ( 'NONE',  ( -27.71565130972494728, -3.171757977841499709, 19.66345542862529072 ) ) ;
#38256 = CYLINDRICAL_SURFACE ( 'NONE', #13347, 1.000000000000000888 ) ;
#38257 = CARTESIAN_POINT ( 'NONE',  ( 11.08276198488759867, 17.39680518735769965, -28.07995138869140206 ) ) ;
#38258 = VERTEX_POINT ( 'NONE', #27831 ) ;
#38259 = CARTESIAN_POINT ( 'NONE',  ( 18.60907781376031522, -9.552212779558386657, -26.96908054186706494 ) ) ;
#38260 = EDGE_CURVE ( 'NONE', #21617, #36923, #202, .T. ) ;
#38261 = CARTESIAN_POINT ( 'NONE',  ( 13.64210930126480115, 24.20081211342298744, 12.00000000000000000 ) ) ;
#38262 = ORIENTED_EDGE ( 'NONE', *, *, #33904, .F. ) ;
#38264 = CARTESIAN_POINT ( 'NONE',  ( 8.118377661053324701, 10.47536095541698486, 7.000000000000000000 ) ) ;
#38263 = CARTESIAN_POINT ( 'NONE',  ( -14.87679345494665029, 26.41285975656771612, -9.216490526136041694 ) ) ;
#38265 = CARTESIAN_POINT ( 'NONE',  ( -16.11582280033900005, -26.76908378381648390, -6.872361183095262227 ) ) ;
#38266 = LINE ( 'NONE', #29123, #7467 ) ;
#38267 = VECTOR ( 'NONE', #17082, 1000.000000000000000 ) ;
#38268 = ORIENTED_EDGE ( 'NONE', *, *, #5617, .F. ) ;
#38269 = CARTESIAN_POINT ( 'NONE',  ( -35.15805814088607661, -13.30077706419156414, -6.711668136891848491 ) ) ;
#38270 = CARTESIAN_POINT ( 'NONE',  ( -12.65038256605562772, -23.99880442748382947, -13.56128062147820579 ) ) ;
#38271 = CARTESIAN_POINT ( 'NONE',  ( -4.100643064501314328, 15.70406341247269211, 13.00000000000000178 ) ) ;
#38272 = CARTESIAN_POINT ( 'NONE',  ( 16.40281439508208194, 21.37890742408058031, -10.26485299642392945 ) ) ;
#38273 = ORIENTED_EDGE ( 'NONE', *, *, #5642, .F. ) ;
#38274 = CARTESIAN_POINT ( 'NONE',  ( 20.30148177599484427, 3.803005773571547454, -27.60600077430455102 ) ) ;
#38275 = CARTESIAN_POINT ( 'NONE',  ( 13.30736835491658887, 15.59574623945385596, 10.49999999999999822 ) ) ;
#38276 = CARTESIAN_POINT ( 'NONE',  ( -22.38472516250435973, -15.35952186208485593, 23.00000000000000000 ) ) ;
#38277 = VECTOR ( 'NONE', #9519, 1000.000000000000114 ) ;
#38278 = ORIENTED_EDGE ( 'NONE', *, *, #12384, .F. ) ;
#38279 = CARTESIAN_POINT ( 'NONE',  ( -29.04989216121797213, -0.08486885121559410716, -11.58176799329598516 ) ) ;
#38280 = CARTESIAN_POINT ( 'NONE',  ( 24.14174240845033026, 0.003122030948076066903, -19.43079603134119893 ) ) ;
#38281 = CARTESIAN_POINT ( 'NONE',  ( 21.56512766274792625, -22.66165129494964958, 19.66345542862529072 ) ) ;
#38282 = EDGE_LOOP ( 'NONE', ( #37851, #33154, #23958, #25605 ) ) ;
#38283 = CARTESIAN_POINT ( 'NONE',  ( 4.336808689942017736E-15, 40.84107189184581443, -5.000000000000008882 ) ) ;
#38284 = DIRECTION ( 'NONE',  ( 0.9510565162951504226, -0.3090169943749573322, -0.000000000000000000 ) ) ;
#38285 = CARTESIAN_POINT ( 'NONE',  ( -8.339609403135952448, 11.87216320208451314, 9.500000000000000000 ) ) ;
#38286 = EDGE_CURVE ( 'NONE', #32239, #36997, #28639, .T. ) ;
#38287 = LINE ( 'NONE', #30105, #18475 ) ;
#38288 = FACE_OUTER_BOUND ( 'NONE', #32284, .T. ) ;
#38289 = DIRECTION ( 'NONE',  ( 0.4731467892558158250, -0.5254827454987615054, 0.7071067811865450192 ) ) ;
#38290 = FACE_OUTER_BOUND ( 'NONE', #27480, .T. ) ;
#38291 = EDGE_LOOP ( 'NONE', ( #3876, #2250, #28065, #33352 ) ) ;
#38292 = CARTESIAN_POINT ( 'NONE',  ( -6.643188263509865799, 35.96180620077112167, 10.49999999999999822 ) ) ;
#38293 = FACE_OUTER_BOUND ( 'NONE', #8799, .T. ) ;
#38294 = CARTESIAN_POINT ( 'NONE',  ( 27.36121244743086578, -25.22392150776288133, -5.440726707707272958 ) ) ;
#38295 = AXIS2_PLACEMENT_3D ( 'NONE', #18218, #2768, #15161 ) ;
#38296 = DIRECTION ( 'NONE',  ( -0.9135454576426059736, -0.4067366430757888285, 0.000000000000000000 ) ) ;
#38297 = CARTESIAN_POINT ( 'NONE',  ( -12.30736835487443415, 14.81698729810790560, 11.00000000000000000 ) ) ;
#38298 = CARTESIAN_POINT ( 'NONE',  ( 10.55968626961773360, 17.57118088696260827, -30.00000000000000355 ) ) ;
#38299 = PLANE ( 'NONE',  #18500 ) ;
#38300 = VERTEX_POINT ( 'NONE', #18494 ) ;
#38301 = CARTESIAN_POINT ( 'NONE',  ( -14.46390983480181092, 16.02145941329244394, -23.10970177944547643 ) ) ;
#38302 = CYLINDRICAL_SURFACE ( 'NONE', #28958, 1.000000000000000000 ) ;
#38303 = EDGE_CURVE ( 'NONE', #27240, #2755, #18300, .T. ) ;
#38304 = CARTESIAN_POINT ( 'NONE',  ( 11.17102189095818687, -20.47090416160008886, -20.54315939279690895 ) ) ;
#38305 = LINE ( 'NONE', #13313, #343 ) ;
#38306 = CARTESIAN_POINT ( 'NONE',  ( 15.40963821861455862, 26.71342488439698570, -5.946084157768660283 ) ) ;
#38307 = VERTEX_POINT ( 'NONE', #27232 ) ;
#38308 = CARTESIAN_POINT ( 'NONE',  ( 15.01833821314314044, 25.96818848446413952, -9.238322678839537616 ) ) ;
#38309 = VERTEX_POINT ( 'NONE', #7280 ) ;
#38311 = FACE_OUTER_BOUND ( 'NONE', #12603, .T. ) ;
#38310 = CARTESIAN_POINT ( 'NONE',  ( -14.98463571429964780, 26.07793220091295083, -9.232870696221679552 ) ) ;
#38312 = CARTESIAN_POINT ( 'NONE',  ( -9.667542991474126879, -18.45194233073163659, -26.83237868059747555 ) ) ;
#38313 = CARTESIAN_POINT ( 'NONE',  ( -33.43067318719309355, -0.2406684815417533818, 13.32518128616583475 ) ) ;
#38314 = CARTESIAN_POINT ( 'NONE',  ( -32.98459937871956527, -19.91850110786283423, -4.999999999999999112 ) ) ;
#38315 = CARTESIAN_POINT ( 'NONE',  ( -4.727592086853887210, -24.67674636019700785, -8.392755456812066583 ) ) ;
#38316 = CARTESIAN_POINT ( 'NONE',  ( 15.37979459131270588, 24.85259051631702221, -9.252807986672786811 ) ) ;
#38317 = ADVANCED_FACE ( 'NONE', ( #34332 ), #22164, .T. ) ;
#38318 = ORIENTED_EDGE ( 'NONE', *, *, #20464, .F. ) ;
#38319 = CARTESIAN_POINT ( 'NONE',  ( 19.30637010739042125, 7.335522903491736635, -27.14430384761622861 ) ) ;
#38320 = AXIS2_PLACEMENT_3D ( 'NONE', #38087, #35453, #20218 ) ;
#38321 = CARTESIAN_POINT ( 'NONE',  ( 9.441034666242805073, 32.57396620494213124, 7.000000000000000000 ) ) ;
#38322 = CARTESIAN_POINT ( 'NONE',  ( -2.510240365544621266, -24.77672057674680772, -5.000000000000000888 ) ) ;
#38323 = ADVANCED_FACE ( 'NONE', ( #28827 ), #37375, .T. ) ;
#38324 = CARTESIAN_POINT ( 'NONE',  ( 13.80282919548806575, 29.83094698618029028, 16.87380292611440424 ) ) ;
#38325 = ORIENTED_EDGE ( 'NONE', *, *, #15074, .F. ) ;
#38326 = CARTESIAN_POINT ( 'NONE',  ( -29.26784074738422703, -2.117567468756759830, -13.29754803565872123 ) ) ;
#38327 = CARTESIAN_POINT ( 'NONE',  ( -18.74997338764005050, -3.362744936731938417, 20.99999999999999645 ) ) ;
#38328 = ORIENTED_EDGE ( 'NONE', *, *, #34976, .F. ) ;
#38329 = CARTESIAN_POINT ( 'NONE',  ( 4.348106467989403257, 35.16482219193073178, 12.00000000000000000 ) ) ;
#38330 = CYLINDRICAL_SURFACE ( 'NONE', #32979, 0.4999999999999999445 ) ;
#38331 = VECTOR ( 'NONE', #6902, 1000.000000000000000 ) ;
#38332 = CARTESIAN_POINT ( 'NONE',  ( 31.06344462049394295, -14.71666030541080161, -11.98151952013437693 ) ) ;
#38333 = CARTESIAN_POINT ( 'NONE',  ( 20.78821643698954347, -29.20280246618839115, 11.55979286843934872 ) ) ;
#38334 = EDGE_CURVE ( 'NONE', #30382, #26791, #17648, .T. ) ;
#38335 = VERTEX_POINT ( 'NONE', #34929 ) ;
#38336 = EDGE_CURVE ( 'NONE', #36223, #30328, #19279, .T. ) ;
#38337 = DIRECTION ( 'NONE',  ( 0.000000000000000000, 0.000000000000000000, 1.000000000000000000 ) ) ;
#38338 = FACE_OUTER_BOUND ( 'NONE', #11682, .T. ) ;
#38339 = CARTESIAN_POINT ( 'NONE',  ( -1.653273178848927853E-15, 36.00000000000000711, 7.000000000000000000 ) ) ;
#38340 = EDGE_LOOP ( 'NONE', ( #3582, #27177, #30998, #36952 ) ) ;
#38341 = CARTESIAN_POINT ( 'NONE',  ( -1.842295339504430807, 36.47303149705159342, -9.727466432712501998 ) ) ;
#38342 = AXIS2_PLACEMENT_3D ( 'NONE', #22589, #31740, #18949 ) ;
#38343 = CARTESIAN_POINT ( 'NONE',  ( -14.99905852611806445, 22.33194247983213643, 7.000000000000000000 ) ) ;
#38344 = CARTESIAN_POINT ( 'NONE',  ( 10.44103466624280685, 32.57396620494213124, 7.000000000000000000 ) ) ;
#38345 = CARTESIAN_POINT ( 'NONE',  ( -22.84654430795398028, 26.73830628268968823, 10.00000000000000000 ) ) ;
#38346 = DIRECTION ( 'NONE',  ( 1.000000000000000000, 0.000000000000000000, 0.000000000000000000 ) ) ;
#38347 = CARTESIAN_POINT ( 'NONE',  ( 7.713869163865849643, 10.18146832927074996, 7.500000000000000888 ) ) ;
#38348 = CARTESIAN_POINT ( 'NONE',  ( 12.48692422165860094, 25.74591318921861927, -14.24962641246380457 ) ) ;
#38349 = DIRECTION ( 'NONE',  ( 1.000000000000000000, 0.000000000000000000, 0.000000000000000000 ) ) ;
#38350 = ORIENTED_EDGE ( 'NONE', *, *, #38920, .T. ) ;
#38352 = DIRECTION ( 'NONE',  ( 1.000000000000000000, 0.000000000000000000, 0.000000000000000000 ) ) ;
#38351 = CARTESIAN_POINT ( 'NONE',  ( -19.60099714212322297, 15.55874775609486882, -7.421013871162296383 ) ) ;
#38353 = CARTESIAN_POINT ( 'NONE',  ( -0.4999999999999998890, 37.04625217320466390, 10.99999999999999645 ) ) ;
#38354 = CARTESIAN_POINT ( 'NONE',  ( 9.825092482715485076, -18.54622831478960165, -26.22104406996453108 ) ) ;
#38355 = DIRECTION ( 'NONE',  ( -0.5000000000000039968, -0.8660254037844363761, 0.000000000000000000 ) ) ;
#38356 = VECTOR ( 'NONE', #25348, 1000.000000000000000 ) ;
#38357 = CARTESIAN_POINT ( 'NONE',  ( 15.08290252549542920, 26.19981407040120658, -8.764898325908280441 ) ) ;
#38358 = CARTESIAN_POINT ( 'NONE',  ( -22.40982762235196191, 2.618079236897031148, -29.99999999999999645 ) ) ;
#38359 = EDGE_CURVE ( 'NONE', #10298, #333, #15675, .T. ) ;
#38360 = CARTESIAN_POINT ( 'NONE',  ( -23.05386822411323422, -7.747535282638357224, 23.00000000000000000 ) ) ;
#38361 = CARTESIAN_POINT ( 'NONE',  ( -25.88768482325948028, -24.33645162349362678, -9.343698090164346937 ) ) ;
#38362 = CARTESIAN_POINT ( 'NONE',  ( 7.456069066676004553, -20.04449398788877090, -24.14870290390329188 ) ) ;
#38363 = CARTESIAN_POINT ( 'NONE',  ( 11.78620804298909519, 18.81532866151945171, -22.75140267569650021 ) ) ;
#38364 = CARTESIAN_POINT ( 'NONE',  ( 16.93799999173078419, 12.15640281848874871, -25.49561531272128789 ) ) ;
#38365 = FACE_OUTER_BOUND ( 'NONE', #5946, .T. ) ;
#38366 = CARTESIAN_POINT ( 'NONE',  ( 13.97557076678965693, 21.53386246193694475, 9.500000000000000000 ) ) ;
#38367 = ORIENTED_EDGE ( 'NONE', *, *, #34725, .F. ) ;
#38368 = CARTESIAN_POINT ( 'NONE',  ( -8.386326804491467612, 35.75291558016277094, -7.156120314017831774 ) ) ;
#38369 = ORIENTED_EDGE ( 'NONE', *, *, #19282, .F. ) ;
#38370 = CARTESIAN_POINT ( 'NONE',  ( -14.59943873959954352, -25.62395699127592508, -10.18321298866148972 ) ) ;
#38371 = AXIS2_PLACEMENT_3D ( 'NONE', #18717, #37396, #28448 ) ;
#38372 = DIRECTION ( 'NONE',  ( 1.000000000000000000, 0.000000000000000000, 0.000000000000000000 ) ) ;
#38373 = EDGE_LOOP ( 'NONE', ( #28085, #31316, #28632, #31230, #26103 ) ) ;
#38374 = CARTESIAN_POINT ( 'NONE',  ( 22.22387256208718043, 0.6525034796978533835, -22.73371951963157400 ) ) ;
#38375 = CIRCLE ( 'NONE', #27989, 0.9999999999999991118 ) ;
#38376 = CARTESIAN_POINT ( 'NONE',  ( -8.843266739736657556, 16.81698729810786830, 10.00000000000000000 ) ) ;
#38377 = FACE_OUTER_BOUND ( 'NONE', #9354, .T. ) ;
#38378 = ORIENTED_EDGE ( 'NONE', *, *, #662, .F. ) ;
#38379 = CARTESIAN_POINT ( 'NONE',  ( -25.16170031353656356, 0.4714222071989471741, -17.44778650913232099 ) ) ;
#38380 = ORIENTED_EDGE ( 'NONE', *, *, #35406, .F. ) ;
#38381 = CARTESIAN_POINT ( 'NONE',  ( 23.39873936915197916, -6.309811595435544263, -20.90194788542293125 ) ) ;
#38382 = EDGE_LOOP ( 'NONE', ( #19227, #5155, #4569, #36422 ) ) ;
#38383 = DIRECTION ( 'NONE',  ( 0.000000000000000000, 0.000000000000000000, 1.000000000000000000 ) ) ;
#38384 = VECTOR ( 'NONE', #17051, 1000.000000000000000 ) ;
#38385 = CARTESIAN_POINT ( 'NONE',  ( 15.98959510862164457, 30.99271259066415496, 10.99999999999987566 ) ) ;
#38386 = EDGE_CURVE ( 'NONE', #22563, #28022, #35126, .T. ) ;
#38387 = CARTESIAN_POINT ( 'NONE',  ( 5.440829913680675034, 10.60893893836775348, 12.00000000000000000 ) ) ;
#38388 = DIRECTION ( 'NONE',  ( -0.4067366430758009299, -0.9135454576426005335, -0.000000000000000000 ) ) ;
#38389 = CARTESIAN_POINT ( 'NONE',  ( 11.88159808435121789, 30.55960002361340955, 17.92354375535251165 ) ) ;
#38390 = DIRECTION ( 'NONE',  ( 0.000000000000000000, 0.000000000000000000, -1.000000000000000000 ) ) ;
#38391 = ORIENTED_EDGE ( 'NONE', *, *, #21800, .F. ) ;
#38392 =( NAMED_UNIT ( * ) PLANE_ANGLE_UNIT ( ) SI_UNIT ( $, .RADIAN. ) );
#38393 = CARTESIAN_POINT ( 'NONE',  ( 2.853166178176219425, 23.42705098312512746, 13.00000000000000178 ) ) ;
#38394 = DIRECTION ( 'NONE',  ( 1.000000000000000000, 0.000000000000000000, 0.000000000000000000 ) ) ;
#38395 = CARTESIAN_POINT ( 'NONE',  ( -9.356056665764020508, 26.06569820189714903, 10.00000000000000000 ) ) ;
#38396 = CARTESIAN_POINT ( 'NONE',  ( 19.03553521139049209, 16.91159591655264904, -6.445528870334666927 ) ) ;
#38397 = CARTESIAN_POINT ( 'NONE',  ( 10.34309936930504925, 32.23458342254649978, -10.30124509090378915 ) ) ;
#38398 = ORIENTED_EDGE ( 'NONE', *, *, #15466, .F. ) ;
#38399 = FACE_OUTER_BOUND ( 'NONE', #35624, .T. ) ;
#38400 = CARTESIAN_POINT ( 'NONE',  ( -0.9461134518049056918, 37.26099332938166242, 10.49999999999999822 ) ) ;
#38401 = CARTESIAN_POINT ( 'NONE',  ( 9.937768194491171769, -17.93102150851172993, -29.33920091550964671 ) ) ;
#38402 = CARTESIAN_POINT ( 'NONE',  ( 2.109373541296217347, 27.06550157850341876, 20.99999999999999645 ) ) ;
#38403 = LINE ( 'NONE', #32726, #17928 ) ;
#38404 = ADVANCED_FACE ( 'NONE', ( #25573 ), #18925, .T. ) ;
#38405 = ORIENTED_EDGE ( 'NONE', *, *, #13311, .F. ) ;
#38406 = CARTESIAN_POINT ( 'NONE',  ( -11.19011939127313049, 17.75217256258857645, -26.22551013601530912 ) ) ;
#38407 = CARTESIAN_POINT ( 'NONE',  ( -25.67968615518532971, -26.00921032235747887, 16.30093088680191116 ) ) ;
#38408 = CARTESIAN_POINT ( 'NONE',  ( 11.48325201437814158, -21.51848809436486931, -18.49319478269642403 ) ) ;
#38409 = ADVANCED_FACE ( 'NONE', ( #19681 ), #24981, .T. ) ;
#38410 = AXIS2_PLACEMENT_3D ( 'NONE', #13540, #25928, #28981 ) ;
#38411 = EDGE_CURVE ( 'NONE', #9357, #18134, #15041, .T. ) ;
#38412 = FACE_OUTER_BOUND ( 'NONE', #37436, .T. ) ;
#38413 = VERTEX_POINT ( 'NONE', #31675 ) ;
#38414 = ORIENTED_EDGE ( 'NONE', *, *, #40194, .F. ) ;
#38415 = CARTESIAN_POINT ( 'NONE',  ( -9.138473067724239840, 20.98330350826042690, -22.34731987422578570 ) ) ;
#38416 = CARTESIAN_POINT ( 'NONE',  ( -5.724378136954611840, 12.76962061027129458, 6.000000000000000000 ) ) ;
#38417 = DIRECTION ( 'NONE',  ( 0.000000000000000000, 0.000000000000000000, 1.000000000000000000 ) ) ;
#38418 = EDGE_CURVE ( 'NONE', #22962, #12988, #37089, .T. ) ;
#38419 = AXIS2_PLACEMENT_3D ( 'NONE', #34819, #31774, #19992 ) ;
#38420 = CARTESIAN_POINT ( 'NONE',  ( -24.34759780290428566, -6.015430600026174801, -19.86655231846714287 ) ) ;
#38421 = DIRECTION ( 'NONE',  ( -0.6691306063588569053, 0.7431448254773954654, 0.000000000000000000 ) ) ;
#38422 = ORIENTED_EDGE ( 'NONE', *, *, #38231, .F. ) ;
#38423 = CARTESIAN_POINT ( 'NONE',  ( 23.27325054855478470, 0.6741572905409627392, -20.55679979627661425 ) ) ;
#38424 = CARTESIAN_POINT ( 'NONE',  ( 15.11440468493446687, 26.16449293604169668, -8.767649845972018241 ) ) ;
#38425 = CARTESIAN_POINT ( 'NONE',  ( -6.354454053420248272, 35.54304081427989814, 7.000000000000000000 ) ) ;
#38426 = UNCERTAINTY_MEASURE_WITH_UNIT (LENGTH_MEASURE( 1.000000000000000082E-05 ), #7912, 'distance_accuracy_value', 'NONE');
#38427 = VERTEX_POINT ( 'NONE', #16038 ) ;
#38428 = CARTESIAN_POINT ( 'NONE',  ( -29.36168537595271744, 0.06585758006631414752, -10.65324670958523967 ) ) ;
#38429 = CARTESIAN_POINT ( 'NONE',  ( -11.87435565298220652, 15.06698729810788961, 7.000000000000000000 ) ) ;
#38430 = EDGE_LOOP ( 'NONE', ( #24592, #32350, #6633, #33620, #39523 ) ) ;
#38431 = CARTESIAN_POINT ( 'NONE',  ( 20.88446507122673168, -1.639503378383732279, -26.63968719893129133 ) ) ;
#38432 = CARTESIAN_POINT ( 'NONE',  ( -2.525645716490710679, 8.212903943950959018, 7.000000000000000000 ) ) ;
#38433 = AXIS2_PLACEMENT_3D ( 'NONE', #11431, #7566, #4930 ) ;
#38434 = CARTESIAN_POINT ( 'NONE',  ( 31.51573171626510117, 0.5582143012859381859, 15.13084544680214094 ) ) ;
#38435 = ORIENTED_EDGE ( 'NONE', *, *, #15204, .F. ) ;
#38436 = CARTESIAN_POINT ( 'NONE',  ( -1.782755275186030275, 38.97445513318768207, 15.72805884748939143 ) ) ;
#38437 = EDGE_CURVE ( 'NONE', #27813, #708, #25409, .T. ) ;
#38438 = CARTESIAN_POINT ( 'NONE',  ( 5.218261001347106465, -24.78318996519343997, 16.30093088680190760 ) ) ;
#38439 = ADVANCED_FACE ( 'NONE', ( #4035 ), #6679, .T. ) ;
#38440 = CARTESIAN_POINT ( 'NONE',  ( 9.293999462566146619, 11.53598992149257008, 12.00000000000000000 ) ) ;
#38441 = ADVANCED_FACE ( 'NONE', ( #602 ), #25911, .T. ) ;
#38442 = CARTESIAN_POINT ( 'NONE',  ( 5.143257298371474384, 25.23120666211534413, 21.00000000000000355 ) ) ;
#38443 = CARTESIAN_POINT ( 'NONE',  ( 6.688300058587269170, 16.47782454277055564, 6.000000000000000000 ) ) ;
#38444 = AXIS2_PLACEMENT_3D ( 'NONE', #17313, #30295, #7747 ) ;
#38445 = CARTESIAN_POINT ( 'NONE',  ( -7.645071344821658954, 9.594463043616254794, 7.000000000000000000 ) ) ;
#38446 = LINE ( 'NONE', #23411, #28796 ) ;
#38447 = CARTESIAN_POINT ( 'NONE',  ( 19.27886458632777789, 17.11073565397641616, 15.72805884748938432 ) ) ;
#38448 = CARTESIAN_POINT ( 'NONE',  ( -19.30322778826291596, 7.114745259177782444, -28.27681454190587473 ) ) ;
#38449 = CARTESIAN_POINT ( 'NONE',  ( 21.77381489986708729, -26.82402092198213950, -7.223031671328368652 ) ) ;
#38450 = CARTESIAN_POINT ( 'NONE',  ( -11.11016527260153097, 31.83082137946489354, 11.00000000000000000 ) ) ;
#38451 = EDGE_CURVE ( 'NONE', #7627, #30348, #1206, .T. ) ;
#38452 = CARTESIAN_POINT ( 'NONE',  ( 10.98290474487089341, 17.71099146112738154, -26.81703527214839156 ) ) ;
#38453 = VERTEX_POINT ( 'NONE', #7891 ) ;
#38454 = CARTESIAN_POINT ( 'NONE',  ( -12.17818915529227475, 17.82757546800293724, -23.95589322833938084 ) ) ;
#38455 = CARTESIAN_POINT ( 'NONE',  ( -29.18141975161403678, -3.595827299476843208, 19.27171037444158230 ) ) ;
#38456 = EDGE_CURVE ( 'NONE', #32704, #35813, #28002, .T. ) ;
#38457 = FACE_OUTER_BOUND ( 'NONE', #26695, .T. ) ;
#38458 = CARTESIAN_POINT ( 'NONE',  ( 11.93447970895564936, 19.33730221226423396, -21.62440255458760774 ) ) ;
#38459 = EDGE_LOOP ( 'NONE', ( #3383, #15197 ) ) ;
#38460 = CARTESIAN_POINT ( 'NONE',  ( 33.12547343259578980, -19.59933603596603291, -5.855473759911283160 ) ) ;
#38461 = DIRECTION ( 'NONE',  ( 1.000000000000000000, 0.000000000000000000, 0.000000000000000000 ) ) ;
#38462 = ORIENTED_EDGE ( 'NONE', *, *, #14664, .F. ) ;
#38464 = FACE_OUTER_BOUND ( 'NONE', #24247, .T. ) ;
#38463 = CARTESIAN_POINT ( 'NONE',  ( -14.09052875053176024, 24.98470579825722027, -12.50744983255499676 ) ) ;
#38465 = CARTESIAN_POINT ( 'NONE',  ( -9.913802546424228979, -17.94660116923212456, -29.33974538417603384 ) ) ;
#38466 = CARTESIAN_POINT ( 'NONE',  ( 13.41748865645068811, 15.79359748466640667, 7.382773698552464126 ) ) ;
#38467 = CONICAL_SURFACE ( 'NONE', #30037, 1.000000000000002665, 0.7853981633974509435 ) ;
#38468 = ORIENTED_EDGE ( 'NONE', *, *, #9384, .F. ) ;
#38469 = CARTESIAN_POINT ( 'NONE',  ( -25.62699182077987814, -10.58736709928222197, -17.64213997670373146 ) ) ;
#38470 = CARTESIAN_POINT ( 'NONE',  ( -9.194505705513583038, -18.37015698959482890, -28.71945744372206022 ) ) ;
#38471 = DIRECTION ( 'NONE',  ( 0.000000000000000000, 0.000000000000000000, 1.000000000000000000 ) ) ;
#38472 = CARTESIAN_POINT ( 'NONE',  ( 16.90293753726015780, 20.49095762985944447, -9.799744462339120332 ) ) ;
#38473 = ORIENTED_EDGE ( 'NONE', *, *, #26393, .F. ) ;
#38474 = CARTESIAN_POINT ( 'NONE',  ( 27.37006007402764496, 2.900043331923816581, -9.768361963922430391 ) ) ;
#38475 = DIRECTION ( 'NONE',  ( 0.9135454576426005335, -0.4067366430758009299, 0.000000000000000000 ) ) ;
#38476 = AXIS2_PLACEMENT_3D ( 'NONE', #7369, #25658, #19981 ) ;
#38477 = CARTESIAN_POINT ( 'NONE',  ( -23.19735768193461567, -14.64350930037788068, 23.00000000000000000 ) ) ;
#38478 = ORIENTED_EDGE ( 'NONE', *, *, #31236, .F. ) ;
#38479 = CARTESIAN_POINT ( 'NONE',  ( -20.49112616741955506, 0.6095660351776280850, -29.34380360967770685 ) ) ;
#38480 = CARTESIAN_POINT ( 'NONE',  ( 30.22309925524323759, -0.6771996511655676843, -10.12731539925492541 ) ) ;
#38481 = CARTESIAN_POINT ( 'NONE',  ( 28.78203904708371397, -16.61731799165995227, 19.99202127657103389 ) ) ;
#38482 = VERTEX_POINT ( 'NONE', #10746 ) ;
#38483 = CARTESIAN_POINT ( 'NONE',  ( -28.28304003931276966, 1.770888965579145324, -9.744255481737679858 ) ) ;
#38484 = CARTESIAN_POINT ( 'NONE',  ( -23.06249103411543544, 13.31513540672989926, -13.39439507595155554 ) ) ;
#38485 = AXIS2_PLACEMENT_3D ( 'NONE', #25305, #22646, #22245 ) ;
#38486 = DIRECTION ( 'NONE',  ( 0.000000000000000000, 0.000000000000000000, 1.000000000000000000 ) ) ;
#38487 = DIRECTION ( 'NONE',  ( -1.000000000000000000, 0.000000000000000000, 0.000000000000000000 ) ) ;
#38488 = VECTOR ( 'NONE', #17011, 1000.000000000000000 ) ;
#38489 = CARTESIAN_POINT ( 'NONE',  ( -11.56190694343544045, 31.61076883254029113, 10.49999999999999822 ) ) ;
#38490 = DIRECTION ( 'NONE',  ( -0.000000000000000000, -0.000000000000000000, -1.000000000000000000 ) ) ;
#38491 = DIRECTION ( 'NONE',  ( -0.000000000000000000, 0.000000000000000000, -1.000000000000000000 ) ) ;
#38492 = ORIENTED_EDGE ( 'NONE', *, *, #2669, .T. ) ;
#38493 = CARTESIAN_POINT ( 'NONE',  ( -6.830039222088849726, 35.38192592444590900, 10.49999999999999822 ) ) ;
#38494 =( GEOMETRIC_REPRESENTATION_CONTEXT ( 3 ) GLOBAL_UNCERTAINTY_ASSIGNED_CONTEXT ( ( #7942 ) ) GLOBAL_UNIT_ASSIGNED_CONTEXT ( ( #36754, #17681, #30056 ) ) REPRESENTATION_CONTEXT ( 'NONE', 'WORKASPACE' ) );
#38495 = CARTESIAN_POINT ( 'NONE',  ( -0.3762682982559537037, 25.43444280220171194, 12.00000000000000000 ) ) ;
#38496 = CARTESIAN_POINT ( 'NONE',  ( 22.40086744732950308, -20.72561197270982447, -14.82888506793862859 ) ) ;
#38497 = CARTESIAN_POINT ( 'NONE',  ( 14.36830325120613239, 20.48707633493482660, 11.00000000000000000 ) ) ;
#38498 = CARTESIAN_POINT ( 'NONE',  ( -10.14717575287011542, 32.53695909538323860, 12.00000000000000000 ) ) ;
#38499 = CARTESIAN_POINT ( 'NONE',  ( 15.18041152575273500, 27.55477496851653640, -5.470520559687252593 ) ) ;
#38500 = DIRECTION ( 'NONE',  ( 0.7431448254773855844, -0.6691306063588678965, 0.000000000000000000 ) ) ;
#38501 = EDGE_LOOP ( 'NONE', ( #5962, #22094, #35683, #1620 ) ) ;
#38502 = AXIS2_PLACEMENT_3D ( 'NONE', #27395, #11368, #39786 ) ;
#38503 = CARTESIAN_POINT ( 'NONE',  ( -14.43025776552523709, 14.57938852240508965, -30.00000000000000711 ) ) ;
#38504 = CARTESIAN_POINT ( 'NONE',  ( -18.23649648353780961, -16.09146789626144169, 20.99999999999999645 ) ) ;
#38505 = CARTESIAN_POINT ( 'NONE',  ( 9.439680310844765998, -18.19733056428809803, -30.00000000000000000 ) ) ;
#38506 = DIRECTION ( 'NONE',  ( -0.000000000000000000, -0.000000000000000000, -1.000000000000000000 ) ) ;
#38507 = CARTESIAN_POINT ( 'NONE',  ( 11.19190749613552072, 17.75087991604564053, -26.22569030697802717 ) ) ;
#38508 = EDGE_LOOP ( 'NONE', ( #36192, #38025, #35160, #27187 ) ) ;
#38509 = CARTESIAN_POINT ( 'NONE',  ( 11.88987759224297669, 19.38458514940646893, -21.61667515872348133 ) ) ;
#38510 = ORIENTED_EDGE ( 'NONE', *, *, #21293, .F. ) ;
#38512 = CARTESIAN_POINT ( 'NONE',  ( 3.596545519285629933, 7.984450832230633566, 10.76099332938164288 ) ) ;
#38511 = CARTESIAN_POINT ( 'NONE',  ( -15.19914089571920890, 26.51953392815337196, -7.824019997130747583 ) ) ;
#38513 = CARTESIAN_POINT ( 'NONE',  ( -13.34033674645691647, -23.61967562324617731, -14.47800511745506213 ) ) ;
#38514 = CARTESIAN_POINT ( 'NONE',  ( -37.58754968649139983, -10.91577297561634552, 11.00000000000031797 ) ) ;
#38515 = CARTESIAN_POINT ( 'NONE',  ( -31.30459858316601185, -18.91178069307321152, -9.725088435557024624 ) ) ;
#38516 = VECTOR ( 'NONE', #21405, 1000.000000000000000 ) ;
#38517 = CARTESIAN_POINT ( 'NONE',  ( -7.194050238941392728, -21.51981635923818104, -19.89556854701389099 ) ) ;
#38518 = CARTESIAN_POINT ( 'NONE',  ( 13.13555678008467353, 20.35422080500006459, -18.53327313025195977 ) ) ;
#38519 = VERTEX_POINT ( 'NONE', #20096 ) ;
#38520 = CARTESIAN_POINT ( 'NONE',  ( 23.60508491000810594, 8.220972298804724687, -9.371835443833486323 ) ) ;
#38521 = DIRECTION ( 'NONE',  ( 0.000000000000000000, 0.000000000000000000, 1.000000000000000000 ) ) ;
#38522 = CARTESIAN_POINT ( 'NONE',  ( 12.74984837297361828, -26.03613044200378113, -5.000000000000000000 ) ) ;
#38523 = CARTESIAN_POINT ( 'NONE',  ( -7.775297188279279403, 35.41132985342461126, 17.42190598798310930 ) ) ;
#38524 = ORIENTED_EDGE ( 'NONE', *, *, #26265, .T. ) ;
#38525 = CARTESIAN_POINT ( 'NONE',  ( -26.24583311168948185, -1.798973365801582291, -17.17928807732686280 ) ) ;
#38526 = VECTOR ( 'NONE', #17435, 1000.000000000000114 ) ;
#38527 = CARTESIAN_POINT ( 'NONE',  ( -7.962467718763332591, 24.71319220550997642, 20.69868183039781329 ) ) ;
#38528 = VERTEX_POINT ( 'NONE', #23540 ) ;
#38529 = DIRECTION ( 'NONE',  ( -0.000000000000000000, -0.000000000000000000, -1.000000000000000000 ) ) ;
#38530 = DIRECTION ( 'NONE',  ( 0.000000000000000000, 0.000000000000000000, 1.000000000000000000 ) ) ;
#38531 = LINE ( 'NONE', #32655, #26810 ) ;
#38532 = CARTESIAN_POINT ( 'NONE',  ( 33.19857134126652909, -14.52248378749990820, -9.739578698604827167 ) ) ;
#38533 = CARTESIAN_POINT ( 'NONE',  ( 28.21696687770567280, -27.03935558029786534, 12.14047268033092841 ) ) ;
#38534 = AXIS2_PLACEMENT_3D ( 'NONE', #25938, #38337, #1775 ) ;
#38535 = EDGE_CURVE ( 'NONE', #26241, #37722, #10955, .T. ) ;
#38536 = VERTEX_POINT ( 'NONE', #7487 ) ;
#38537 = B_SPLINE_CURVE_WITH_KNOTS ( 'NONE', 3,
 ( #11927, #8879, #21268, #39553, #24511, #20879, #33281, #37109 ),
 .UNSPECIFIED., .F., .F.,
 ( 4, 2, 2, 4 ),
 ( 0.000000000000000000, 0.0004726692273637176397, 0.0007090038410455758904, 0.0009453384547274341953 ),
 .UNSPECIFIED. ) ;
#38538 = PLANE ( 'NONE',  #21003 ) ;
#38539 = CARTESIAN_POINT ( 'NONE',  ( -9.742785792574970571, -49.01344959084108410, 23.00000000000000000 ) ) ;
#38540 = CARTESIAN_POINT ( 'NONE',  ( 9.697889840765411051, 31.90483559858327212, 10.50000000000000000 ) ) ;
#38541 = ORIENTED_EDGE ( 'NONE', *, *, #28985, .T. ) ;
#38542 = AXIS2_PLACEMENT_3D ( 'NONE', #18128, #11627, #24407 ) ;
#38543 = ADVANCED_FACE ( 'NONE', ( #26782 ), #23737, .T. ) ;
#38544 = CARTESIAN_POINT ( 'NONE',  ( -0.7332251858107181608, 37.19956836493663843, -8.842669820069614772 ) ) ;
#38545 = CARTESIAN_POINT ( 'NONE',  ( -3.229437847141423124, 24.50739181907689712, 13.00000000000000178 ) ) ;
#38546 = DIRECTION ( 'NONE',  ( -0.9510565162951497564, 0.3090169943749591086, 3.469446951953608667E-15 ) ) ;
#38547 = ADVANCED_FACE ( 'NONE', ( #32897 ), #1810, .T. ) ;
#38548 = CARTESIAN_POINT ( 'NONE',  ( 14.49025312501839657, 21.64735187953116480, 10.83333333333333393 ) ) ;
#38549 = LINE ( 'NONE', #7057, #6742 ) ;
#38550 = DIRECTION ( 'NONE',  ( 0.000000000000000000, 0.000000000000000000, 1.000000000000000000 ) ) ;
#38551 = CARTESIAN_POINT ( 'NONE',  ( 11.54610483293918755, 23.61922780243806486, -17.18207871116365837 ) ) ;
#38552 = CARTESIAN_POINT ( 'NONE',  ( -4.940908595777636414, 35.94977745735568675, 11.00000000000000000 ) ) ;
#38553 = ORIENTED_EDGE ( 'NONE', *, *, #40144, .F. ) ;
#38555 = CARTESIAN_POINT ( 'NONE',  ( 19.73557158514996601, 33.31698729810761250, 11.00000000000000000 ) ) ;
#38554 = CARTESIAN_POINT ( 'NONE',  ( -19.24418432356083386, 12.60524799736691115, -15.94388489509767837 ) ) ;
#38556 = CARTESIAN_POINT ( 'NONE',  ( -0.4999999999999998890, 37.18846563620834189, 10.96580507645519909 ) ) ;
#38557 = CARTESIAN_POINT ( 'NONE',  ( 14.06819841691203266, -24.61544153353286646, -12.54891093376155986 ) ) ;
#38558 = CARTESIAN_POINT ( 'NONE',  ( 13.94482798346721175, 26.50521816028912525, 11.00000000000000000 ) ) ;
#38559 = CARTESIAN_POINT ( 'NONE',  ( 14.72345531851253853, 25.43898799495751106, -10.65037270653031598 ) ) ;
#38560 = CARTESIAN_POINT ( 'NONE',  ( -6.155076441694329326, 21.71698211341365692, -29.99999999999997868 ) ) ;
#38561 = CARTESIAN_POINT ( 'NONE',  ( -18.23649648353780961, -16.09146789626143814, 23.00000000000000000 ) ) ;
#38562 = CIRCLE ( 'NONE', #37289, 18.00000000000000355 ) ;
#38563 = CARTESIAN_POINT ( 'NONE',  ( -26.29711927695796092, -24.70225483488810170, -8.459928924156699281 ) ) ;
#38564 = CARTESIAN_POINT ( 'NONE',  ( 8.347004892849424706, -25.02468466642049449, -8.361640715383630962 ) ) ;
#38565 = CARTESIAN_POINT ( 'NONE',  ( 11.14613432397584880, 17.25733169733589989, -28.71274769282841888 ) ) ;
#38566 = CARTESIAN_POINT ( 'NONE',  ( 17.21149163973099760, 11.38646518709530220, -27.17255296939820752 ) ) ;
#38567 = EDGE_CURVE ( 'NONE', #1690, #17473, #12455, .T. ) ;
#38568 = DIRECTION ( 'NONE',  ( 0.000000000000000000, 0.000000000000000000, 1.000000000000000000 ) ) ;
#38569 = CARTESIAN_POINT ( 'NONE',  ( 12.80736835487433112, 15.68301270189216545, 9.500000000000000000 ) ) ;
#38570 = EDGE_CURVE ( 'NONE', #29211, #1824, #35935, .T. ) ;
#38571 = ORIENTED_EDGE ( 'NONE', *, *, #25247, .T. ) ;
#38572 = CARTESIAN_POINT ( 'NONE',  ( -7.326431115582969333, 35.94962014070476641, -8.009053875344944728 ) ) ;
#38573 = ORIENTED_EDGE ( 'NONE', *, *, #36979, .F. ) ;
#38574 = CARTESIAN_POINT ( 'NONE',  ( -15.09037123163817640, -26.35566568629046103, -7.828641914250869860 ) ) ;
#38575 = CARTESIAN_POINT ( 'NONE',  ( 14.57109471128388378, 21.97402451295022630, 10.49999999999999822 ) ) ;
#38576 = EDGE_LOOP ( 'NONE', ( #4505, #35835 ) ) ;
#38577 = DIRECTION ( 'NONE',  ( -0.2079116908177533751, 0.9781476007338067991, 0.000000000000000000 ) ) ;
#38578 = CARTESIAN_POINT ( 'NONE',  ( 10.70158575030369796, 30.79011836036717753, 10.50000000000000000 ) ) ;
#38579 = ORIENTED_EDGE ( 'NONE', *, *, #35196, .F. ) ;
#38580 = CARTESIAN_POINT ( 'NONE',  ( -20.80888993467136316, 0.9087143968972012376, -26.83659548020632002 ) ) ;
#38581 = ORIENTED_EDGE ( 'NONE', *, *, #30613, .T. ) ;
#38582 = CARTESIAN_POINT ( 'NONE',  ( 34.50741919436119787, -9.298902886619249131, -8.474956792276689299 ) ) ;
#38583 = CIRCLE ( 'NONE', #33417, 1.000000000000000000 ) ;
#38584 = VERTEX_POINT ( 'NONE', #35328 ) ;
#38585 = CARTESIAN_POINT ( 'NONE',  ( -12.44178368932704259, 35.65276919562052882, 11.00000000000005329 ) ) ;
#38586 = DIRECTION ( 'NONE',  ( 1.000000000000000000, 0.000000000000000000, 0.000000000000000000 ) ) ;
#38587 = AXIS2_PLACEMENT_3D ( 'NONE', #28555, #37703, #728 ) ;
#38588 = DIRECTION ( 'NONE',  ( -1.000000000000000000, 0.000000000000000000, 0.000000000000000000 ) ) ;
#38589 = EDGE_CURVE ( 'NONE', #25338, #20584, #8569, .T. ) ;
#38590 = CARTESIAN_POINT ( 'NONE',  ( 7.124477683919607784, 34.33078274761139426, 18.42518152272109333 ) ) ;
#38591 = CIRCLE ( 'NONE', #35377, 1.000000000000000888 ) ;
#38592 = DIRECTION ( 'NONE',  ( 0.1470157664651866314, 0.6916548014802309519, -0.7071067811865446862 ) ) ;
#38593 = ORIENTED_EDGE ( 'NONE', *, *, #8773, .T. ) ;
#38594 = DIRECTION ( 'NONE',  ( 0.000000000000000000, 0.000000000000000000, 1.000000000000000000 ) ) ;
#38595 = CARTESIAN_POINT ( 'NONE',  ( -2.618397918552020975, 7.776539141412908585, 10.76099332938163755 ) ) ;
#38596 = CARTESIAN_POINT ( 'NONE',  ( -0.6237384431625470071, 19.56555719779890978, 12.00000000000000000 ) ) ;
#38597 = CARTESIAN_POINT ( 'NONE',  ( 15.53294352554807034, 13.99868018475545561, -25.43220508911406341 ) ) ;
#38598 = CARTESIAN_POINT ( 'NONE',  ( 6.888886835531742747, 21.38082869974457623, -23.27631121293514838 ) ) ;
#38599 = ORIENTED_EDGE ( 'NONE', *, *, #20583, .T. ) ;
#38600 = CARTESIAN_POINT ( 'NONE',  ( -5.440836655099179353, 34.39106106163288246, 12.00000000000000000 ) ) ;
#38601 = DIRECTION ( 'NONE',  ( 1.000000000000000000, 0.000000000000000000, 0.000000000000000000 ) ) ;
#38602 = CARTESIAN_POINT ( 'NONE',  ( 10.11113855348066615, -17.88931650804065754, -28.68331442007524856 ) ) ;
#38603 = DIRECTION ( 'NONE',  ( -1.000000000000000000, 0.000000000000000000, 0.000000000000000000 ) ) ;
#38604 = CARTESIAN_POINT ( 'NONE',  ( -3.494943660522439099, 10.76222879119470832, 6.000000000000000000 ) ) ;
#38605 = AXIS2_PLACEMENT_3D ( 'NONE', #32479, #26573, #4432 ) ;
#38606 = ORIENTED_EDGE ( 'NONE', *, *, #30545, .T. ) ;
#38607 = CARTESIAN_POINT ( 'NONE',  ( -11.06212937511586958, 17.50982107800345133, -27.44695155360371075 ) ) ;
#38608 = CARTESIAN_POINT ( 'NONE',  ( -35.51887168741988887, -12.71114019210525647, 16.30093088680185076 ) ) ;
#38609 = CARTESIAN_POINT ( 'NONE',  ( 14.79195119394937308, -26.44684019677998421, -6.889201696584072110 ) ) ;
#38610 = ADVANCED_FACE ( 'NONE', ( #26379 ), #20500, .F. ) ;
#38611 = DIRECTION ( 'NONE',  ( 1.000000000000000000, 0.000000000000000000, 0.000000000000000000 ) ) ;
#38612 = EDGE_CURVE ( 'NONE', #6323, #1436, #38630, .T. ) ;
#38613 = EDGE_LOOP ( 'NONE', ( #28079, #6513, #31836, #33024 ) ) ;
#38614 = ORIENTED_EDGE ( 'NONE', *, *, #21652, .T. ) ;
#38615 = CARTESIAN_POINT ( 'NONE',  ( -11.87470576980882697, 27.72462808436429071, -13.19994123200545744 ) ) ;
#38616 = AXIS2_PLACEMENT_3D ( 'NONE', #34864, #16782, #29168 ) ;
#38617 = CARTESIAN_POINT ( 'NONE',  ( 6.577540944421576441, 33.15743037285414374, 12.00000000000000000 ) ) ;
#38618 = FACE_BOUND ( 'NONE', #31478, .T. ) ;
#38619 = AXIS2_PLACEMENT_3D ( 'NONE', #33319, #17878, #30261 ) ;
#38621 = AXIS2_PLACEMENT_3D ( 'NONE', #35981, #11989, #24381 ) ;
#38620 = CARTESIAN_POINT ( 'NONE',  ( -26.22468522521110046, -6.472231845536984274, -17.80872549056464749 ) ) ;
#38622 = DIRECTION ( 'NONE',  ( 1.000000000000000000, 0.000000000000000000, 0.000000000000000000 ) ) ;
#38623 = VERTEX_POINT ( 'NONE', #17663 ) ;
#38624 = CARTESIAN_POINT ( 'NONE',  ( 21.25435618972812790, 0.9309806893528798089, -25.03105100026559171 ) ) ;
#38625 = CARTESIAN_POINT ( 'NONE',  ( -10.10646936306323340, 32.94553861768096681, 10.49999999999999822 ) ) ;
#38626 = CARTESIAN_POINT ( 'NONE',  ( -8.927394655428429360, 11.06314620770957013, 11.00000000000000000 ) ) ;
#38627 = LINE ( 'NONE', #13032, #35520 ) ;
#38628 = ORIENTED_EDGE ( 'NONE', *, *, #11364, .F. ) ;
#38629 = CARTESIAN_POINT ( 'NONE',  ( -26.50930299955345504, 0.2689666410773219885, -15.44989252601773266 ) ) ;
#38630 = B_SPLINE_CURVE_WITH_KNOTS ( 'NONE', 3,
 ( #10544, #39175, #11354, #36137, #20704, #4847, #35533, #5251 ),
 .UNSPECIFIED., .F., .F.,
 ( 4, 2, 2, 4 ),
 ( 8.673617379884035472E-19, 0.0004726692273637259339, 0.0007090038410455884671, 0.0009453384547274510004 ),
 .UNSPECIFIED. ) ;
#38631 = CARTESIAN_POINT ( 'NONE',  ( 0.6237317017440463518, 25.43444280220171194, 12.00000000000000000 ) ) ;
#38632 = ORIENTED_EDGE ( 'NONE', *, *, #7249, .T. ) ;
#38633 = CARTESIAN_POINT ( 'NONE',  ( 28.04465044637506921, -2.531702322499061353, -15.16146178204541073 ) ) ;
#38634 = CARTESIAN_POINT ( 'NONE',  ( -5.947717410344457001, 34.62949535663729250, 10.00000000000000000 ) ) ;
#38635 = CARTESIAN_POINT ( 'NONE',  ( 22.52482594781217529, -27.93079697604290246, 15.13084544680195265 ) ) ;
#38636 = ORIENTED_EDGE ( 'NONE', *, *, #21322, .T. ) ;
#38637 = CARTESIAN_POINT ( 'NONE',  ( -15.87271491999997863, 26.91186955879525300, 15.72805884748939498 ) ) ;
#38638 = CARTESIAN_POINT ( 'NONE',  ( -10.71169154829944681, -23.81371503818770918, 17.92354375535594357 ) ) ;
#38639 = CARTESIAN_POINT ( 'NONE',  ( 2.036571916123615100, 8.108948098542045457, 7.499999999999990230 ) ) ;
#38640 = EDGE_CURVE ( 'NONE', #22764, #2610, #28691, .T. ) ;
#38641 = CARTESIAN_POINT ( 'NONE',  ( 7.722840163546785597, 25.57530741998005652, 20.69868183039857712 ) ) ;
#38642 = DIRECTION ( 'NONE',  ( -0.8090169943749426773, 0.5877852522924797984, 0.000000000000000000 ) ) ;
#38643 = ORIENTED_EDGE ( 'NONE', *, *, #30284, .F. ) ;
#38644 = ADVANCED_FACE ( 'NONE', ( #13584 ), #25971, .T. ) ;
#38645 = DIRECTION ( 'NONE',  ( -0.000000000000000000, -0.000000000000000000, -1.000000000000000000 ) ) ;
#38646 = CIRCLE ( 'NONE', #16610, 17.00000000000000355 ) ;
#38647 = CARTESIAN_POINT ( 'NONE',  ( 4.861068763497363499, 36.44255459974750266, -8.860485891349553000 ) ) ;
#38648 = AXIS2_PLACEMENT_3D ( 'NONE', #7115, #13620, #1435 ) ;
#38649 = CARTESIAN_POINT ( 'NONE',  ( 9.593820794837855104, 26.14295245049076755, 10.75000000000000000 ) ) ;
#38650 = CARTESIAN_POINT ( 'NONE',  ( 25.97912795563643584, 2.630260520701592775, 17.92354375536424627 ) ) ;
#38651 = CARTESIAN_POINT ( 'NONE',  ( -20.92786251698451494, 10.22285104615988693, -14.91617428519021082 ) ) ;
#38652 = CARTESIAN_POINT ( 'NONE',  ( 21.40359050063177904, -26.41076042838597004, -8.557087298424924882 ) ) ;
#38653 = LINE ( 'NONE', #34060, #273 ) ;
#38654 = DIRECTION ( 'NONE',  ( 0.000000000000000000, 0.000000000000000000, 1.000000000000000000 ) ) ;
#38655 = ORIENTED_EDGE ( 'NONE', *, *, #23441, .T. ) ;
#38656 = CARTESIAN_POINT ( 'NONE',  ( 15.38842093998857230, 26.88136989284191003, -5.473725555427078504 ) ) ;
#38657 = ORIENTED_EDGE ( 'NONE', *, *, #34640, .T. ) ;
#38658 = CARTESIAN_POINT ( 'NONE',  ( -15.63977754581427959, 25.75093463275924677, -6.418238443301547136 ) ) ;
#38659 = CARTESIAN_POINT ( 'NONE',  ( -29.31961554340469078, -5.098421488388908074, 19.66345542862496742 ) ) ;
#38660 = LINE ( 'NONE', #29519, #2322 ) ;
#38661 = CARTESIAN_POINT ( 'NONE',  ( 15.26439360241955612, 26.29740473991443039, -7.828362627414925612 ) ) ;
#38662 = ORIENTED_EDGE ( 'NONE', *, *, #22388, .F. ) ;
#38663 = CARTESIAN_POINT ( 'NONE',  ( 30.18950977129052049, -16.64208564415852365, -11.97445339315004809 ) ) ;
#38664 = EDGE_LOOP ( 'NONE', ( #19159, #10913, #24258, #27870 ) ) ;
#38666 = CARTESIAN_POINT ( 'NONE',  ( -2.525645716490712012, 8.212903943950955465, 7.000000000000000000 ) ) ;
#38665 = CARTESIAN_POINT ( 'NONE',  ( -13.86789451117665095, 24.32149117241265301, -13.47705164427899938 ) ) ;
#38667 = EDGE_CURVE ( 'NONE', #34838, #26378, #22835, .T. ) ;
#38668 = CARTESIAN_POINT ( 'NONE',  ( -9.941839879247096334, -17.98565085000458197, -28.69025900671589824 ) ) ;
#38669 = LINE ( 'NONE', #10841, #13388 ) ;
#38670 = EDGE_CURVE ( 'NONE', #31336, #20131, #5453, .T. ) ;
#38671 = ORIENTED_EDGE ( 'NONE', *, *, #2271, .T. ) ;
#38672 = CARTESIAN_POINT ( 'NONE',  ( -27.67975872713484975, -11.41987064963364062, -15.71665464447120186 ) ) ;
#38673 = CARTESIAN_POINT ( 'NONE',  ( -9.133854131406611288, -18.57253604913642420, -27.48140049201442636 ) ) ;
#38674 = CARTESIAN_POINT ( 'NONE',  ( 24.08646667827958154, -13.28101593840524330, 23.00000000000000000 ) ) ;
#38675 = CARTESIAN_POINT ( 'NONE',  ( 15.09486127709339875, 17.52762106458872893, -18.81276594169348471 ) ) ;
#38676 = VERTEX_POINT ( 'NONE', #20898 ) ;
#38677 = CARTESIAN_POINT ( 'NONE',  ( 26.02691584061487973, 3.766903892757499595, -11.72995947271240524 ) ) ;
#38678 = CARTESIAN_POINT ( 'NONE',  ( -10.81260707898136708, 32.90853150812170469, 10.49999999999999822 ) ) ;
#38679 = DIRECTION ( 'NONE',  ( 0.1045284632676564129, 0.9945218953682731788, 0.000000000000000000 ) ) ;
#38680 = CIRCLE ( 'NONE', #30245, 1.000000000000000222 ) ;
#38681 = ORIENTED_EDGE ( 'NONE', *, *, #2425, .T. ) ;
#38682 = CARTESIAN_POINT ( 'NONE',  ( -20.82975236705524580, 0.6559526755414205601, -26.81703596920652544 ) ) ;
#38683 = CARTESIAN_POINT ( 'NONE',  ( 23.42995061493359543, 0.2370758946468835837, -20.49876334635902353 ) ) ;
#38684 = CIRCLE ( 'NONE', #4194, 0.5000000000000004441 ) ;
#38685 = VECTOR ( 'NONE', #15727, 1000.000000000000227 ) ;
#38686 = CARTESIAN_POINT ( 'NONE',  ( 31.50169271651470737, -8.384983552473938673, 19.27171037444156099 ) ) ;
#38687 = AXIS2_PLACEMENT_3D ( 'NONE', #8687, #18630, #15176 ) ;
#38688 = ORIENTED_EDGE ( 'NONE', *, *, #4837, .F. ) ;
#38689 = CARTESIAN_POINT ( 'NONE',  ( -27.03853842261034046, 1.817756925060996176, -12.62724191157268194 ) ) ;
#38690 = CARTESIAN_POINT ( 'NONE',  ( -16.84920187454418539, 29.09530251867925443, -5.000000000000000000 ) ) ;
#38691 = ADVANCED_FACE ( 'NONE', ( #3005 ), #3850, .F. ) ;
#38692 = DIRECTION ( 'NONE',  ( 1.000000000000000000, 0.000000000000000000, 0.000000000000000000 ) ) ;
#38693 = CARTESIAN_POINT ( 'NONE',  ( 6.935770203493858865, 22.34671014717335780, 12.00000000000000000 ) ) ;
#38694 = EDGE_CURVE ( 'NONE', #26220, #14950, #8048, .T. ) ;
#38695 = ADVANCED_FACE ( 'NONE', ( #11313 ), #16601, .T. ) ;
#38696 = CARTESIAN_POINT ( 'NONE',  ( 3.399837471815453593, 8.909889435135580626, 9.500000000000000000 ) ) ;
#38697 = DIRECTION ( 'NONE',  ( -0.9945218953682748442, -0.1045284632676391490, 0.000000000000000000 ) ) ;
#38698 = PLANE ( 'NONE',  #15948 ) ;
#38699 = VERTEX_POINT ( 'NONE', #10498 ) ;
#38700 = DIRECTION ( 'NONE',  ( 0.5000000000000041078, 0.8660254037844362651, 0.000000000000000000 ) ) ;
#38701 = DIRECTION ( 'NONE',  ( 1.000000000000000000, 0.000000000000000000, 0.000000000000000000 ) ) ;
#38702 = CARTESIAN_POINT ( 'NONE',  ( 16.15654479250856213, -14.01367662916781143, -25.66150427861421690 ) ) ;
#38703 = CARTESIAN_POINT ( 'NONE',  ( 7.468455364333220103, 29.89744377950669474, 10.00000000000000000 ) ) ;
#38704 = CARTESIAN_POINT ( 'NONE',  ( 8.796116341590819232, 23.42450908139080568, 7.000000000000000000 ) ) ;
#38705 = CARTESIAN_POINT ( 'NONE',  ( 11.39958526853898668, 19.89188415871232252, -21.52512903687211221 ) ) ;
#38706 = FILL_AREA_STYLE ('',( #10469 ) ) ;
#38707 = ORIENTED_EDGE ( 'NONE', *, *, #14263, .F. ) ;
#38709 = VECTOR ( 'NONE', #39064, 1000.000000000000000 ) ;
#38708 = CARTESIAN_POINT ( 'NONE',  ( -17.41140981635742691, 20.80174530708337244, -5.000000000000000000 ) ) ;
#38710 = CARTESIAN_POINT ( 'NONE',  ( -22.38472516250435973, -15.35952186208485593, 21.00000000000000000 ) ) ;
#38711 = CARTESIAN_POINT ( 'NONE',  ( 12.59484304515129516, -22.55689553818449156, -16.44840651353704786 ) ) ;
#38712 = DIRECTION ( 'NONE',  ( -0.07391278520355985815, 0.7032331762534049791, -0.7071067811865475727 ) ) ;
#38713 = CARTESIAN_POINT ( 'NONE',  ( 10.99531269100861763, 17.30182433700542788, -30.00000000000001421 ) ) ;
#38714 = ORIENTED_EDGE ( 'NONE', *, *, #9410, .F. ) ;
#38715 = CARTESIAN_POINT ( 'NONE',  ( 14.93529390890679664, 25.79829262747109198, -9.709001792061677349 ) ) ;
#38716 = ORIENTED_EDGE ( 'NONE', *, *, #22669, .F. ) ;
#38718 = CARTESIAN_POINT ( 'NONE',  ( 13.98881638187875787, 26.51951085733867330, 10.99999999999999289 ) ) ;
#38717 = CARTESIAN_POINT ( 'NONE',  ( -14.71284311239260667, 25.47114600920629002, -10.64827379499097226 ) ) ;
#38719 = ADVANCED_FACE ( 'NONE', ( #13741 ), #19848, .F. ) ;
#38720 = CARTESIAN_POINT ( 'NONE',  ( -15.31510379003943356, -26.50301315550676762, -7.358184284617420801 ) ) ;
#38721 = CARTESIAN_POINT ( 'NONE',  ( -36.04785107591552418, -18.56329043283772151, 11.55979286843925102 ) ) ;
#38722 = EDGE_CURVE ( 'NONE', #23375, #19728, #4688, .T. ) ;
#38723 = CARTESIAN_POINT ( 'NONE',  ( -27.21050208389111447, -17.59196774493118198, -13.80967687889205919 ) ) ;
#38724 = CARTESIAN_POINT ( 'NONE',  ( -4.980521078259840806, -20.55575703614546512, -24.29636214656850868 ) ) ;
#38725 = CARTESIAN_POINT ( 'NONE',  ( 15.93428740759538265, 25.01899822204553203, -5.000000000000000888 ) ) ;
#38726 = ORIENTED_EDGE ( 'NONE', *, *, #16307, .F. ) ;
#38727 = CARTESIAN_POINT ( 'NONE',  ( 20.37439232564474523, 8.397279452178770143, -20.08687019429353882 ) ) ;
#38728 = LINE ( 'NONE', #20247, #17378 ) ;
#38729 = LINE ( 'NONE', #13939, #37432 ) ;
#38730 = LINE ( 'NONE', #27141, #19308 ) ;
#38731 = ORIENTED_EDGE ( 'NONE', *, *, #37153, .F. ) ;
#38732 = CARTESIAN_POINT ( 'NONE',  ( -20.71492070759099136, -1.809969325171036481, -27.27634564961995878 ) ) ;
#38733 = CARTESIAN_POINT ( 'NONE',  ( -23.05386822411323422, -7.747535282638357224, 20.99999999999999645 ) ) ;
#38734 = ORIENTED_EDGE ( 'NONE', *, *, #25648, .F. ) ;
#38735 = CARTESIAN_POINT ( 'NONE',  ( 20.52988321362932922, -16.97904867242824523, 20.99999999999999645 ) ) ;
#38736 = DIRECTION ( 'NONE',  ( -0.000000000000000000, -0.000000000000000000, -1.000000000000000000 ) ) ;
#38737 = CARTESIAN_POINT ( 'NONE',  ( -11.54666566735214772, 32.07468077621344094, 7.000000000000000000 ) ) ;
#38738 = CARTESIAN_POINT ( 'NONE',  ( 19.88015388149283780, -9.459153964528258740, -24.23427547882557320 ) ) ;
#38739 = CARTESIAN_POINT ( 'NONE',  ( 35.62872793493669832, -3.428732413881706798, 12.14047268033096927 ) ) ;
#38740 = VECTOR ( 'NONE', #27536, 1000.000000000000000 ) ;
#38741 = ADVANCED_FACE ( 'NONE', ( #24489 ), #27147, .F. ) ;
#38742 = ORIENTED_EDGE ( 'NONE', *, *, #15425, .F. ) ;
#38743 = DIRECTION ( 'NONE',  ( 1.000000000000000000, 0.000000000000000000, 0.000000000000000000 ) ) ;
#38744 = CYLINDRICAL_SURFACE ( 'NONE', #2650, 1.000000000000000000 ) ;
#38745 = CARTESIAN_POINT ( 'NONE',  ( 9.183240348400453001, 28.21559575157615996, 12.00000000000000000 ) ) ;
#38746 = ORIENTED_EDGE ( 'NONE', *, *, #7907, .F. ) ;
#38747 = CARTESIAN_POINT ( 'NONE',  ( 1.146085828710420085, 27.91706644536319359, -17.59780091161095328 ) ) ;
#38748 = LINE ( 'NONE', #26354, #36652 ) ;
#38749 = CARTESIAN_POINT ( 'NONE',  ( -75.15099915297791711, 43.38844959084113384, -5.000000000000000000 ) ) ;
#38750 = DIRECTION ( 'NONE',  ( -0.000000000000000000, -0.000000000000000000, -1.000000000000000000 ) ) ;
#38751 = DIRECTION ( 'NONE',  ( -0.9945218953682742891, -0.1045284632676437425, 0.000000000000000000 ) ) ;
#38752 = FACE_OUTER_BOUND ( 'NONE', #5459, .T. ) ;
#38753 = CARTESIAN_POINT ( 'NONE',  ( 10.34603125738301266, 20.85552122335373681, -21.35002345354203968 ) ) ;
#38754 = DIRECTION ( 'NONE',  ( -0.000000000000000000, -0.000000000000000000, -1.000000000000000000 ) ) ;
#38755 = ORIENTED_EDGE ( 'NONE', *, *, #19410, .F. ) ;
#38757 = DIRECTION ( 'NONE',  ( 0.000000000000000000, 0.000000000000000000, 1.000000000000000000 ) ) ;
#38756 = CARTESIAN_POINT ( 'NONE',  ( -17.23503577783534624, 11.12556197759191967, -30.00000000000000000 ) ) ;
#38758 = DIRECTION ( 'NONE',  ( 1.000000000000000000, 0.000000000000000000, 0.000000000000000000 ) ) ;
#38759 = CARTESIAN_POINT ( 'NONE',  ( 11.57930096821026744, -20.97270239393662550, -19.49257125052969641 ) ) ;
#38760 = CARTESIAN_POINT ( 'NONE',  ( -4.082607396026893376, 23.58034083595207875, 13.00000000000000178 ) ) ;
#38761 = CARTESIAN_POINT ( 'NONE',  ( 14.00631563109706512, 23.99234777561873599, -13.50787202288133848 ) ) ;
#38762 = CARTESIAN_POINT ( 'NONE',  ( -21.88444403592365362, 6.126538576424530369, -30.00000000000001066 ) ) ;
#38763 = CARTESIAN_POINT ( 'NONE',  ( -19.30269652822713056, -16.27647962203388943, 23.00000000000001066 ) ) ;
#38764 = VECTOR ( 'NONE', #16342, 1000.000000000000000 ) ;
#38765 = AXIS2_PLACEMENT_3D ( 'NONE', #8294, #8495, #11746 ) ;
#38766 = CARTESIAN_POINT ( 'NONE',  ( -28.02256666113110128, -24.77408825670562820, -5.866844285589661645 ) ) ;
#38767 = CARTESIAN_POINT ( 'NONE',  ( 3.780512468825520056, -23.99670114915234720, -11.86248818774162572 ) ) ;
#38768 = CARTESIAN_POINT ( 'NONE',  ( 15.39800120669520389, 26.16141782975133623, -7.359158868726225045 ) ) ;
#38769 = CARTESIAN_POINT ( 'NONE',  ( 20.90635927389905291, 12.88005819179653599, -8.408867834709406353 ) ) ;
#38770 = FACE_OUTER_BOUND ( 'NONE', #26421, .T. ) ;
#38771 = EDGE_CURVE ( 'NONE', #18941, #20144, #24144, .T. ) ;
#38772 = ORIENTED_EDGE ( 'NONE', *, *, #16957, .F. ) ;
#38773 = CARTESIAN_POINT ( 'NONE',  ( -6.922216865142736708, 33.79108910511520492, -11.11993846343762016 ) ) ;
#38774 = AXIS2_PLACEMENT_3D ( 'NONE', #21008, #32606, #33014 ) ;
#38775 = EDGE_LOOP ( 'NONE', ( #39389, #2663, #2362, #20066 ) ) ;
#38776 = AXIS2_PLACEMENT_3D ( 'NONE', #20855, #23490, #35885 ) ;
#38777 = DIRECTION ( 'NONE',  ( 0.000000000000000000, 0.000000000000000000, 1.000000000000000000 ) ) ;
#38778 = ORIENTED_EDGE ( 'NONE', *, *, #14101, .T. ) ;
#38779 = CARTESIAN_POINT ( 'NONE',  ( -10.81260707898136353, 32.90853150812170469, 10.50000000000000000 ) ) ;
#38780 = CARTESIAN_POINT ( 'NONE',  ( 9.038171950369859431, 10.91067434175320017, 10.96580508970280654 ) ) ;
#38781 = EDGE_CURVE ( 'NONE', #880, #35978, #14407, .T. ) ;
#38782 = ORIENTED_EDGE ( 'NONE', *, *, #25268, .T. ) ;
#38783 = CARTESIAN_POINT ( 'NONE',  ( -23.89935431336828842, 0.5844314413813609388, -19.50775400706428897 ) ) ;
#38784 = EDGE_LOOP ( 'NONE', ( #39383, #21660 ) ) ;
#38785 = CARTESIAN_POINT ( 'NONE',  ( 23.29525806319241710, -7.038873791111292633, -20.85594693144456357 ) ) ;
#38786 = ORIENTED_EDGE ( 'NONE', *, *, #38303, .F. ) ;
#38787 = DIRECTION ( 'NONE',  ( 1.000000000000000000, 0.000000000000000000, 0.000000000000000000 ) ) ;
#38788 = ORIENTED_EDGE ( 'NONE', *, *, #3667, .T. ) ;
#38789 = CIRCLE ( 'NONE', #18125, 0.5000000000000004441 ) ;
#38790 = DIRECTION ( 'NONE',  ( 1.000000000000000000, 0.000000000000000000, 0.000000000000000000 ) ) ;
#38791 = CARTESIAN_POINT ( 'NONE',  ( -4.591666147298613332, 15.32946292166675306, 7.000000000000000000 ) ) ;
#38792 = CARTESIAN_POINT ( 'NONE',  ( 12.75384976115305236, 29.27371191231734571, 17.92354375535250455 ) ) ;
#38793 = AXIS2_PLACEMENT_3D ( 'NONE', #25977, #34934, #7491 ) ;
#38794 = CIRCLE ( 'NONE', #515, 15.00000000000000000 ) ;
#38795 = DIRECTION ( 'NONE',  ( -0.6123724356957894743, 0.3535533905932873311, -0.7071067811865451302 ) ) ;
#38796 = ORIENTED_EDGE ( 'NONE', *, *, #21993, .F. ) ;
#38797 = CARTESIAN_POINT ( 'NONE',  ( -19.48557158514998022, -11.24999999999982414, 3.000000000000000000 ) ) ;
#38798 = CARTESIAN_POINT ( 'NONE',  ( -6.811226782241547539, 35.33967249274200384, 7.000000000000000000 ) ) ;
#38799 = EDGE_CURVE ( 'NONE', #34302, #11394, #34532, .T. ) ;
#38800 = CARTESIAN_POINT ( 'NONE',  ( -20.66414367076832193, 17.76245163069108557, 10.99999999999809397 ) ) ;
#38801 = CARTESIAN_POINT ( 'NONE',  ( 18.72104006414143029, 16.54790594782236113, -9.860094852877404392 ) ) ;
#38802 = VECTOR ( 'NONE', #37179, 1000.000000000000227 ) ;
#38803 = CARTESIAN_POINT ( 'NONE',  ( 9.917373875393378668, 30.84216450598692916, -12.12503220460585851 ) ) ;
#38804 = ORIENTED_EDGE ( 'NONE', *, *, #1611, .T. ) ;
#38805 = CARTESIAN_POINT ( 'NONE',  ( -13.63581098909220302, 27.45627467658446719, 11.00000000000000000 ) ) ;
#38806 = CARTESIAN_POINT ( 'NONE',  ( 5.440908595777817602, 35.94977745735560859, 11.00000000000000000 ) ) ;
#38807 = CARTESIAN_POINT ( 'NONE',  ( 11.18272573551269566, -19.90824572261553271, -21.57092338806107179 ) ) ;
#38808 = CARTESIAN_POINT ( 'NONE',  ( 37.48507449946188785, -12.38247117345842341, -5.000000000000004441 ) ) ;
#38809 = CARTESIAN_POINT ( 'NONE',  ( -14.86556419889029534, 20.43481210330121556, 10.49999999999999822 ) ) ;
#38810 = ORIENTED_EDGE ( 'NONE', *, *, #22230, .F. ) ;
#38811 = CARTESIAN_POINT ( 'NONE',  ( -14.73694251361284913, 25.39790523529706334, -10.65305906957618021 ) ) ;
#38812 = CARTESIAN_POINT ( 'NONE',  ( -31.51573171626422010, 0.5582143012871293442, 15.13084544680214094 ) ) ;
#38813 = CARTESIAN_POINT ( 'NONE',  ( 14.29043209799990777, -26.44292502402198863, -5.000000000000000888 ) ) ;
#38814 = EDGE_CURVE ( 'NONE', #21971, #23024, #30797, .T. ) ;
#38815 = CYLINDRICAL_SURFACE ( 'NONE', #20530, 0.5000000000000015543 ) ;
#38816 = ORIENTED_EDGE ( 'NONE', *, *, #38437, .F. ) ;
#38817 = ORIENTED_EDGE ( 'NONE', *, *, #33101, .T. ) ;
#38818 = CARTESIAN_POINT ( 'NONE',  ( -9.053254851683428583, 24.89655747824621201, -17.93160491756381347 ) ) ;
#38819 = CARTESIAN_POINT ( 'NONE',  ( -2.518583951651200081, 7.712953814960714638, 7.000000000000000000 ) ) ;
#38820 = CARTESIAN_POINT ( 'NONE',  ( 2.025645716490518389, 8.212903943950921715, 7.499999999999990230 ) ) ;
#38821 = AXIS2_PLACEMENT_3D ( 'NONE', #15200, #36536, #21691 ) ;
#38822 = CARTESIAN_POINT ( 'NONE',  ( -20.80768648429576473, -4.462460184070209834, -25.80116617916775823 ) ) ;
#38823 = CARTESIAN_POINT ( 'NONE',  ( 15.48853125999100833, -26.74269726803731118, -0.000000000000000000 ) ) ;
#38824 = VERTEX_POINT ( 'NONE', #2961 ) ;
#38825 = CARTESIAN_POINT ( 'NONE',  ( 20.96220882709428324, 0.8789131500063240843, -26.23105454971878459 ) ) ;
#38826 = EDGE_CURVE ( 'NONE', #22802, #38413, #17023, .T. ) ;
#38827 = CARTESIAN_POINT ( 'NONE',  ( -12.27050296327057666, -16.73575495843078187, -27.23024630153084402 ) ) ;
#38828 = CARTESIAN_POINT ( 'NONE',  ( 32.33143948541783885, 1.358872982501748927, -5.000000000000000000 ) ) ;
#38829 = LINE ( 'NONE', #8146, #14147 ) ;
#38830 = ADVANCED_FACE ( 'NONE', ( #36889 ), #39724, .T. ) ;
#38831 = CIRCLE ( 'NONE', #31690, 1.000000000000000000 ) ;
#38832 = ORIENTED_EDGE ( 'NONE', *, *, #21456, .T. ) ;
#38833 = CARTESIAN_POINT ( 'NONE',  ( -25.21380665299743740, 0.3741287532325562881, -17.43820136744484017 ) ) ;
#38834 = CARTESIAN_POINT ( 'NONE',  ( 2.421689871081641687, 8.701977744317826335, 10.00000000000000000 ) ) ;
#38835 = VERTEX_POINT ( 'NONE', #11906 ) ;
#38836 = CARTESIAN_POINT ( 'NONE',  ( 31.81590626430815050, -2.991356775276182489, -9.994954404607028664 ) ) ;
#38837 = CIRCLE ( 'NONE', #31593, 1.000000000000000888 ) ;
#38838 = CARTESIAN_POINT ( 'NONE',  ( 36.50335543115979675, -9.090109797569423833, 14.53008259254010959 ) ) ;
#38839 = ORIENTED_EDGE ( 'NONE', *, *, #10616, .F. ) ;
#38840 = CARTESIAN_POINT ( 'NONE',  ( 16.81416712651216017, 27.17354907310114243, 13.92931973827808889 ) ) ;
#38841 = CARTESIAN_POINT ( 'NONE',  ( 15.74227866054390290, -25.75916161678440375, 17.42190598798392998 ) ) ;
#38842 = DIRECTION ( 'NONE',  ( 0.000000000000000000, 0.000000000000000000, 1.000000000000000000 ) ) ;
#38843 = CARTESIAN_POINT ( 'NONE',  ( -5.712781365377792575, 28.53852268908977052, 20.69868183039818277 ) ) ;
#38844 = LINE ( 'NONE', #7348, #14206 ) ;
#38845 = ORIENTED_EDGE ( 'NONE', *, *, #34431, .T. ) ;
#38846 = ADVANCED_FACE ( 'NONE', ( #33060 ), #21053, .T. ) ;
#38847 = DIRECTION ( 'NONE',  ( 0.000000000000000000, 0.000000000000000000, 1.000000000000000000 ) ) ;
#38848 = EDGE_CURVE ( 'NONE', #32089, #24654, #4010, .T. ) ;
#38849 = VECTOR ( 'NONE', #22584, 1000.000000000000000 ) ;
#38851 = VECTOR ( 'NONE', #13031, 1000.000000000000000 ) ;
#38850 = CARTESIAN_POINT ( 'NONE',  ( 4.739855970000743213, 35.45921866945190004, -10.19245697289364649 ) ) ;
#38852 = LINE ( 'NONE', #38649, #8686 ) ;
#38853 = CARTESIAN_POINT ( 'NONE',  ( 21.46287209667334039, 12.39159498259634695, 16.30093088680190405 ) ) ;
#38854 = CARTESIAN_POINT ( 'NONE',  ( 11.84905944520939158, -16.93912730843665315, -27.94593565603549123 ) ) ;
#38855 = CARTESIAN_POINT ( 'NONE',  ( -3.057264508911469392, 12.92643568347973826, 10.50000000000000533 ) ) ;
#38856 = AXIS2_PLACEMENT_3D ( 'NONE', #7955, #8368, #36597 ) ;
#38857 = DIRECTION ( 'NONE',  ( 1.000000000000000000, 0.000000000000000000, 0.000000000000000000 ) ) ;
#38858 = FACE_OUTER_BOUND ( 'NONE', #27048, .T. ) ;
#38859 = ORIENTED_EDGE ( 'NONE', *, *, #18562, .F. ) ;
#38860 = CARTESIAN_POINT ( 'NONE',  ( 13.16052575310691175, 22.32601956860930059, -16.43275809617471239 ) ) ;
#38861 = ORIENTED_EDGE ( 'NONE', *, *, #6394, .T. ) ;
#38862 = CARTESIAN_POINT ( 'NONE',  ( -15.36331629305222535, 25.66072101725646348, -8.302433069061233795 ) ) ;
#38863 = CARTESIAN_POINT ( 'NONE',  ( -30.00904163739982167, -13.36872314231684733, 19.99202127657103389 ) ) ;
#38864 = CARTESIAN_POINT ( 'NONE',  ( -2.362621116368410323, 8.178251995481311099, 10.83333333333333215 ) ) ;
#38865 = CARTESIAN_POINT ( 'NONE',  ( 15.44105900787717900, 26.60157864969849228, -5.946102268273840252 ) ) ;
#38866 = ORIENTED_EDGE ( 'NONE', *, *, #6558, .F. ) ;
#38867 = CARTESIAN_POINT ( 'NONE',  ( 17.40478573504346471, -11.01252481820737117, -28.44515566755788072 ) ) ;
#38868 = EDGE_LOOP ( 'NONE', ( #23142, #17664 ) ) ;
#38870 = CARTESIAN_POINT ( 'NONE',  ( -3.118678732975735279, 7.827785988993307242, 13.00000000000000178 ) ) ;
#38869 = CARTESIAN_POINT ( 'NONE',  ( -15.17875652326131863, 27.47441271400335694, -5.938670991771770602 ) ) ;
#38871 = CARTESIAN_POINT ( 'NONE',  ( -16.58921006345730120, -26.12567795957870942, -9.624075946779614199 ) ) ;
#38872 = EDGE_CURVE ( 'NONE', #27126, #4300, #5998, .T. ) ;
#38873 = CARTESIAN_POINT ( 'NONE',  ( 13.28503138821876917, 15.53523575316134142, 7.499999999999997335 ) ) ;
#38874 = ORIENTED_EDGE ( 'NONE', *, *, #23760, .F. ) ;
#38875 = CARTESIAN_POINT ( 'NONE',  ( -32.35609090632282658, -13.32965902131102709, -11.08975651091474468 ) ) ;
#38876 = CARTESIAN_POINT ( 'NONE',  ( -10.52791161976172596, -20.06334676836660336, -21.65469227164354038 ) ) ;
#38877 = DIRECTION ( 'NONE',  ( -0.000000000000000000, -0.000000000000000000, -1.000000000000000000 ) ) ;
#38878 = CARTESIAN_POINT ( 'NONE',  ( 15.29136776227527150, 19.45896063891741079, -15.68350118317069608 ) ) ;
#38879 = EDGE_LOOP ( 'NONE', ( #25972, #7745 ) ) ;
#38880 = CARTESIAN_POINT ( 'NONE',  ( 21.44184074642562976, 4.518366863407804246, -22.01530538004446669 ) ) ;
#38881 = CARTESIAN_POINT ( 'NONE',  ( -7.852310722359095330, 10.04909572729077105, 10.49999999999999822 ) ) ;
#38882 = CARTESIAN_POINT ( 'NONE',  ( 36.48557158514975640, -11.24999999999995559, 6.000000000000000000 ) ) ;
#38883 = ORIENTED_EDGE ( 'NONE', *, *, #26033, .F. ) ;
#38884 = CARTESIAN_POINT ( 'NONE',  ( -20.71012148218438043, 0.5861083848712056454, -27.43142461003399291 ) ) ;
#38886 = CARTESIAN_POINT ( 'NONE',  ( 22.87208170588712264, 0.1283377855311399196, -21.55196105168392151 ) ) ;
#38885 = AXIS2_PLACEMENT_3D ( 'NONE', #14789, #11541, #5840 ) ;
#38887 = VECTOR ( 'NONE', #38960, 1000.000000000000227 ) ;
#38888 = CARTESIAN_POINT ( 'NONE',  ( 24.23816072143611677, -22.57437281311106858, 19.27171037444157875 ) ) ;
#38889 = ORIENTED_EDGE ( 'NONE', *, *, #39336, .T. ) ;
#38890 = CARTESIAN_POINT ( 'NONE',  ( -20.49897829065735166, 2.206463918494783627, -28.14064370775090751 ) ) ;
#38891 = AXIS2_PLACEMENT_3D ( 'NONE', #18905, #27848, #3465 ) ;
#38892 = CARTESIAN_POINT ( 'NONE',  ( -33.62187204924172335, 0.04418559750806001774, -13.79123840944734347 ) ) ;
#38893 = LINE ( 'NONE', #14506, #24536 ) ;
#38894 = DIRECTION ( 'NONE',  ( 0.3090169943749573322, 0.9510565162951505336, -0.000000000000000000 ) ) ;
#38895 = EDGE_CURVE ( 'NONE', #20144, #20763, #5604, .T. ) ;
#38896 = CARTESIAN_POINT ( 'NONE',  ( -2.440759101148431309, 7.699698400927159625, 7.485646746502371940 ) ) ;
#38897 = CARTESIAN_POINT ( 'NONE',  ( 12.64210930126479937, 24.20081211342298744, 6.000000000000000000 ) ) ;
#38898 = FACE_OUTER_BOUND ( 'NONE', #12196, .T. ) ;
#38899 = ORIENTED_EDGE ( 'NONE', *, *, #14132, .T. ) ;
#38900 = CARTESIAN_POINT ( 'NONE',  ( -25.77311405540110911, 5.286159686137065883, -8.844531936936238736 ) ) ;
#38901 = LINE ( 'NONE', #35853, #32623 ) ;
#38902 = FACE_OUTER_BOUND ( 'NONE', #8029, .T. ) ;
#38903 = CARTESIAN_POINT ( 'NONE',  ( 28.35230428231212230, -24.61827297795788638, -5.000000000000000000 ) ) ;
#38904 = LINE ( 'NONE', #11081, #16438 ) ;
#38905 = DIRECTION ( 'NONE',  ( 0.5000000000000038858, 0.8660254037844364872, -0.000000000000000000 ) ) ;
#38906 = CARTESIAN_POINT ( 'NONE',  ( 10.90819920133987964, 17.95289977334026688, -26.19501740155092406 ) ) ;
#38907 = DIRECTION ( 'NONE',  ( -0.7431448254773846962, 0.6691306063588690067, -6.938893903907220489E-15 ) ) ;
#38908 = ORIENTED_EDGE ( 'NONE', *, *, #27283, .F. ) ;
#38909 = CARTESIAN_POINT ( 'NONE',  ( -13.94411147149912367, 15.13589321949257460, -28.21918225953774240 ) ) ;
#38910 = CARTESIAN_POINT ( 'NONE',  ( -22.30415078909513227, -16.34589999308528618, 20.99999999999995026 ) ) ;
#38911 = CARTESIAN_POINT ( 'NONE',  ( 9.458291886585664443, -18.18766449894053849, -29.34916192869308560 ) ) ;
#38912 = DIRECTION ( 'NONE',  ( 0.000000000000000000, 0.000000000000000000, -1.000000000000000000 ) ) ;
#38913 = CARTESIAN_POINT ( 'NONE',  ( 14.30088122820257368, 24.44632208664130246, -12.55129266994459059 ) ) ;
#38914 = VERTEX_POINT ( 'NONE', #14755 ) ;
#38915 = DIRECTION ( 'NONE',  ( 1.000000000000000000, 0.000000000000000000, 0.000000000000000000 ) ) ;
#38916 = ORIENTED_EDGE ( 'NONE', *, *, #26758, .T. ) ;
#38918 = CARTESIAN_POINT ( 'NONE',  ( -3.713592597587354049, 7.966960743906858156, 7.000000000000000000 ) ) ;
#38917 = CARTESIAN_POINT ( 'NONE',  ( -11.24611422795147853, 18.08780201161743406, -25.00577628530580299 ) ) ;
#38919 = CARTESIAN_POINT ( 'NONE',  ( -11.24122759046548481, -20.45868835281356723, -20.53405996523489563 ) ) ;
#38920 = EDGE_CURVE ( 'NONE', #7138, #38453, #23509, .T. ) ;
#38921 = CARTESIAN_POINT ( 'NONE',  ( -26.45121176803934304, -27.84758587393085350, 11.55979286843934872 ) ) ;
#38922 = CARTESIAN_POINT ( 'NONE',  ( -32.77147431096915398, -19.79161752149877174, -6.696281051292849895 ) ) ;
#38923 = CARTESIAN_POINT ( 'NONE',  ( -6.072675937371057486, -22.95838016832008677, -15.82819075888657068 ) ) ;
#38924 = CARTESIAN_POINT ( 'NONE',  ( 15.67293563814069124, 24.96974998548517277, -7.836397927719035650 ) ) ;
#38926 = EDGE_CURVE ( 'NONE', #18941, #26640, #20905, .T. ) ;
#38925 = ORIENTED_EDGE ( 'NONE', *, *, #5517, .T. ) ;
#38927 = CARTESIAN_POINT ( 'NONE',  ( 23.77017115979666428, 8.255607362891254297, -8.390682868101873026 ) ) ;
#38928 = CARTESIAN_POINT ( 'NONE',  ( -12.14717575287011719, 32.53695909538323860, 12.00000000000000000 ) ) ;
#38929 = DIRECTION ( 'NONE',  ( 1.000000000000000000, 0.000000000000000000, 0.000000000000000000 ) ) ;
#38930 = CARTESIAN_POINT ( 'NONE',  ( 3.914034194965611668, 30.06176806842419680, 9.000000000000001776 ) ) ;
#38931 = ORIENTED_EDGE ( 'NONE', *, *, #14771, .T. ) ;
#38932 = CARTESIAN_POINT ( 'NONE',  ( -31.69715058011894016, -2.389216380787061222, -9.565402919442236751 ) ) ;
#38933 = EDGE_CURVE ( 'NONE', #16076, #39330, #13758, .T. ) ;
#38934 = CARTESIAN_POINT ( 'NONE',  ( -17.01074486384391449, 2.963432112732212520, 20.82122704794078771 ) ) ;
#38935 = CARTESIAN_POINT ( 'NONE',  ( 21.38319344285460843, -17.62079982023265501, 20.94377226548386517 ) ) ;
#38936 = DIRECTION ( 'NONE',  ( 0.9781476007338043566, -0.2079116908177657264, 0.000000000000000000 ) ) ;
#38937 = DIRECTION ( 'NONE',  ( 0.2113248654051944064, 0.7886751345948047609, 0.5773502691896342798 ) ) ;
#38938 = CARTESIAN_POINT ( 'NONE',  ( 18.59608826487667343, -8.852250640322028019, -28.44979860309804920 ) ) ;
#38939 = DIRECTION ( 'NONE',  ( -1.000000000000000000, 0.000000000000000000, 0.000000000000000000 ) ) ;
#38940 = CONICAL_SURFACE ( 'NONE', #35700, 0.5000000000000065503, 0.7853981633974495002 ) ;
#38941 = ORIENTED_EDGE ( 'NONE', *, *, #32459, .F. ) ;
#38942 = EDGE_CURVE ( 'NONE', #10398, #2507, #37775, .T. ) ;
#38943 = VECTOR ( 'NONE', #11272, 1000.000000000000114 ) ;
#38944 = CYLINDRICAL_SURFACE ( 'NONE', #9998, 1.000000000000000000 ) ;
#38945 = EDGE_CURVE ( 'NONE', #19314, #2033, #2752, .T. ) ;
#38946 = ADVANCED_FACE ( 'NONE', ( #14552 ), #39333, .T. ) ;
#38947 = CARTESIAN_POINT ( 'NONE',  ( 6.643188263510064751, 35.96180620077102219, 10.49999999999999822 ) ) ;
#38948 = CARTESIAN_POINT ( 'NONE',  ( 0.5000000000000002220, 36.00000000000000711, 10.00000000000000000 ) ) ;
#38949 = CARTESIAN_POINT ( 'NONE',  ( 1.565334152085329888, 38.07008842306128571, -7.117895202388205611 ) ) ;
#38950 = DIRECTION ( 'NONE',  ( 0.000000000000000000, 0.000000000000000000, 1.000000000000000000 ) ) ;
#38951 = CARTESIAN_POINT ( 'NONE',  ( 16.81416712651216017, 27.17354907310113887, 13.92931973827808712 ) ) ;
#38952 = DIRECTION ( 'NONE',  ( 0.000000000000000000, 0.000000000000000000, -1.000000000000000000 ) ) ;
#38953 = CARTESIAN_POINT ( 'NONE',  ( 12.74038105676654453, 14.56698729810772264, 10.49999999999999822 ) ) ;
#38954 = CARTESIAN_POINT ( 'NONE',  ( 9.427394655437332460, 10.98460639141775808, 10.49999999999999645 ) ) ;
#38955 = CARTESIAN_POINT ( 'NONE',  ( 11.69402330146858482, 21.36632422587266689, -19.35895708507096202 ) ) ;
#38956 = DIRECTION ( 'NONE',  ( -1.000000000000000000, 0.000000000000000000, 0.000000000000000000 ) ) ;
#38957 = ORIENTED_EDGE ( 'NONE', *, *, #39842, .T. ) ;
#38958 = VECTOR ( 'NONE', #13955, 1000.000000000000114 ) ;
#38960 = DIRECTION ( 'NONE',  ( 0.9945218953682742891, 0.1045284632676437425, -0.000000000000000000 ) ) ;
#38959 = CARTESIAN_POINT ( 'NONE',  ( -18.76357486801690655, 13.43274215842698993, -15.92991587464894288 ) ) ;
#38961 = LINE ( 'NONE', #35720, #16620 ) ;
#38962 = CARTESIAN_POINT ( 'NONE',  ( 14.39131927975945402, -25.07688395697384465, -11.59674742285950089 ) ) ;
#38963 = CARTESIAN_POINT ( 'NONE',  ( 8.410254037844358876, 17.06698729810774395, 10.49999999999999822 ) ) ;
#38964 = CARTESIAN_POINT ( 'NONE',  ( 11.66333929151196713, 18.93342404723955852, -22.73119902039520568 ) ) ;
#38965 = CARTESIAN_POINT ( 'NONE',  ( 11.31392148919590923, 36.91540483778863546, -5.000000000000002665 ) ) ;
#38966 = CARTESIAN_POINT ( 'NONE',  ( -23.54277854204216069, -14.22284186533119410, 22.99999999999999645 ) ) ;
#38967 = ADVANCED_FACE ( 'NONE', ( #35388 ), #19338, .T. ) ;
#38968 = CARTESIAN_POINT ( 'NONE',  ( -15.43503188818483451, -13.62775707822376070, -28.48261797098671266 ) ) ;
#38969 = CARTESIAN_POINT ( 'NONE',  ( 4.192399910511806382, -20.06660217949758618, -30.00000000000001776 ) ) ;
#38970 = CARTESIAN_POINT ( 'NONE',  ( 11.16317946027923824, 17.19403390828999889, -30.00000000000000355 ) ) ;
#38971 = ADVANCED_FACE ( 'NONE', ( #24888 ), #35180, .F. ) ;
#38972 = CARTESIAN_POINT ( 'NONE',  ( 20.85031025169343266, 12.84359668456042591, -8.901149520029621343 ) ) ;
#38973 = DIRECTION ( 'NONE',  ( 0.000000000000000000, 0.000000000000000000, -1.000000000000000000 ) ) ;
#38974 = ORIENTED_EDGE ( 'NONE', *, *, #20212, .F. ) ;
#38975 = AXIS2_PLACEMENT_3D ( 'NONE', #34552, #429, #19111 ) ;
#38976 = CARTESIAN_POINT ( 'NONE',  ( -7.236536542773612801, 35.44204148769340179, -8.885907059458707735 ) ) ;
#38977 = ORIENTED_EDGE ( 'NONE', *, *, #27527, .T. ) ;
#38978 = CARTESIAN_POINT ( 'NONE',  ( 2.494936919103933448, 34.23777120880591696, 13.00000000000000178 ) ) ;
#38979 = VERTEX_POINT ( 'NONE', #25831 ) ;
#38980 = DIRECTION ( 'NONE',  ( 1.000000000000000000, 0.000000000000000000, 0.000000000000000000 ) ) ;
#38981 = DIRECTION ( 'NONE',  ( 0.000000000000000000, 0.000000000000000000, 1.000000000000000000 ) ) ;
#38982 = ORIENTED_EDGE ( 'NONE', *, *, #27736, .T. ) ;
#38983 = CARTESIAN_POINT ( 'NONE',  ( -24.49105222923185821, 0.5749155098870283309, -18.46773377504650782 ) ) ;
#38984 = ORIENTED_EDGE ( 'NONE', *, *, #8528, .T. ) ;
#38985 = CARTESIAN_POINT ( 'NONE',  ( 34.58134563245810256, -10.42100876475338467, -8.458827757296450756 ) ) ;
#38986 = VECTOR ( 'NONE', #23207, 1000.000000000000227 ) ;
#38987 = ORIENTED_EDGE ( 'NONE', *, *, #22044, .F. ) ;
#38988 = DIRECTION ( 'NONE',  ( -0.1470157664652021190, 0.6916548014802263999, -0.7071067811865459074 ) ) ;
#38989 = ORIENTED_EDGE ( 'NONE', *, *, #19138, .F. ) ;
#38990 = FACE_OUTER_BOUND ( 'NONE', #1617, .T. ) ;
#38991 = CARTESIAN_POINT ( 'NONE',  ( 7.611215932167711529, 18.68301270189218855, 9.000000000000001776 ) ) ;
#38992 = CARTESIAN_POINT ( 'NONE',  ( -10.78342637327578224, 29.81468131102269936, 18.87996532025784546 ) ) ;
#38993 = DIRECTION ( 'NONE',  ( 0.000000000000000000, -0.6445931928399307731, 0.7645257456387090089 ) ) ;
#38994 = VERTEX_POINT ( 'NONE', #19946 ) ;
#38995 = DIRECTION ( 'NONE',  ( 0.000000000000000000, 0.000000000000000000, 1.000000000000000000 ) ) ;
#38996 = CARTESIAN_POINT ( 'NONE',  ( 5.440829913680675034, 10.60893893836775348, 13.00000000000000178 ) ) ;
#38997 = EDGE_CURVE ( 'NONE', #8563, #34372, #29847, .T. ) ;
#38998 = AXIS2_PLACEMENT_3D ( 'NONE', #10316, #22898, #23317 ) ;
#38999 = CARTESIAN_POINT ( 'NONE',  ( 4.817371740575539185, 23.83900317890011422, 23.00000000000000000 ) ) ;
#39000 = CARTESIAN_POINT ( 'NONE',  ( 18.25029525998795066, 16.00669453228446670, -12.84108188352884206 ) ) ;
#39001 = CARTESIAN_POINT ( 'NONE',  ( 7.669720458042128541, 19.54291380638433040, -26.53555194593364064 ) ) ;
#39002 = ORIENTED_EDGE ( 'NONE', *, *, #33265, .F. ) ;
#39003 = CARTESIAN_POINT ( 'NONE',  ( 5.198706521309295780, 29.65540566576566661, 7.000000000000000000 ) ) ;
#39004 = CARTESIAN_POINT ( 'NONE',  ( 13.63581098909226874, 27.45627467658428955, 9.000000000000001776 ) ) ;
#39005 = CARTESIAN_POINT ( 'NONE',  ( 14.28460229709901519, -24.65033995194861660, -12.53151620945226341 ) ) ;
#39006 = CARTESIAN_POINT ( 'NONE',  ( 20.55563217186196212, -29.52600041847795254, -5.000000000000018652 ) ) ;
#39007 = CARTESIAN_POINT ( 'NONE',  ( -14.47283171447380212, 21.48159823030330529, 11.00000000000000000 ) ) ;
#39008 = CARTESIAN_POINT ( 'NONE',  ( -12.38581555130674872, 20.49744764627239491, -19.49524353550787126 ) ) ;
#39009 = CARTESIAN_POINT ( 'NONE',  ( -15.27443809246124218, -27.57253143578281041, 15.13084544680213561 ) ) ;
#39010 = CARTESIAN_POINT ( 'NONE',  ( 8.962294377823376124, -18.56986243642861112, -28.10993916399811354 ) ) ;
#39011 = VECTOR ( 'NONE', #2866, 1000.000000000000000 ) ;
#39012 = DIRECTION ( 'NONE',  ( -0.3090169943749573878, -0.9510565162951503115, 0.000000000000000000 ) ) ;
#39013 = VERTEX_POINT ( 'NONE', #16499 ) ;
#39014 = ORIENTED_EDGE ( 'NONE', *, *, #31511, .T. ) ;
#39015 = CARTESIAN_POINT ( 'NONE',  ( -11.29360755245008718, 31.24910176029843711, -10.34195632950957844 ) ) ;
#39016 = DIRECTION ( 'NONE',  ( -1.000000000000000000, 0.000000000000000000, 0.000000000000000000 ) ) ;
#39017 = FACE_BOUND ( 'NONE', #25829, .T. ) ;
#39018 = CARTESIAN_POINT ( 'NONE',  ( -21.37767459502805778, -3.913953112044378457, -24.54261330738080460 ) ) ;
#39019 = CARTESIAN_POINT ( 'NONE',  ( 0.000000000000000000, 22.50000000000000355, 13.00000000000000178 ) ) ;
#39020 = ORIENTED_EDGE ( 'NONE', *, *, #35569, .T. ) ;
#39021 = CARTESIAN_POINT ( 'NONE',  ( 30.26282733560709559, 0.09093532349598118514, -8.298613290467722337 ) ) ;
#39022 = DIRECTION ( 'NONE',  ( -0.000000000000000000, -0.000000000000000000, -1.000000000000000000 ) ) ;
#39023 = CARTESIAN_POINT ( 'NONE',  ( 11.14716901145161643, 12.46304090461738667, 13.00000000000000178 ) ) ;
#39024 = AXIS2_PLACEMENT_3D ( 'NONE', #21927, #1003, #22129 ) ;
#39025 = DIRECTION ( 'NONE',  ( 1.000000000000000000, 0.000000000000000000, 0.000000000000000000 ) ) ;
#39026 = EDGE_LOOP ( 'NONE', ( #21377, #17516 ) ) ;
#39027 = CARTESIAN_POINT ( 'NONE',  ( -20.48192033757745278, 0.8608427067432725677, -30.00000000000000000 ) ) ;
#39028 = CYLINDRICAL_SURFACE ( 'NONE', #27421, 1.000000000000000888 ) ;
#39029 = ORIENTED_EDGE ( 'NONE', *, *, #20205, .T. ) ;
#39030 = CARTESIAN_POINT ( 'NONE',  ( 29.94967456567781028, -3.579765429977533220, -13.19994935436286809 ) ) ;
#39031 = CARTESIAN_POINT ( 'NONE',  ( 35.08890111189684546, -5.671281373296992001, 15.72805884748904681 ) ) ;
#39032 = ORIENTED_EDGE ( 'NONE', *, *, #8420, .F. ) ;
#39033 = CARTESIAN_POINT ( 'NONE',  ( 8.901509289502147482, 37.28103075694621538, 14.53008259254014689 ) ) ;
#39034 = CARTESIAN_POINT ( 'NONE',  ( 10.81727955709540723, -23.19337658755338083, 18.42518152271931697 ) ) ;
#39035 = CARTESIAN_POINT ( 'NONE',  ( 7.935770203493858865, 22.34671014717335780, 12.00000000000000000 ) ) ;
#39036 = CARTESIAN_POINT ( 'NONE',  ( 7.341569467741936528, 26.39884405248101373, 20.69868183039782039 ) ) ;
#39037 = AXIS2_PLACEMENT_3D ( 'NONE', #35098, #10514, #25746 ) ;
#39038 = PLANE ( 'NONE',  #17475 ) ;
#39039 = VERTEX_POINT ( 'NONE', #25626 ) ;
#39040 = EDGE_CURVE ( 'NONE', #11564, #4629, #34988, .T. ) ;
#39041 = LINE ( 'NONE', #6990, #24960 ) ;
#39042 = LINE ( 'NONE', #14459, #17605 ) ;
#39043 = CARTESIAN_POINT ( 'NONE',  ( 2.701375607076830221, 20.57380448486020086, -27.72792284495386994 ) ) ;
#39044 = CARTESIAN_POINT ( 'NONE',  ( 28.79410123593972415, 4.962698632456642223, -5.000000000000000000 ) ) ;
#39045 = EDGE_CURVE ( 'NONE', #26235, #5593, #1058, .T. ) ;
#39046 = CARTESIAN_POINT ( 'NONE',  ( 15.00309677617812554, 1.567672476142359939, 20.99999999999999645 ) ) ;
#39047 = AXIS2_PLACEMENT_3D ( 'NONE', #13787, #26586, #17459 ) ;
#39048 = EDGE_CURVE ( 'NONE', #19095, #36376, #31910, .T. ) ;
#39049 = CARTESIAN_POINT ( 'NONE',  ( 12.97325122237492145, -17.30183730846044554, -24.66100610027864093 ) ) ;
#39050 = DIRECTION ( 'NONE',  ( 1.000000000000000000, 0.000000000000000000, 0.000000000000000000 ) ) ;
#39051 = CARTESIAN_POINT ( 'NONE',  ( 1.693998953219503445, 12.12549434688615690, 10.50000000000000000 ) ) ;
#39052 = DIRECTION ( 'NONE',  ( 0.000000000000000000, 0.000000000000000000, 1.000000000000000000 ) ) ;
#39053 = ORIENTED_EDGE ( 'NONE', *, *, #35361, .T. ) ;
#39054 = CARTESIAN_POINT ( 'NONE',  ( 13.97401297928019481, 24.07084740764522124, -13.50045613746490325 ) ) ;
#39055 = EDGE_LOOP ( 'NONE', ( #29314, #40071, #21839, #90 ) ) ;
#39056 = CARTESIAN_POINT ( 'NONE',  ( -11.43474607271607724, 17.01453699462772207, -29.35782462692642625 ) ) ;
#39057 = CARTESIAN_POINT ( 'NONE',  ( -32.41210168510392009, -9.609370058585097851, 18.87996532025784546 ) ) ;
#39058 = DIRECTION ( 'NONE',  ( 1.000000000000000000, 0.000000000000000000, 0.000000000000000000 ) ) ;
#39059 = CARTESIAN_POINT ( 'NONE',  ( 15.04605592278479875, 25.88023467481654905, -9.239420567519900374 ) ) ;
#39060 = ORIENTED_EDGE ( 'NONE', *, *, #4304, .F. ) ;
#39061 = CARTESIAN_POINT ( 'NONE',  ( 29.70373973584631955, -17.57897857355148830, -11.97277981779456901 ) ) ;
#39062 = ORIENTED_EDGE ( 'NONE', *, *, #12404, .F. ) ;
#39064 = DIRECTION ( 'NONE',  ( -0.000000000000000000, -0.000000000000000000, -1.000000000000000000 ) ) ;
#39063 = CARTESIAN_POINT ( 'NONE',  ( -12.97748996312875747, 22.65302653440283009, -16.39225588091346353 ) ) ;
#39065 = CARTESIAN_POINT ( 'NONE',  ( -11.66758301494133043, -19.21216028216936422, -22.58759682042235184 ) ) ;
#39066 = CARTESIAN_POINT ( 'NONE',  ( 13.00577423375721864, 27.77729443754439487, 9.500000000000000000 ) ) ;
#39067 = ORIENTED_EDGE ( 'NONE', *, *, #28496, .T. ) ;
#39068 = CARTESIAN_POINT ( 'NONE',  ( -31.87840698781867133, -10.92544140939488173, -12.02591668823370874 ) ) ;
#39069 = CARTESIAN_POINT ( 'NONE',  ( -12.15224344198015949, -22.55312021461349303, -16.48165687185815642 ) ) ;
#39070 = AXIS2_PLACEMENT_3D ( 'NONE', #30767, #27702, #15522 ) ;
#39071 = LINE ( 'NONE', #11249, #4722 ) ;
#39072 = EDGE_LOOP ( 'NONE', ( #17383, #38086, #38056, #40013 ) ) ;
#39073 = CARTESIAN_POINT ( 'NONE',  ( 21.18854743806299368, 3.064997187841227877, -24.09357946227068936 ) ) ;
#39074 = DIRECTION ( 'NONE',  ( 0.000000000000000000, 0.000000000000000000, 1.000000000000000000 ) ) ;
#39075 = EDGE_CURVE ( 'NONE', #36019, #1586, #25435, .T. ) ;
#39076 = CARTESIAN_POINT ( 'NONE',  ( -35.27625572565260370, 1.213838575766586603, 11.00000000000000000 ) ) ;
#39077 = ADVANCED_FACE ( 'NONE', ( #22779 ), #19755, .T. ) ;
#39078 = VERTEX_POINT ( 'NONE', #36191 ) ;
#39079 = CARTESIAN_POINT ( 'NONE',  ( -22.26224525938009435, 0.4962469403767001963, -22.71332818809632670 ) ) ;
#39080 = CARTESIAN_POINT ( 'NONE',  ( 22.37143894708468395, 0.01545002306387475294, -22.65172220279661275 ) ) ;
#39081 = CARTESIAN_POINT ( 'NONE',  ( 31.52520841578668254, -13.67397774227536367, 19.27171037444156099 ) ) ;
#39082 = ORIENTED_EDGE ( 'NONE', *, *, #4564, .T. ) ;
#39083 = VECTOR ( 'NONE', #6491, 1000.000000000000227 ) ;
#39084 = CARTESIAN_POINT ( 'NONE',  ( -22.03994032835833750, 1.381754348432899349, -22.81883089661271669 ) ) ;
#39085 = CARTESIAN_POINT ( 'NONE',  ( 11.10756861982301125, 19.59949212537556562, -30.00000000000000000 ) ) ;
#39086 = DIRECTION ( 'NONE',  ( 0.000000000000000000, 0.000000000000000000, -1.000000000000000000 ) ) ;
#39087 = VECTOR ( 'NONE', #10235, 1000.000000000000114 ) ;
#39088 = DIRECTION ( 'NONE',  ( -0.000000000000000000, -0.000000000000000000, -1.000000000000000000 ) ) ;
#39089 = EDGE_CURVE ( 'NONE', #23174, #24240, #37114, .T. ) ;
#39090 = CARTESIAN_POINT ( 'NONE',  ( 13.87104230352200140, 20.53934056656866147, 7.500000000000010658 ) ) ;
#39091 = CARTESIAN_POINT ( 'NONE',  ( 0.2655024426717602637, 36.24516302788250499, 12.00000000000000000 ) ) ;
#39092 = DIRECTION ( 'NONE',  ( -0.000000000000000000, -0.000000000000000000, 1.000000000000000000 ) ) ;
#39093 = ORIENTED_EDGE ( 'NONE', *, *, #2328, .F. ) ;
#39094 = CARTESIAN_POINT ( 'NONE',  ( -20.36895863172275156, 5.751155262373932153, -24.28491833738754835 ) ) ;
#39095 = CARTESIAN_POINT ( 'NONE',  ( 10.80697542085375140, 31.15003855377755571, 6.000000000000000000 ) ) ;
#39096 = DIRECTION ( 'NONE',  ( 0.000000000000000000, 0.000000000000000000, 1.000000000000000000 ) ) ;
#39097 = CARTESIAN_POINT ( 'NONE',  ( 17.32694539406390177, -16.96442657344122296, -20.89054752054989805 ) ) ;
#39098 = CARTESIAN_POINT ( 'NONE',  ( 9.819582157326486538, 24.63911342745429778, 10.50000000000000533 ) ) ;
#39099 = CARTESIAN_POINT ( 'NONE',  ( 10.72215843559913750, 17.73370681071187605, -27.42052473872761098 ) ) ;
#39100 = VECTOR ( 'NONE', #5772, 1000.000000000000000 ) ;
#39101 = CARTESIAN_POINT ( 'NONE',  ( -9.697889840765288483, 31.90483559858339646, 9.500000000000000000 ) ) ;
#39102 = ORIENTED_EDGE ( 'NONE', *, *, #34983, .T. ) ;
#39103 = CARTESIAN_POINT ( 'NONE',  ( -15.20072915685657122, 20.47391248462032465, -14.64817096683644593 ) ) ;
#39104 = CARTESIAN_POINT ( 'NONE',  ( -18.76090689389218014, -16.22676322417297001, 20.99999999999999645 ) ) ;
#39105 = CIRCLE ( 'NONE', #25468, 1.000000000000000000 ) ;
#39106 = DIRECTION ( 'NONE',  ( 0.000000000000000000, 0.000000000000000000, 1.000000000000000000 ) ) ;
#39107 = CARTESIAN_POINT ( 'NONE',  ( 14.74653517655818291, 25.36980923495725548, -10.65380407947966823 ) ) ;
#39108 = VERTEX_POINT ( 'NONE', #39425 ) ;
#39109 = CARTESIAN_POINT ( 'NONE',  ( -14.97009266215794376, 21.42933399866948463, 10.50000000000000178 ) ) ;
#39110 = ORIENTED_EDGE ( 'NONE', *, *, #25174, .T. ) ;
#39112 = LINE ( 'NONE', #27325, #30276 ) ;
#39111 = CARTESIAN_POINT ( 'NONE',  ( -14.69323628723109998, 25.52969830242819427, -10.64447204089981014 ) ) ;
#39113 = CARTESIAN_POINT ( 'NONE',  ( -15.57263558642642032, -26.76429566359157164, -5.000000000000000888 ) ) ;
#39114 = CARTESIAN_POINT ( 'NONE',  ( -32.80061120326500657, -23.42582577749657347, 12.14047268033081295 ) ) ;
#39115 = CIRCLE ( 'NONE', #3411, 0.5000000000000004441 ) ;
#39116 = CARTESIAN_POINT ( 'NONE',  ( -30.97886774876783633, -18.71541742275284648, -10.17228780496799878 ) ) ;
#39117 = CARTESIAN_POINT ( 'NONE',  ( -6.137033441707241188, -19.64448462102270909, -28.81001259779947077 ) ) ;
#39118 = CARTESIAN_POINT ( 'NONE',  ( 13.39920212058827964, 20.89892004213690768, -17.51356503033543888 ) ) ;
#39119 = ORIENTED_EDGE ( 'NONE', *, *, #19083, .T. ) ;
#39120 = CARTESIAN_POINT ( 'NONE',  ( 24.66102986608180103, 7.389241230280822137, -5.000000000000000888 ) ) ;
#39121 = DIRECTION ( 'NONE',  ( -1.000000000000000000, 0.000000000000000000, 0.000000000000000000 ) ) ;
#39122 = CARTESIAN_POINT ( 'NONE',  ( -15.26585111513660209, 17.86474508437623143, 12.00000000000000000 ) ) ;
#39123 = ADVANCED_FACE ( 'NONE', ( #8553 ), #20555, .T. ) ;
#39124 = PLANE ( 'NONE',  #36836 ) ;
#39125 = ORIENTED_EDGE ( 'NONE', *, *, #29980, .T. ) ;
#39126 = CARTESIAN_POINT ( 'NONE',  ( -32.30815150485408793, -1.680769291408187538, -5.465098400837421266 ) ) ;
#39127 = VECTOR ( 'NONE', #31203, 1000.000000000000000 ) ;
#39128 = CARTESIAN_POINT ( 'NONE',  ( 24.56621758168594738, 0.4171823343055403588, -18.45072505565352472 ) ) ;
#39129 = CARTESIAN_POINT ( 'NONE',  ( -17.69280599717042080, 3.437614796744613344, 20.69868183039779908 ) ) ;
#39130 = CARTESIAN_POINT ( 'NONE',  ( 18.03924190088524782, -16.85603499720511067, 20.99999999999999645 ) ) ;
#39131 = CARTESIAN_POINT ( 'NONE',  ( -13.28503138821885798, 15.53523575316151195, 7.499999999999993783 ) ) ;
#39132 =( NAMED_UNIT ( * ) SI_UNIT ( $, .STERADIAN. ) SOLID_ANGLE_UNIT ( ) );
#39133 = AXIS2_PLACEMENT_3D ( 'NONE', #13949, #11513, #14152 ) ;
#39134 = CARTESIAN_POINT ( 'NONE',  ( 33.69589222704781406, -0.03122585499636791606, 11.55979286843971465 ) ) ;
#39135 = ORIENTED_EDGE ( 'NONE', *, *, #38670, .F. ) ;
#39136 = CARTESIAN_POINT ( 'NONE',  ( -12.68475447279705470, 27.14725768220950641, 10.00000000000000000 ) ) ;
#39137 = ADVANCED_FACE ( 'NONE', ( #17110 ), #26639, .T. ) ;
#39138 = AXIS2_PLACEMENT_3D ( 'NONE', #13301, #9865, #25698 ) ;
#39139 = CARTESIAN_POINT ( 'NONE',  ( 6.513333500389088648, 35.89988989478896997, 10.82238861112342043 ) ) ;
#39140 = CARTESIAN_POINT ( 'NONE',  ( -8.927394655428429360, 11.06314620770957013, 9.000000000000001776 ) ) ;
#39141 = ADVANCED_FACE ( 'NONE', ( #29886 ), #20151, .T. ) ;
#39142 = CARTESIAN_POINT ( 'NONE',  ( 0.8699709723833062291, 21.42695088328918018, -25.57864724691659930 ) ) ;
#39143 = CARTESIAN_POINT ( 'NONE',  ( -5.198706521309195416, 29.65540566576573767, 9.000000000000001776 ) ) ;
#39144 = CARTESIAN_POINT ( 'NONE',  ( -12.92073081513906452, 15.61756285494255003, 11.00000000000000000 ) ) ;
#39145 = DIRECTION ( 'NONE',  ( -0.000000000000000000, -0.000000000000000000, -1.000000000000000000 ) ) ;
#39146 = CYLINDRICAL_SURFACE ( 'NONE', #34593, 58.00000000000007816 ) ;
#39147 = AXIS2_PLACEMENT_3D ( 'NONE', #4776, #33030, #39502 ) ;
#39148 = LINE ( 'NONE', #11127, #39827 ) ;
#39149 = CARTESIAN_POINT ( 'NONE',  ( 12.04999115871534876, 22.98224508480782902, -17.26137212625882000 ) ) ;
#39150 = CYLINDRICAL_SURFACE ( 'NONE', #9479, 6.000000000000015987 ) ;
#39151 = ORIENTED_EDGE ( 'NONE', *, *, #2120, .F. ) ;
#39152 = EDGE_CURVE ( 'NONE', #26378, #20669, #26234, .T. ) ;
#39154 = CARTESIAN_POINT ( 'NONE',  ( 0.000000000000000000, 22.50000000000000355, 11.00000000000000178 ) ) ;
#39153 = CARTESIAN_POINT ( 'NONE',  ( -18.19708040568177410, 15.52697327766063218, -13.86016582398509556 ) ) ;
#39155 = AXIS2_PLACEMENT_3D ( 'NONE', #3709, #31943, #10011 ) ;
#39156 = CARTESIAN_POINT ( 'NONE',  ( -0.4999999999999998890, 37.50000000000000711, 10.49999999999999467 ) ) ;
#39157 = CARTESIAN_POINT ( 'NONE',  ( 15.50471485482113820, -26.74686345152265332, -5.000000000000000888 ) ) ;
#39158 = DIRECTION ( 'NONE',  ( 1.000000000000000000, 0.000000000000000000, 0.000000000000000000 ) ) ;
#39159 = CARTESIAN_POINT ( 'NONE',  ( 15.32564493454926513, 26.66194327151340815, -6.887025365065524873 ) ) ;
#39160 = CARTESIAN_POINT ( 'NONE',  ( 11.10756861982301125, 19.59949212537556562, -30.00000000000000000 ) ) ;
#39161 = DIRECTION ( 'NONE',  ( -1.000000000000000000, 0.000000000000000000, 0.000000000000000000 ) ) ;
#39162 = VECTOR ( 'NONE', #32872, 1000.000000000000000 ) ;
#39163 = CARTESIAN_POINT ( 'NONE',  ( -26.61378535533439305, -24.97840923415078862, -7.589850937743148229 ) ) ;
#39164 = CARTESIAN_POINT ( 'NONE',  ( 3.837299910079773557, -24.19987090832864496, -10.86751699812955962 ) ) ;
#39165 = CARTESIAN_POINT ( 'NONE',  ( 11.16317946027923824, 17.19403390828999889, -29.35217987579671117 ) ) ;
#39166 = CARTESIAN_POINT ( 'NONE',  ( 19.71714621942704326, 13.31983420865925005, -12.88265316112568293 ) ) ;
#39167 = CARTESIAN_POINT ( 'NONE',  ( -14.31603901957233660, 19.98981538725089990, 7.500000000000004441 ) ) ;
#39169 = ORIENTED_EDGE ( 'NONE', *, *, #40178, .T. ) ;
#39168 = EDGE_CURVE ( 'NONE', #13732, #31717, #9492, .T. ) ;
#39170 = CARTESIAN_POINT ( 'NONE',  ( -6.146602377671369410, 30.05109521024887798, -14.81031381684638859 ) ) ;
#39171 = EDGE_CURVE ( 'NONE', #21822, #26584, #20298, .T. ) ;
#39172 = EDGE_LOOP ( 'NONE', ( #17236, #39510, #597, #10902, #26595, #33312, #39179, #19560, #23804, #11160, #23733, #32170, #31425, #29772, #13063, #25453, #24216, #7547, #30346, #33204, #36598, #10853, #36382, #15499, #21332, #9195, #18972, #13297, #7061, #23620, #16088, #6178, #910, #29841, #19388, #36638, #12765, #36333, #6527, #18943, #4552, #4557, #34981, #29715, #30127, #249 ) ) ;
#39173 = EDGE_CURVE ( 'NONE', #13029, #9605, #9907, .T. ) ;
#39174 = AXIS2_PLACEMENT_3D ( 'NONE', #8917, #33715, #33113 ) ;
#39175 = CARTESIAN_POINT ( 'NONE',  ( 4.908384188814759241, 36.67470053474868052, 7.102637441331453694 ) ) ;
#39176 = ORIENTED_EDGE ( 'NONE', *, *, #3169, .F. ) ;
#39177 = DIRECTION ( 'NONE',  ( -0.5138379476002908897, 0.6345370204114160195, 0.5773502691896168493 ) ) ;
#39178 = CARTESIAN_POINT ( 'NONE',  ( -1.829593030691901284E-15, 22.50000000000001066, 3.000000000000000000 ) ) ;
#39179 = ORIENTED_EDGE ( 'NONE', *, *, #34849, .F. ) ;
#39180 = CARTESIAN_POINT ( 'NONE',  ( -20.47628691903608811, 0.9865603022909629205, -29.35067870942681267 ) ) ;
#39181 = EDGE_LOOP ( 'NONE', ( #33221, #6710, #31531 ) ) ;
#39182 = CARTESIAN_POINT ( 'NONE',  ( 33.36650818028201826, -11.13369706517688407, -10.22289954697786030 ) ) ;
#39183 = CIRCLE ( 'NONE', #11931, 1.000000000000000888 ) ;
#39184 = ORIENTED_EDGE ( 'NONE', *, *, #14351, .F. ) ;
#39185 = CONTEXT_DEPENDENT_SHAPE_REPRESENTATION ( #33991, #35334 ) ;
#39186 = CARTESIAN_POINT ( 'NONE',  ( -6.354454053420242943, 35.54304081427989814, 11.00000000000000000 ) ) ;
#39187 = ORIENTED_EDGE ( 'NONE', *, *, #11126, .T. ) ;
#39188 = DIRECTION ( 'NONE',  ( -0.5877852522924796874, -0.8090169943749426773, 0.000000000000000000 ) ) ;
#39189 = FACE_OUTER_BOUND ( 'NONE', #46, .T. ) ;
#39190 = ADVANCED_FACE ( 'NONE', ( #11206 ), #39028, .F. ) ;
#39191 = VECTOR ( 'NONE', #21856, 1000.000000000000000 ) ;
#39192 = EDGE_CURVE ( 'NONE', #24994, #19934, #39105, .T. ) ;
#39193 = LINE ( 'NONE', #14617, #9692 ) ;
#39194 = ORIENTED_EDGE ( 'NONE', *, *, #31983, .F. ) ;
#39195 = ADVANCED_FACE ( 'NONE', ( #33354 ), #37798, .T. ) ;
#39196 = CARTESIAN_POINT ( 'NONE',  ( 0.6417673702184640838, 33.31072022568110924, 13.00000000000000178 ) ) ;
#39197 = DIRECTION ( 'NONE',  ( 0.7071067811865451302, 8.659560562354889717E-17, -0.7071067811865500152 ) ) ;
#39198 = CARTESIAN_POINT ( 'NONE',  ( -8.410254037844433483, 17.06698729810786475, 10.00000000000000000 ) ) ;
#39199 = CARTESIAN_POINT ( 'NONE',  ( 15.33041871681650292, 15.00779217446572744, -23.19570158157604567 ) ) ;
#39200 = CARTESIAN_POINT ( 'NONE',  ( 12.31217864997667810, 32.24565435429136073, -7.223754960023913263 ) ) ;
#39201 = CIRCLE ( 'NONE', #283, 0.5000000000000004441 ) ;
#39202 = EDGE_LOOP ( 'NONE', ( #13893, #34733, #15650, #38468 ) ) ;
#39203 = ADVANCED_FACE ( 'NONE', ( #14044 ), #17911, .T. ) ;
#39204 = DIRECTION ( 'NONE',  ( -0.000000000000000000, -0.000000000000000000, -1.000000000000000000 ) ) ;
#39205 = DIRECTION ( 'NONE',  ( 0.9781476007338041345, -0.2079116908177664202, -0.000000000000000000 ) ) ;
#39206 = CARTESIAN_POINT ( 'NONE',  ( 15.68560287515114560, -26.71608784079017340, -6.412881614423534771 ) ) ;
#39207 = DIRECTION ( 'NONE',  ( 1.000000000000000000, 0.000000000000000000, 0.000000000000000000 ) ) ;
#39208 = CARTESIAN_POINT ( 'NONE',  ( -1.829593030691901284E-15, 22.50000000000001066, 23.00000000000000000 ) ) ;
#39209 = CARTESIAN_POINT ( 'NONE',  ( -15.23129526741244533, 26.40958019939556323, -7.827668941241471501 ) ) ;
#39210 = VECTOR ( 'NONE', #8771, 1000.000000000000114 ) ;
#39211 = CARTESIAN_POINT ( 'NONE',  ( -31.72789954390480105, 0.7664678198863910108, 14.53008259254011492 ) ) ;
#39212 = CARTESIAN_POINT ( 'NONE',  ( 13.07091773603987406, -25.33042880074001602, -10.21159384544662885 ) ) ;
#39213 = DIRECTION ( 'NONE',  ( 0.8090169943749426773, -0.5877852522924796874, -0.000000000000000000 ) ) ;
#39214 = ORIENTED_EDGE ( 'NONE', *, *, #5213, .F. ) ;
#39215 = ORIENTED_EDGE ( 'NONE', *, *, #7448, .F. ) ;
#39216 = CARTESIAN_POINT ( 'NONE',  ( -7.928368490687788928, 21.70034315306905981, -22.21406577488186684 ) ) ;
#39217 = CARTESIAN_POINT ( 'NONE',  ( -4.003793317224517700, 8.420815634768723967, 11.00000000000000000 ) ) ;
#39218 = CARTESIAN_POINT ( 'NONE',  ( 3.724371395536106188, 32.23037938972932892, 13.00000000000000178 ) ) ;
#39219 = ADVANCED_FACE ( 'NONE', ( #32550 ), #15738, .T. ) ;
#39220 = AXIS2_PLACEMENT_3D ( 'NONE', #19312, #19923, #28858 ) ;
#39221 = DIRECTION ( 'NONE',  ( 0.000000000000000000, 0.000000000000000000, 1.000000000000000000 ) ) ;
#39222 = ORIENTED_EDGE ( 'NONE', *, *, #31739, .F. ) ;
#39223 = CARTESIAN_POINT ( 'NONE',  ( 30.73050688267034758, 0.03238439121148584815, -6.417084242708104291 ) ) ;
#39224 = DIRECTION ( 'NONE',  ( 1.000000000000000000, 0.000000000000000000, 0.000000000000000000 ) ) ;
#39225 = DIRECTION ( 'NONE',  ( 0.7622652262560051240, -0.2926062055178242916, 0.5773502691896332806 ) ) ;
#39226 = CARTESIAN_POINT ( 'NONE',  ( -36.24879720996644039, -17.94626546700501635, 10.99999999999997691 ) ) ;
#39227 = ORIENTED_EDGE ( 'NONE', *, *, #8892, .T. ) ;
#39228 = CARTESIAN_POINT ( 'NONE',  ( -20.69342229627120133, 0.8482707436503026388, -27.44844477688208073 ) ) ;
#39229 = CARTESIAN_POINT ( 'NONE',  ( 0.000000000000000000, 22.50000000000000355, 7.000000000000000000 ) ) ;
#39230 = ORIENTED_EDGE ( 'NONE', *, *, #37582, .F. ) ;
#39231 = CARTESIAN_POINT ( 'NONE',  ( 28.60017629935383354, -4.227747798920739264, -15.04471679130755390 ) ) ;
#39232 = AXIS2_PLACEMENT_3D ( 'NONE', #38797, #38594, #10768 ) ;
#39233 = CARTESIAN_POINT ( 'NONE',  ( 24.41232237689766293, -27.78610790073912895, 14.53008259254038670 ) ) ;
#39234 = EDGE_LOOP ( 'NONE', ( #25533, #38350 ) ) ;
#39235 = CARTESIAN_POINT ( 'NONE',  ( 15.50248524335058065, 30.73390593357087397, 13.92931973827802317 ) ) ;
#39236 = CARTESIAN_POINT ( 'NONE',  ( 5.531500846456773424, -21.05812563137664739, 19.27171037444156809 ) ) ;
#39237 = DIRECTION ( 'NONE',  ( -0.7431448254773882489, 0.6691306063588648989, 0.000000000000000000 ) ) ;
#39238 = CARTESIAN_POINT ( 'NONE',  ( 3.838817179443445138, 30.80979998870935788, 20.50957957746028981 ) ) ;
#39239 = DIRECTION ( 'NONE',  ( -0.7032331762534054231, 0.07391278520356943382, -0.7071067811865461294 ) ) ;
#39240 = VERTEX_POINT ( 'NONE', #1663 ) ;
#39241 = EDGE_CURVE ( 'NONE', #37722, #751, #26436, .T. ) ;
#39242 = FACE_OUTER_BOUND ( 'NONE', #30484, .T. ) ;
#39243 = DIRECTION ( 'NONE',  ( 1.000000000000000000, 0.000000000000000000, 0.000000000000000000 ) ) ;
#39244 = AXIS2_PLACEMENT_3D ( 'NONE', #28813, #16632, #9732 ) ;
#39245 = CARTESIAN_POINT ( 'NONE',  ( 5.880693269542113910, 30.13551902636890389, -14.80509325191231618 ) ) ;
#39246 = DIRECTION ( 'NONE',  ( -1.224646799147351235E-16, 1.000000000000000000, 0.000000000000000000 ) ) ;
#39247 = CARTESIAN_POINT ( 'NONE',  ( 17.58821720676783329, 10.15456193889309411, 19.66345542862528717 ) ) ;
#39248 = CARTESIAN_POINT ( 'NONE',  ( 13.55783596901029853, -19.12971960218908762, -21.26853342772727729 ) ) ;
#39249 = FACE_OUTER_BOUND ( 'NONE', #7103, .T. ) ;
#39250 = CARTESIAN_POINT ( 'NONE',  ( -13.01373512358517459, 15.56386679242537774, 10.94387467462635577 ) ) ;
#39251 = CARTESIAN_POINT ( 'NONE',  ( 2.596139932171742437, 7.881254734312914678, 10.87262190629281200 ) ) ;
#39252 = ORIENTED_EDGE ( 'NONE', *, *, #34109, .F. ) ;
#39253 = CARTESIAN_POINT ( 'NONE',  ( 14.68930050026369827, 25.54147410505130722, -10.64370694421165453 ) ) ;
#39254 = ORIENTED_EDGE ( 'NONE', *, *, #27474, .F. ) ;
#39255 = TOROIDAL_SURFACE ( 'NONE', #6162, 1.000000000000000000, 0.5000000000000000000 ) ;
#39256 = CARTESIAN_POINT ( 'NONE',  ( -12.30634478552224031, 18.94025476089912985, -21.68721750851181085 ) ) ;
#39257 = AXIS2_PLACEMENT_3D ( 'NONE', #28714, #9834, #25270 ) ;
#39258 = CARTESIAN_POINT ( 'NONE',  ( -30.77008022630320738, -17.76511410164224003, 18.87996532025785257 ) ) ;
#39259 = CARTESIAN_POINT ( 'NONE',  ( -14.45052027064702749, 26.47704597190823606, 10.49999999999999822 ) ) ;
#39260 = CARTESIAN_POINT ( 'NONE',  ( 15.37921949410162981, 26.47433205842913750, -6.888199520723817137 ) ) ;
#39261 = EDGE_LOOP ( 'NONE', ( #26260, #1113, #34909 ) ) ;
#39262 = CARTESIAN_POINT ( 'NONE',  ( 32.39246062267798010, -20.52362622975203266, -6.276506097946584539 ) ) ;
#39263 = ORIENTED_EDGE ( 'NONE', *, *, #7990, .T. ) ;
#39265 = DIRECTION ( 'NONE',  ( 1.000000000000000000, 0.000000000000000000, 0.000000000000000000 ) ) ;
#39264 = CARTESIAN_POINT ( 'NONE',  ( -11.86077688257339524, 20.24129428177698742, -20.48706616378117928 ) ) ;
#39266 = CARTESIAN_POINT ( 'NONE',  ( -11.00841538111624551, -18.87725956289415308, -23.75370681038233656 ) ) ;
#39267 = DIRECTION ( 'NONE',  ( 0.000000000000000000, 0.000000000000000000, -1.000000000000000000 ) ) ;
#39268 = VERTEX_POINT ( 'NONE', #34143 ) ;
#39269 = CARTESIAN_POINT ( 'NONE',  ( -33.61361311049479639, -12.67649022699521311, -9.755067238301116106 ) ) ;
#39270 = CARTESIAN_POINT ( 'NONE',  ( -13.61052633586881555, -24.54839736670113837, -12.56630099801351719 ) ) ;
#39271 = DIRECTION ( 'NONE',  ( 1.000000000000000000, -3.469446951953574746E-15, 0.000000000000000000 ) ) ;
#39272 = ORIENTED_EDGE ( 'NONE', *, *, #4583, .T. ) ;
#39273 = CARTESIAN_POINT ( 'NONE',  ( 28.82737146255313476, 2.000641240079708894, -6.895424389095080819 ) ) ;
#39274 = EDGE_CURVE ( 'NONE', #19973, #2054, #22221, .T. ) ;
#39275 = CARTESIAN_POINT ( 'NONE',  ( -4.527363138135027221, 36.35651410043147536, 7.000000000000000000 ) ) ;
#39276 = DIRECTION ( 'NONE',  ( 0.6459741880212496179, -0.2876062384759507373, 0.7071067811865487940 ) ) ;
#39277 = B_SPLINE_CURVE_WITH_KNOTS ( 'NONE', 3,
 ( #24766, #37162, #18877, #12772, #10132, #3236 ),
 .UNSPECIFIED., .F., .F.,
 ( 4, 2, 4 ),
 ( 0.000000000000000000, 0.5000000000000000000, 1.000000000000000000 ),
 .UNSPECIFIED. ) ;
#39278 = ORIENTED_EDGE ( 'NONE', *, *, #15364, .T. ) ;
#39279 = CARTESIAN_POINT ( 'NONE',  ( -25.26188173616072419, 0.2875138470135812363, -17.42658750387904121 ) ) ;
#39280 = CARTESIAN_POINT ( 'NONE',  ( 20.50011096633554786, 0.05624224123783994750, -30.00000000000000000 ) ) ;
#39281 = CARTESIAN_POINT ( 'NONE',  ( 31.66906069137291624, -9.703676519218381813, 19.27171037444156099 ) ) ;
#39282 = ORIENTED_EDGE ( 'NONE', *, *, #25148, .T. ) ;
#39283 = CARTESIAN_POINT ( 'NONE',  ( -26.72686952400124483, 3.517128624037218820, -10.26466785145276717 ) ) ;
#39284 = EDGE_CURVE ( 'NONE', #342, #25818, #16372, .T. ) ;
#39285 = VECTOR ( 'NONE', #2145, 1000.000000000000000 ) ;
#39286 = FACE_OUTER_BOUND ( 'NONE', #12499, .T. ) ;
#39287 = DIRECTION ( 'NONE',  ( -0.9945218953682740670, -0.1045284632676460046, 0.000000000000000000 ) ) ;
#39288 = AXIS2_PLACEMENT_3D ( 'NONE', #7404, #31994, #25692 ) ;
#39289 = CIRCLE ( 'NONE', #28898, 0.4999999999999995559 ) ;
#39290 = DIRECTION ( 'NONE',  ( 0.000000000000000000, 0.000000000000000000, -1.000000000000000000 ) ) ;
#39291 = CARTESIAN_POINT ( 'NONE',  ( 6.354454053420411697, 35.54304081427980577, 7.000000000000000000 ) ) ;
#39292 = CARTESIAN_POINT ( 'NONE',  ( 7.312035131040564906, 19.41226734497195849, 12.00000000000000000 ) ) ;
#39293 = CARTESIAN_POINT ( 'NONE',  ( -3.503793317224517700, 8.420815634768727520, 9.500000000000000000 ) ) ;
#39294 = ORIENTED_EDGE ( 'NONE', *, *, #39297, .T. ) ;
#39295 = CARTESIAN_POINT ( 'NONE',  ( -26.18615939189180608, 5.309650895087318467, -5.955328271003301310 ) ) ;
#39296 = LINE ( 'NONE', #11474, #33299 ) ;
#39297 = EDGE_CURVE ( 'NONE', #18974, #163, #31093, .T. ) ;
#39298 = CARTESIAN_POINT ( 'NONE',  ( -23.05386822411323422, -7.747535282638357224, 20.99999999999999645 ) ) ;
#39299 = CARTESIAN_POINT ( 'NONE',  ( 25.29206606878849328, -26.20377346906149185, -4.999999999999997335 ) ) ;
#39300 = DIRECTION ( 'NONE',  ( -0.000000000000000000, -0.000000000000000000, -1.000000000000000000 ) ) ;
#39301 = FACE_OUTER_BOUND ( 'NONE', #35429, .T. ) ;
#39302 = CARTESIAN_POINT ( 'NONE',  ( 13.01074387160668522, 22.59504030922215279, -16.39937294696464676 ) ) ;
#39303 = CARTESIAN_POINT ( 'NONE',  ( -10.29072928254728403, -26.28675887230140162, 15.13084544681106536 ) ) ;
#39304 = VERTEX_POINT ( 'NONE', #37384 ) ;
#39305 = CARTESIAN_POINT ( 'NONE',  ( -14.53441762336499998, 17.65377433136575647, -19.82464443782235008 ) ) ;
#39306 = CARTESIAN_POINT ( 'NONE',  ( -18.40750778688453337, -18.65192611823525581, 20.82122704794080548 ) ) ;
#39307 = CARTESIAN_POINT ( 'NONE',  ( 11.80736835487432401, 14.81698729810772619, 7.499999999999997335 ) ) ;
#39308 = CARTESIAN_POINT ( 'NONE',  ( 11.02265137815304108, 17.33746510307418731, -28.70764649880413089 ) ) ;
#39309 = ORIENTED_EDGE ( 'NONE', *, *, #32917, .T. ) ;
#39310 = CARTESIAN_POINT ( 'NONE',  ( 11.03878455726504093, 17.42581041319598611, -28.07733810068037528 ) ) ;
#39311 = ORIENTED_EDGE ( 'NONE', *, *, #36498, .F. ) ;
#39312 = AXIS2_PLACEMENT_3D ( 'NONE', #21223, #12471, #21812 ) ;
#39314 = DIRECTION ( 'NONE',  ( 1.000000000000000000, -6.938893903907174735E-15, 0.000000000000000000 ) ) ;
#39313 = CARTESIAN_POINT ( 'NONE',  ( -15.13066917251539145, 26.42877163258943796, -8.292150810359242286 ) ) ;
#39315 = CARTESIAN_POINT ( 'NONE',  ( -13.73555582509986728, -24.12058157067978570, -13.51135623849643075 ) ) ;
#39316 = CARTESIAN_POINT ( 'NONE',  ( -28.21696687770289813, -27.03935558029874286, 12.14047268033091598 ) ) ;
#39317 = AXIS2_PLACEMENT_3D ( 'NONE', #7258, #33771, #29006 ) ;
#39318 = AXIS2_PLACEMENT_3D ( 'NONE', #12332, #37120, #37317 ) ;
#39319 = CARTESIAN_POINT ( 'NONE',  ( -17.86905274512871244, -10.06606982860865607, -30.00000000000002132 ) ) ;
#39320 = CARTESIAN_POINT ( 'NONE',  ( -4.698712440877560681, -19.95451542538867784, -30.00000000000000355 ) ) ;
#39321 = CARTESIAN_POINT ( 'NONE',  ( 5.238409041734346516, 36.41108174777518514, 10.49999999999999822 ) ) ;
#39322 = CARTESIAN_POINT ( 'NONE',  ( 11.69146759026597238, 16.83997637742415776, -30.00000000000000000 ) ) ;
#39323 = VERTEX_POINT ( 'NONE', #39824 ) ;
#39324 = CARTESIAN_POINT ( 'NONE',  ( 20.53763572180891828, 6.763609892796464074, -22.15629058788150729 ) ) ;
#39325 = CIRCLE ( 'NONE', #31543, 0.5000000000000004441 ) ;
#39326 = ADVANCED_FACE ( 'NONE', ( #36585 ), #15649, .F. ) ;
#39327 = DIRECTION ( 'NONE',  ( 0.2876062384759419666, -0.6459741880212652720, -0.7071067811865382469 ) ) ;
#39328 = CARTESIAN_POINT ( 'NONE',  ( 8.238488885696289898, 24.65111619403943877, 9.000000000000001776 ) ) ;
#39329 = CARTESIAN_POINT ( 'NONE',  ( 0.000000000000000000, 22.50000000000000355, 12.00000000000000000 ) ) ;
#39330 = VERTEX_POINT ( 'NONE', #33939 ) ;
#39331 = CARTESIAN_POINT ( 'NONE',  ( -22.44886821189929904, -0.3562293043217420463, -22.60475047268272775 ) ) ;
#39332 = CARTESIAN_POINT ( 'NONE',  ( 27.25673043994063960, 0.07488738648532623776, -14.45827337014668679 ) ) ;
#39333 = CYLINDRICAL_SURFACE ( 'NONE', #13112, 62.00000000000001421 ) ;
#39334 = CARTESIAN_POINT ( 'NONE',  ( 17.83459896181130944, -17.64923967996766052, 20.94377226548378701 ) ) ;
#39335 = CARTESIAN_POINT ( 'NONE',  ( -14.47283171447380212, 21.48159823030330884, 9.500000000000000000 ) ) ;
#39336 = EDGE_CURVE ( 'NONE', #22956, #34728, #24391, .T. ) ;
#39337 = CARTESIAN_POINT ( 'NONE',  ( -5.688306800005769048, 28.52217545723006609, 13.00000000000000178 ) ) ;
#39338 = CARTESIAN_POINT ( 'NONE',  ( 36.74707368630886606, -16.71203845619553974, 10.99999999999982769 ) ) ;
#39339 = EDGE_LOOP ( 'NONE', ( #9851, #1036, #39850, #39709 ) ) ;
#39340 = CARTESIAN_POINT ( 'NONE',  ( -14.64211604268330902, 20.79918788657763429, 12.00000000000000000 ) ) ;
#39341 = CIRCLE ( 'NONE', #4311, 0.5000000000000004441 ) ;
#39342 = DIRECTION ( 'NONE',  ( 0.000000000000000000, 0.000000000000000000, 1.000000000000000000 ) ) ;
#39343 = DIRECTION ( 'NONE',  ( -1.000000000000000000, 0.000000000000000000, 0.000000000000000000 ) ) ;
#39344 = CARTESIAN_POINT ( 'NONE',  ( 0.3901599449075797699, 36.15865306409283875, -10.17303319637575676 ) ) ;
#39345 = CARTESIAN_POINT ( 'NONE',  ( -5.524694096546769018, 36.45979188825334916, 10.49999999999999645 ) ) ;
#39346 = AXIS2_PLACEMENT_3D ( 'NONE', #37858, #31563, #12678 ) ;
#39347 = EDGE_CURVE ( 'NONE', #38300, #20973, #15104, .T. ) ;
#39348 = DIRECTION ( 'NONE',  ( -0.3090169943749573322, -0.9510565162951505336, 0.000000000000000000 ) ) ;
#39349 = ADVANCED_FACE ( 'NONE', ( #12598 ), #21145, .T. ) ;
#39350 = DIRECTION ( 'NONE',  ( 1.000000000000000000, 0.000000000000000000, 0.000000000000000000 ) ) ;
#39351 = DIRECTION ( 'NONE',  ( 0.000000000000000000, -0.7071067811865451302, 0.7071067811865500152 ) ) ;
#39352 = CARTESIAN_POINT ( 'NONE',  ( -2.525645716490710679, 8.212903943950959018, 7.000000000000000000 ) ) ;
#39353 = DIRECTION ( 'NONE',  ( 1.000000000000000000, 0.000000000000000000, 0.000000000000000000 ) ) ;
#39354 = CARTESIAN_POINT ( 'NONE',  ( 9.943094648483580045, 18.21399347630012144, -27.36083611208444566 ) ) ;
#39355 = DIRECTION ( 'NONE',  ( 0.1045284632676569680, 0.9945218953682730678, 0.000000000000000000 ) ) ;
#39356 = VERTEX_POINT ( 'NONE', #18304 ) ;
#39358 = CARTESIAN_POINT ( 'NONE',  ( -13.97557076678966403, 21.53386246193713305, 10.00000000000000000 ) ) ;
#39357 = CARTESIAN_POINT ( 'NONE',  ( -17.07654005633402150, 13.06277261991058580, -22.21483479645549153 ) ) ;
#39359 = DIRECTION ( 'NONE',  ( -0.6459741880212467313, 0.2876062384759635604, 0.7071067811865462405 ) ) ;
#39360 = CARTESIAN_POINT ( 'NONE',  ( 15.28437775947960908, -26.40254534672767406, -7.826725057383953299 ) ) ;
#39361 = PLANE ( 'NONE',  #33446 ) ;
#39362 = CARTESIAN_POINT ( 'NONE',  ( 11.01243325502136372, 17.44311777400445607, -28.07576541037593287 ) ) ;
#39363 = LINE ( 'NONE', #39760, #22426 ) ;
#39364 = CARTESIAN_POINT ( 'NONE',  ( 14.36830325120613772, 20.48707633493483371, 9.500000000000000000 ) ) ;
#39365 = CARTESIAN_POINT ( 'NONE',  ( -29.58504087036580188, -23.16551093242282278, -7.131814702964139663 ) ) ;
#39366 = CARTESIAN_POINT ( 'NONE',  ( 2.775580681383440051, -20.45610540486786277, -27.72389806004756352 ) ) ;
#39367 = CARTESIAN_POINT ( 'NONE',  ( 14.15536964391180241, 23.64370951135699173, -13.52742165616817438 ) ) ;
#39368 = CARTESIAN_POINT ( 'NONE',  ( 21.31969949502798656, 11.87203962839359761, -9.396023366860072557 ) ) ;
#39369 = DIRECTION ( 'NONE',  ( 0.000000000000000000, 0.000000000000000000, 1.000000000000000000 ) ) ;
#39370 = ORIENTED_EDGE ( 'NONE', *, *, #28199, .T. ) ;
#39371 = CARTESIAN_POINT ( 'NONE',  ( -4.242919837288198437, 20.95646936440089547, -25.66960880586146843 ) ) ;
#39372 = ORIENTED_EDGE ( 'NONE', *, *, #5751, .T. ) ;
#39373 = EDGE_CURVE ( 'NONE', #2857, #37653, #5900, .T. ) ;
#39374 = VECTOR ( 'NONE', #21437, 1000.000000000000000 ) ;
#39375 = CIRCLE ( 'NONE', #21845, 21.00000000000001776 ) ;
#39376 = CARTESIAN_POINT ( 'NONE',  ( -17.61963632530846979, 22.05541241832616706, 15.13084544681368548 ) ) ;
#39377 = ORIENTED_EDGE ( 'NONE', *, *, #37595, .F. ) ;
#39378 = DIRECTION ( 'NONE',  ( -0.000000000000000000, -0.000000000000000000, -1.000000000000000000 ) ) ;
#39379 = CARTESIAN_POINT ( 'NONE',  ( 2.672146553953312687, 12.33340603770390942, 10.00000000000000000 ) ) ;
#39380 = VERTEX_POINT ( 'NONE', #18896 ) ;
#39381 = CARTESIAN_POINT ( 'NONE',  ( -23.87967171433753677, 0.6314381994875827298, -19.51309412989072456 ) ) ;
#39382 = CARTESIAN_POINT ( 'NONE',  ( 35.24497909167011045, -11.81349549158436041, -6.720739232717652278 ) ) ;
#39383 = ORIENTED_EDGE ( 'NONE', *, *, #9410, .T. ) ;
#39384 = DIRECTION ( 'NONE',  ( 0.4999999999999921174, -0.8660254037844431485, -0.000000000000000000 ) ) ;
#39385 = ORIENTED_EDGE ( 'NONE', *, *, #13497, .T. ) ;
#39386 = DIRECTION ( 'NONE',  ( -1.000000000000000000, 0.000000000000000000, 0.000000000000000000 ) ) ;
#39387 = CARTESIAN_POINT ( 'NONE',  ( -4.211402178667006169, 32.38366924255629442, 6.000000000000000000 ) ) ;
#39388 = DIRECTION ( 'NONE',  ( -0.4446959099295410001, 0.6847716512521619947, 0.5773502691896187367 ) ) ;
#39389 = ORIENTED_EDGE ( 'NONE', *, *, #11235, .T. ) ;
#39390 = CARTESIAN_POINT ( 'NONE',  ( -5.644276917315534270, 36.40655018617698602, 10.49999999999999822 ) ) ;
#39391 = LINE ( 'NONE', #17683, #7210 ) ;
#39392 = CARTESIAN_POINT ( 'NONE',  ( -4.444496572746359675, 24.85486536600718921, 23.00000000000000711 ) ) ;
#39393 = EDGE_CURVE ( 'NONE', #38482, #27384, #10496, .T. ) ;
#39394 = CARTESIAN_POINT ( 'NONE',  ( 15.80417486761067813, 13.15001486149802901, -28.27561554616373130 ) ) ;
#39395 = AXIS2_PLACEMENT_3D ( 'NONE', #29080, #850, #3891 ) ;
#39396 = CARTESIAN_POINT ( 'NONE',  ( 10.38712762836738790, 29.35899506542313731, -13.09421097062898376 ) ) ;
#39397 = ORIENTED_EDGE ( 'NONE', *, *, #18809, .T. ) ;
#39398 = CARTESIAN_POINT ( 'NONE',  ( -21.39046744509776232, 10.41410512707694558, -12.88491266128117196 ) ) ;
#39399 = CARTESIAN_POINT ( 'NONE',  ( 0.3582258883630317636, 11.68927977431952137, 13.00000000000000178 ) ) ;
#39400 = DIRECTION ( 'NONE',  ( -1.000000000000000000, 0.000000000000000000, 0.000000000000000000 ) ) ;
#39401 = CARTESIAN_POINT ( 'NONE',  ( 14.16828251099090608, -24.17632410410987021, -13.47354249254208192 ) ) ;
#39402 = FACE_OUTER_BOUND ( 'NONE', #11491, .T. ) ;
#39403 = AXIS2_PLACEMENT_3D ( 'NONE', #9854, #13493, #13088 ) ;
#39404 = CARTESIAN_POINT ( 'NONE',  ( 23.06249103411542478, 13.31513540672987972, -13.39439507595155199 ) ) ;
#39405 = VECTOR ( 'NONE', #9272, 1000.000000000000000 ) ;
#39406 = CARTESIAN_POINT ( 'NONE',  ( -11.17299096545415793, 17.76456080679757932, -26.22365104219313992 ) ) ;
#39407 = CARTESIAN_POINT ( 'NONE',  ( -13.25611089641869000, -15.90730867704575857, -27.86709263596938158 ) ) ;
#39408 = CARTESIAN_POINT ( 'NONE',  ( 10.01790345176820374, -20.67646280627521804, -20.67097678944346484 ) ) ;
#39409 = FACE_OUTER_BOUND ( 'NONE', #34414, .T. ) ;
#39410 = ORIENTED_EDGE ( 'NONE', *, *, #15603, .T. ) ;
#39411 = VERTEX_POINT ( 'NONE', #12396 ) ;
#39412 = CARTESIAN_POINT ( 'NONE',  ( -12.11690442435413217, 30.76865878555264544, -9.918238614674569575 ) ) ;
#39413 = CYLINDRICAL_SURFACE ( 'NONE', #25634, 0.5000000000000004441 ) ;
#39414 = ADVANCED_FACE ( 'NONE', ( #33552 ), #9356, .F. ) ;
#39415 = CARTESIAN_POINT ( 'NONE',  ( -12.14063985594382800, 14.34296697341692095, 10.49999999999999822 ) ) ;
#39416 = DIRECTION ( 'NONE',  ( -0.000000000000000000, -0.000000000000000000, -1.000000000000000000 ) ) ;
#39417 = EDGE_LOOP ( 'NONE', ( #36027, #3592, #21105, #40054, #22613, #28659 ) ) ;
#39418 = CARTESIAN_POINT ( 'NONE',  ( 30.83880836401509029, 0.02450782886024078025, -4.999999999999999112 ) ) ;
#39419 = EDGE_CURVE ( 'NONE', #37722, #7787, #24785, .T. ) ;
#39420 = CARTESIAN_POINT ( 'NONE',  ( 10.81260707898150386, 32.90853150812155548, 11.00000000000000000 ) ) ;
#39421 = CARTESIAN_POINT ( 'NONE',  ( -3.587667106213709101, 35.31811204475769728, 6.000000000000000000 ) ) ;
#39422 = CARTESIAN_POINT ( 'NONE',  ( -2.629601561899593598, 7.723830143584060615, 10.49999999999999112 ) ) ;
#39423 = VERTEX_POINT ( 'NONE', #27638 ) ;
#39424 = CARTESIAN_POINT ( 'NONE',  ( -30.89051437471967887, -0.02824647624105830826, -4.999999999999999112 ) ) ;
#39425 = CARTESIAN_POINT ( 'NONE',  ( -12.05736835487443237, 14.38397459621567442, 10.50000000000000000 ) ) ;
#39426 = ORIENTED_EDGE ( 'NONE', *, *, #3200, .F. ) ;
#39427 = CARTESIAN_POINT ( 'NONE',  ( 20.30048362414427743, -2.857582090605152558, -29.28181927125163853 ) ) ;
#39428 = AXIS2_PLACEMENT_3D ( 'NONE', #31088, #3051, #5897 ) ;
#39429 = AXIS2_PLACEMENT_3D ( 'NONE', #24682, #37078, #21436 ) ;
#39430 = ADVANCED_FACE ( 'NONE', ( #6293 ), #24189, .F. ) ;
#39431 = CARTESIAN_POINT ( 'NONE',  ( 15.07283634909883929, -28.35394831540531158, 13.32518128616608877 ) ) ;
#39432 = ORIENTED_EDGE ( 'NONE', *, *, #33257, .F. ) ;
#39433 = CARTESIAN_POINT ( 'NONE',  ( -14.44241962112810285, 32.29667252612950534, 13.92931973827808889 ) ) ;
#39434 = AXIS2_PLACEMENT_3D ( 'NONE', #1619, #27002, #38787 ) ;
#39435 = CARTESIAN_POINT ( 'NONE',  ( -18.03924190088443424, -16.85603499720474119, 20.99999999999999645 ) ) ;
#39436 = CARTESIAN_POINT ( 'NONE',  ( -32.33143948542088708, 1.358872982498823268, -5.000000000000000888 ) ) ;
#39437 = CARTESIAN_POINT ( 'NONE',  ( -6.154269285972598702, 26.67460248448161764, 20.82122704794079837 ) ) ;
#39438 = CIRCLE ( 'NONE', #38776, 1.000000000000000000 ) ;
#39439 = CARTESIAN_POINT ( 'NONE',  ( 8.559505275947156377, 25.28115294937476065, 13.00000000000000178 ) ) ;
#39440 = EDGE_LOOP ( 'NONE', ( #11414, #4750, #10959 ) ) ;
#39441 = DIRECTION ( 'NONE',  ( -0.7032331762534090869, 0.07391278520354985226, -0.7071067811865444641 ) ) ;
#39442 = CARTESIAN_POINT ( 'NONE',  ( 11.41267482483262619, 26.20820393249957192, 6.000000000000000000 ) ) ;
#39443 = EDGE_CURVE ( 'NONE', #3967, #24813, #21936, .T. ) ;
#39444 = EDGE_CURVE ( 'NONE', #4676, #15434, #2465, .T. ) ;
#39445 = CARTESIAN_POINT ( 'NONE',  ( 6.820427054864983241, 34.96104138684941631, -9.769343582562422412 ) ) ;
#39446 = DIRECTION ( 'NONE',  ( 0.000000000000000000, 0.000000000000000000, 1.000000000000000000 ) ) ;
#39447 = CARTESIAN_POINT ( 'NONE',  ( 10.32110568910150228, 19.34973993754613986, 20.50957957746029336 ) ) ;
#39448 = CARTESIAN_POINT ( 'NONE',  ( 18.61788257364777266, -27.16959213022483510, -6.373035692954665876 ) ) ;
#39449 = DIRECTION ( 'NONE',  ( 0.9781476007338042455, -0.2079116908177663092, 0.000000000000000000 ) ) ;
#39450 = DIRECTION ( 'NONE',  ( 0.000000000000000000, 0.000000000000000000, 1.000000000000000000 ) ) ;
#39451 = DIRECTION ( 'NONE',  ( -0.9135454576426005335, 0.4067366430758008744, -0.000000000000000000 ) ) ;
#39452 = ORIENTED_EDGE ( 'NONE', *, *, #17127, .T. ) ;
#39453 = CARTESIAN_POINT ( 'NONE',  ( 11.62397448804718536, 18.97120798431754096, -22.72432224387674538 ) ) ;
#39454 = CIRCLE ( 'NONE', #21308, 18.00000000000000000 ) ;
#39455 = ORIENTED_EDGE ( 'NONE', *, *, #38814, .T. ) ;
#39457 = VECTOR ( 'NONE', #39074, 1000.000000000000000 ) ;
#39456 = CARTESIAN_POINT ( 'NONE',  ( -15.13210240647062399, 25.19633130894646911, -9.718349095871507970 ) ) ;
#39458 = CARTESIAN_POINT ( 'NONE',  ( -32.53782915839244083, -12.43926102483660578, 18.87996532025785967 ) ) ;
#39459 = CARTESIAN_POINT ( 'NONE',  ( -3.938766756526925761, 8.166638875703812417, 10.49999999999999822 ) ) ;
#39460 = CARTESIAN_POINT ( 'NONE',  ( 15.46782449521607283, 26.59794325776330481, -4.999999999999998224 ) ) ;
#39461 = ORIENTED_EDGE ( 'NONE', *, *, #2345, .T. ) ;
#39462 = CARTESIAN_POINT ( 'NONE',  ( 30.86005551239754396, -19.56640338714962013, -9.726560286790116194 ) ) ;
#39463 = ORIENTED_EDGE ( 'NONE', *, *, #39641, .F. ) ;
#39464 = CIRCLE ( 'NONE', #552, 1.000000000000002665 ) ;
#39466 = DIRECTION ( 'NONE',  ( 0.000000000000000000, 0.000000000000000000, 1.000000000000000000 ) ) ;
#39465 = CARTESIAN_POINT ( 'NONE',  ( -13.55369973957343532, 23.86660515378133240, -14.42750371290488154 ) ) ;
#39467 = B_SPLINE_CURVE_WITH_KNOTS ( 'NONE', 3,
 ( #40087, #11867, #8619, #3315 ),
 .UNSPECIFIED., .F., .F.,
 ( 4, 4 ),
 ( 0.0006014480309583149914, 0.0009453384547274258469 ),
 .UNSPECIFIED. ) ;
#39468 = CARTESIAN_POINT ( 'NONE',  ( -16.00326414221997240, -25.30023022726772552, -11.48905281562103653 ) ) ;
#39469 = ADVANCED_FACE ( 'NONE', ( #5699 ), #3405, .T. ) ;
#39470 = CARTESIAN_POINT ( 'NONE',  ( -6.557822374958137246, 35.99981354310120452, 7.000000000000000000 ) ) ;
#39471 = VECTOR ( 'NONE', #24387, 1000.000000000000114 ) ;
#39472 = ORIENTED_EDGE ( 'NONE', *, *, #28400, .T. ) ;
#39473 = CARTESIAN_POINT ( 'NONE',  ( -35.49576857290053766, -12.23958519446773785, -5.000000000000004441 ) ) ;
#39474 = CARTESIAN_POINT ( 'NONE',  ( -13.09227930551162444, -23.59843141973120595, -14.49164938364699751 ) ) ;
#39475 = CARTESIAN_POINT ( 'NONE',  ( 16.58691282011993806, -31.15705289668494871, 22.99999999999905853 ) ) ;
#39476 = ORIENTED_EDGE ( 'NONE', *, *, #26148, .T. ) ;
#39477 = CARTESIAN_POINT ( 'NONE',  ( 25.86870765427833163, 2.101442506354480599, -14.59862430777500464 ) ) ;
#39478 = EDGE_CURVE ( 'NONE', #32551, #2390, #827, .T. ) ;
#39479 = CARTESIAN_POINT ( 'NONE',  ( -8.317671217786068993, 10.20105690706398249, 10.87262190629279601 ) ) ;
#39480 = CARTESIAN_POINT ( 'NONE',  ( 3.607749162633204332, 7.931741834401770497, 7.000000000000000000 ) ) ;
#39481 = VERTEX_POINT ( 'NONE', #10353 ) ;
#39482 = CARTESIAN_POINT ( 'NONE',  ( -20.52994536750384214, 0.7932886217482892910, -28.70470255602677057 ) ) ;
#39483 = ORIENTED_EDGE ( 'NONE', *, *, #23415, .T. ) ;
#39484 = CARTESIAN_POINT ( 'NONE',  ( 20.54983429119329941, 0.05123126462676740045, -28.67845366199332346 ) ) ;
#39485 = CARTESIAN_POINT ( 'NONE',  ( 29.31960910815444521, -5.098408205982018160, 19.66345542862562468 ) ) ;
#39486 = VERTEX_POINT ( 'NONE', #9756 ) ;
#39487 = CARTESIAN_POINT ( 'NONE',  ( -26.89440075162845289, 4.411995506115219179, -5.952929326054199777 ) ) ;
#39488 = CARTESIAN_POINT ( 'NONE',  ( 2.118671991557230516, 37.17221401100731981, 12.00000000000000000 ) ) ;
#39489 = LINE ( 'NONE', #26898, #10254 ) ;
#39490 = AXIS2_PLACEMENT_3D ( 'NONE', #31072, #6472, #3831 ) ;
#39491 = AXIS2_PLACEMENT_3D ( 'NONE', #26364, #38757, #22307 ) ;
#39492 = DIRECTION ( 'NONE',  ( -0.000000000000000000, 0.000000000000000000, -1.000000000000000000 ) ) ;
#39493 = CARTESIAN_POINT ( 'NONE',  ( -12.14717575287011719, 32.53695909538323860, 13.00000000000000178 ) ) ;
#39494 = FACE_BOUND ( 'NONE', #31881, .T. ) ;
#39495 = CARTESIAN_POINT ( 'NONE',  ( 0.5000000000000035527, 32.50000000000000000, 10.50000000000000178 ) ) ;
#39496 = ORIENTED_EDGE ( 'NONE', *, *, #17005, .F. ) ;
#39497 = CARTESIAN_POINT ( 'NONE',  ( -20.05673146015622521, 4.300176513202893958, -29.99999999999999645 ) ) ;
#39498 = CARTESIAN_POINT ( 'NONE',  ( -13.63581098909220479, 27.45627467658446008, 7.499999999999993783 ) ) ;
#39499 = DIRECTION ( 'NONE',  ( -0.000000000000000000, -0.000000000000000000, -1.000000000000000000 ) ) ;
#39500 = CARTESIAN_POINT ( 'NONE',  ( 14.90381431695064585, -14.60044926573648283, -27.07745846674980683 ) ) ;
#39501 = ADVANCED_FACE ( 'NONE', ( #13392 ), #19287, .T. ) ;
#39502 = DIRECTION ( 'NONE',  ( 1.000000000000000000, 0.000000000000000000, 0.000000000000000000 ) ) ;
#39503 = CARTESIAN_POINT ( 'NONE',  ( 12.16824354003327535, 20.78390325353091228, -19.44999157952565128 ) ) ;
#39504 = CARTESIAN_POINT ( 'NONE',  ( -15.07283634909299685, -28.35394831540364180, 13.32518128616608877 ) ) ;
#39505 = ORIENTED_EDGE ( 'NONE', *, *, #30647, .F. ) ;
#39506 = CARTESIAN_POINT ( 'NONE',  ( -16.44063469669066535, 22.69260288965874750, -7.852988990058472396 ) ) ;
#39507 = CARTESIAN_POINT ( 'NONE',  ( -27.58732789242640138, -12.88115193908558354, 20.69868183039781329 ) ) ;
#39508 = CARTESIAN_POINT ( 'NONE',  ( -13.94482798346716201, 26.50521816028930999, 7.000000000000000000 ) ) ;
#39509 = CARTESIAN_POINT ( 'NONE',  ( 15.11779573149777178, 26.08460211011391294, -8.768163045224820706 ) ) ;
#39510 = ORIENTED_EDGE ( 'NONE', *, *, #9465, .F. ) ;
#39511 = CARTESIAN_POINT ( 'NONE',  ( 12.65336495216310553, 21.05333586549351921, -18.45227026116430125 ) ) ;
#39512 = VERTEX_POINT ( 'NONE', #3853 ) ;
#39514 = CARTESIAN_POINT ( 'NONE',  ( -11.14717575287011542, 32.53695909538323860, 13.00000000000000178 ) ) ;
#39513 = CARTESIAN_POINT ( 'NONE',  ( -15.23016191995029445, 26.73636172458780180, -7.352086281858299266 ) ) ;
#39515 = CARTESIAN_POINT ( 'NONE',  ( -10.58818753192410966, -19.56084638205915027, -22.72817583048230006 ) ) ;
#39516 = LINE ( 'NONE', #5586, #11461 ) ;
#39517 = AXIS2_PLACEMENT_3D ( 'NONE', #11343, #27180, #39565 ) ;
#39518 = VECTOR ( 'NONE', #18231, 999.9999999999998863 ) ;
#39519 = CARTESIAN_POINT ( 'NONE',  ( -32.68238800772844144, -18.40062344110566883, -8.403867360342845316 ) ) ;
#39520 = CARTESIAN_POINT ( 'NONE',  ( -10.79967333563281429, -24.51318330059240935, -11.70098447834189059 ) ) ;
#39521 = DIRECTION ( 'NONE',  ( 0.9510565162951544194, 0.3090169943749449533, -0.000000000000000000 ) ) ;
#39522 = CARTESIAN_POINT ( 'NONE',  ( 12.40075146136572215, 17.14821721898418261, -25.15186329211611493 ) ) ;
#39523 = ORIENTED_EDGE ( 'NONE', *, *, #27694, .T. ) ;
#39524 = CARTESIAN_POINT ( 'NONE',  ( 21.85184851404966366, 6.109037027396825081, -18.92964341907457637 ) ) ;
#39525 = DIRECTION ( 'NONE',  ( -0.6123724356957955806, 0.3535533905932792820, -0.7071067811865437980 ) ) ;
#39526 = DIRECTION ( 'NONE',  ( 0.000000000000000000, 0.000000000000000000, 1.000000000000000000 ) ) ;
#39527 = DIRECTION ( 'NONE',  ( -0.000000000000000000, -0.000000000000000000, -1.000000000000000000 ) ) ;
#39528 = AXIS2_PLACEMENT_3D ( 'NONE', #33518, #39388, #38993 ) ;
#39529 = EDGE_LOOP ( 'NONE', ( #14481, #3892, #37823 ) ) ;
#39530 = CARTESIAN_POINT ( 'NONE',  ( -31.67541566499863137, -1.212671030267491457, -7.318079979765841792 ) ) ;
#39531 = CARTESIAN_POINT ( 'NONE',  ( 29.86521059342267037, -0.02516630548550341170, -9.704683626496786175 ) ) ;
#39532 = DIRECTION ( 'NONE',  ( 1.000000000000000000, 0.000000000000000000, 0.000000000000000000 ) ) ;
#39533 = CARTESIAN_POINT ( 'NONE',  ( 25.22909892406947918, -10.52103384677014120, 20.99999999999999645 ) ) ;
#39534 = ADVANCED_FACE ( 'NONE', ( #28834 ), #15849, .F. ) ;
#39535 = DIRECTION ( 'NONE',  ( 1.000000000000000000, 0.000000000000000000, 0.000000000000000000 ) ) ;
#39536 = DIRECTION ( 'NONE',  ( 0.000000000000000000, 0.000000000000000000, 1.000000000000000000 ) ) ;
#39537 = VERTEX_POINT ( 'NONE', #31682 ) ;
#39538 = CARTESIAN_POINT ( 'NONE',  ( 14.98522546127354182, 21.83078073962648347, 7.382773698552468566 ) ) ;
#39539 = B_SPLINE_CURVE_WITH_KNOTS ( 'NONE', 3,
 ( #2579, #27351, #39739, #18812, #12312, #12508 ),
 .UNSPECIFIED., .F., .F.,
 ( 4, 1, 1, 4 ),
 ( 0.000000000000000000, 0.1250000000429448144, 0.2500000000286252688, 0.3034822677883343145 ),
 .UNSPECIFIED. ) ;
#39540 = CIRCLE ( 'NONE', #4516, 1.000000000000000000 ) ;
#39541 = FACE_OUTER_BOUND ( 'NONE', #35716, .T. ) ;
#39542 = EDGE_LOOP ( 'NONE', ( #16043, #27425, #19873, #35736 ) ) ;
#39543 = CARTESIAN_POINT ( 'NONE',  ( 1.576739634193315531, 38.46478598617967748, -5.435507960873805722 ) ) ;
#39544 = DIRECTION ( 'NONE',  ( 0.000000000000000000, 0.000000000000000000, 1.000000000000000000 ) ) ;
#39545 = EDGE_CURVE ( 'NONE', #10050, #31776, #16250, .T. ) ;
#39546 = CARTESIAN_POINT ( 'NONE',  ( -13.24038105676664401, 15.43301270189234486, 10.49999999999999822 ) ) ;
#39547 = CARTESIAN_POINT ( 'NONE',  ( 21.39877161664088590, 15.54711762656346075, 7.000000000000000000 ) ) ;
#39548 = CONICAL_SURFACE ( 'NONE', #19418, 0.9999999999999970024, 0.7853981633974552734 ) ;
#39549 = CARTESIAN_POINT ( 'NONE',  ( -11.14717575287011542, 32.53695909538323860, 6.000000000000000000 ) ) ;
#39550 = DIRECTION ( 'NONE',  ( 1.000000000000000000, 0.000000000000000000, 0.000000000000000000 ) ) ;
#39551 = CYLINDRICAL_SURFACE ( 'NONE', #8694, 0.4999999999999999445 ) ;
#39552 = CARTESIAN_POINT ( 'NONE',  ( 10.64953201439048591, 19.84495155912917852, -22.56251018198367220 ) ) ;
#39553 = CARTESIAN_POINT ( 'NONE',  ( 9.581182426140127717, 10.95854901866634812, 7.339470489435492517 ) ) ;
#39554 = VERTEX_POINT ( 'NONE', #37779 ) ;
#39556 = LINE ( 'NONE', #30224, #25215 ) ;
#39555 = CARTESIAN_POINT ( 'NONE',  ( -16.01363482889661682, 13.06226528883478721, -27.14623243372550832 ) ) ;
#39557 = EDGE_CURVE ( 'NONE', #29202, #13434, #34536, .T. ) ;
#39558 = CARTESIAN_POINT ( 'NONE',  ( 13.24038105676654986, 15.43301270189216368, 10.49999999999999822 ) ) ;
#39559 = CARTESIAN_POINT ( 'NONE',  ( 14.97993852148964145, -25.99036409581853846, -9.238322188113263778 ) ) ;
#39560 = EDGE_CURVE ( 'NONE', #27233, #10152, #7287, .T. ) ;
#39561 = CARTESIAN_POINT ( 'NONE',  ( 30.57450045108191006, -0.3656520783221838267, 16.87380292611441490 ) ) ;
#39562 = CARTESIAN_POINT ( 'NONE',  ( 15.16414560994073035, 26.31667483029525556, -8.296495527103925127 ) ) ;
#39563 = ORIENTED_EDGE ( 'NONE', *, *, #6413, .F. ) ;
#39564 = CARTESIAN_POINT ( 'NONE',  ( 11.10756861982301125, 19.59949212537556562, -20.90349153980999475 ) ) ;
#39565 = DIRECTION ( 'NONE',  ( -1.000000000000000000, 0.000000000000000000, 0.000000000000000000 ) ) ;
#39566 = CARTESIAN_POINT ( 'NONE',  ( -17.31219681121567788, -13.52410775897827477, -24.27504181234872505 ) ) ;
#39567 = CARTESIAN_POINT ( 'NONE',  ( 4.011976552904903848, -24.82011946043718353, -6.449216445830162847 ) ) ;
#39568 = CARTESIAN_POINT ( 'NONE',  ( 13.43547369680725012, 21.83571133183076540, -16.47867356606642986 ) ) ;
#39569 = CARTESIAN_POINT ( 'NONE',  ( 21.54236824818556073, 11.99210819226683711, -7.428645542648590450 ) ) ;
#39570 = FACE_OUTER_BOUND ( 'NONE', #41, .T. ) ;
#39571 = B_SPLINE_CURVE_WITH_KNOTS ( 'NONE', 3,
 ( #21662, #34066, #18629, #3184 ),
 .UNSPECIFIED., .F., .F.,
 ( 4, 4 ),
 ( 0.000000000000000000, 1.000000000000000000 ),
 .UNSPECIFIED. ) ;
#39572 = CARTESIAN_POINT ( 'NONE',  ( -4.142698204329950507, 24.13178648764145606, -20.78291476969486951 ) ) ;
#39573 = EDGE_LOOP ( 'NONE', ( #17007, #17364, #3058, #32162 ) ) ;
#39574 = AXIS2_PLACEMENT_3D ( 'NONE', #26209, #36364, #32723 ) ;
#39575 = CARTESIAN_POINT ( 'NONE',  ( -28.79337657216576574, 4.963436916929316212, 11.55979286844546472 ) ) ;
#39576 = ORIENTED_EDGE ( 'NONE', *, *, #10569, .T. ) ;
#39577 = FACE_OUTER_BOUND ( 'NONE', #6262, .T. ) ;
#39578 = ADVANCED_FACE ( 'NONE', ( #31288 ), #31883, .F. ) ;
#39579 = CARTESIAN_POINT ( 'NONE',  ( 0.3582258883630317636, 11.68927977431952137, 6.000000000000000000 ) ) ;
#39580 = EDGE_CURVE ( 'NONE', #32493, #7288, #26755, .T. ) ;
#39581 = AXIS2_PLACEMENT_3D ( 'NONE', #26601, #23359, #17478 ) ;
#39582 = CARTESIAN_POINT ( 'NONE',  ( -22.69002229967135520, 0.7462262646974573421, -21.63419033603206643 ) ) ;
#39583 = CARTESIAN_POINT ( 'NONE',  ( 35.38149650531432400, -10.69973295221460141, -6.299277470973589921 ) ) ;
#39584 = ORIENTED_EDGE ( 'NONE', *, *, #32395, .T. ) ;
#39585 = CONTEXT_DEPENDENT_SHAPE_REPRESENTATION ( #33233, #35002 ) ;
#39586 = CARTESIAN_POINT ( 'NONE',  ( -4.984135866956331817, 36.15314577889358105, 7.500000000000000888 ) ) ;
#39587 = ORIENTED_EDGE ( 'NONE', *, *, #32223, .F. ) ;
#39588 = CARTESIAN_POINT ( 'NONE',  ( 13.37378135583786332, 20.59160479820249279, 10.00000000000000000 ) ) ;
#39589 = CARTESIAN_POINT ( 'NONE',  ( 6.688300058587269170, 16.47782454277055564, 13.00000000000000178 ) ) ;
#39590 = AXIS2_PLACEMENT_3D ( 'NONE', #39589, #11962, #5861 ) ;
#39591 = CARTESIAN_POINT ( 'NONE',  ( 1.229431105722923023, 20.49260818092372460, 13.00000000000000178 ) ) ;
#39592 = ORIENTED_EDGE ( 'NONE', *, *, #33487, .T. ) ;
#39593 = FILL_AREA_STYLE ('',( #23756 ) ) ;
#39594 = CARTESIAN_POINT ( 'NONE',  ( -19.48557158514988785, -11.24999999999987743, 10.00000000000000000 ) ) ;
#39595 = CARTESIAN_POINT ( 'NONE',  ( -13.30736835487442349, 15.68301270189233954, 7.499999999999993783 ) ) ;
#39596 = DIRECTION ( 'NONE',  ( 0.000000000000000000, 0.000000000000000000, 1.000000000000000000 ) ) ;
#39597 = ADVANCED_FACE ( 'NONE', ( #34735 ), #15515, .F. ) ;
#39598 = CARTESIAN_POINT ( 'NONE',  ( 28.89712736758817613, -22.26113267439890109, -9.299949049805807277 ) ) ;
#39599 = CARTESIAN_POINT ( 'NONE',  ( 16.25326542110554939, 12.54616751129404584, -28.85328854345905469 ) ) ;
#39600 = CARTESIAN_POINT ( 'NONE',  ( 9.822137042998281942, 25.39517083171130096, -16.97761038151271862 ) ) ;
#39601 = ORIENTED_EDGE ( 'NONE', *, *, #37090, .F. ) ;
#39602 = CARTESIAN_POINT ( 'NONE',  ( -21.81785358434161637, 11.77199115278586028, -5.000000000000000000 ) ) ;
#39603 = FACE_OUTER_BOUND ( 'NONE', #35409, .T. ) ;
#39604 = DIRECTION ( 'NONE',  ( 1.000000000000000000, 0.000000000000000000, 0.000000000000000000 ) ) ;
#39605 = CARTESIAN_POINT ( 'NONE',  ( 9.791560039807741589, -18.01123673837627592, -29.34227149249296929 ) ) ;
#39606 = DIRECTION ( 'NONE',  ( 0.000000000000000000, 0.000000000000000000, 1.000000000000000000 ) ) ;
#39607 = CARTESIAN_POINT ( 'NONE',  ( 9.941034666242806850, 32.57396620494213124, 7.000000000000000000 ) ) ;
#39608 = CARTESIAN_POINT ( 'NONE',  ( -11.10259761515444765, 17.62853563763367859, -26.82830193443789568 ) ) ;
#39609 = CARTESIAN_POINT ( 'NONE',  ( -13.59989706787225572, -15.33919494678365680, -30.00000000000001421 ) ) ;
#39610 = CARTESIAN_POINT ( 'NONE',  ( 14.19885085794842894, -26.30396096727126221, -6.890628514556540907 ) ) ;
#39611 = DIRECTION ( 'NONE',  ( 1.000000000000000000, 0.000000000000000000, 0.000000000000000000 ) ) ;
#39612 = EDGE_LOOP ( 'NONE', ( #14158, #10242 ) ) ;
#39613 = ORIENTED_EDGE ( 'NONE', *, *, #10914, .F. ) ;
#39614 = CARTESIAN_POINT ( 'NONE',  ( -8.796796072880949779, 22.03530637549132365, -21.13878428389095632 ) ) ;
#39615 = DIRECTION ( 'NONE',  ( 1.000000000000000000, 0.000000000000000000, 0.000000000000000000 ) ) ;
#39616 = DIRECTION ( 'NONE',  ( -0.6691306063588561281, 0.7431448254773961315, 0.000000000000000000 ) ) ;
#39617 = AXIS2_PLACEMENT_3D ( 'NONE', #19859, #17016, #26349 ) ;
#39618 = FACE_OUTER_BOUND ( 'NONE', #12844, .T. ) ;
#39619 = ORIENTED_EDGE ( 'NONE', *, *, #18736, .T. ) ;
#39620 = CARTESIAN_POINT ( 'NONE',  ( 20.47975215921984216, 0.9111364859620186829, -30.00000000000000000 ) ) ;
#39621 = VECTOR ( 'NONE', #21851, 1000.000000000000000 ) ;
#39622 = CARTESIAN_POINT ( 'NONE',  ( -14.47283171447380035, 21.48159823030330884, 7.000000000000000000 ) ) ;
#39623 = CARTESIAN_POINT ( 'NONE',  ( -2.629601561899621576, 7.723830143584065056, 10.59344459855561382 ) ) ;
#39624 = EDGE_CURVE ( 'NONE', #490, #13732, #11295, .T. ) ;
#39625 = ORIENTED_EDGE ( 'NONE', *, *, #32797, .F. ) ;
#39626 = CARTESIAN_POINT ( 'NONE',  ( -25.20729123572924379, 0.3862878095295266823, -17.43940099721178782 ) ) ;
#39627 = DIRECTION ( 'NONE',  ( 0.000000000000000000, 0.000000000000000000, 1.000000000000000000 ) ) ;
#39628 = VERTEX_POINT ( 'NONE', #32833 ) ;
#39629 = CARTESIAN_POINT ( 'NONE',  ( 30.71250582953177144, -3.685950063347092076, -12.25764069449938809 ) ) ;
#39630 = CARTESIAN_POINT ( 'NONE',  ( 33.26300037445852098, -0.3730773600908409704, 13.92931973827949221 ) ) ;
#39631 = EDGE_LOOP ( 'NONE', ( #27621, #5838, #27639, #34896, #6560 ) ) ;
#39632 = CARTESIAN_POINT ( 'NONE',  ( -15.23843103912111019, 30.59358247944625120, 14.53008259253998169 ) ) ;
#39633 = AXIS2_PLACEMENT_3D ( 'NONE', #25005, #3272, #6506 ) ;
#39634 = CARTESIAN_POINT ( 'NONE',  ( -11.73759695149396620, -17.78600041308340707, 20.69868183039790566 ) ) ;
#39635 = DIRECTION ( 'NONE',  ( 0.9135454576426048634, 0.4067366430757912710, 0.000000000000000000 ) ) ;
#39636 = CARTESIAN_POINT ( 'NONE',  ( 6.495117285921949701, 31.04668714394701823, 19.99202127657103745 ) ) ;
#39637 = DIRECTION ( 'NONE',  ( 0.000000000000000000, 0.000000000000000000, 1.000000000000000000 ) ) ;
#39638 = ORIENTED_EDGE ( 'NONE', *, *, #24693, .F. ) ;
#39639 = CARTESIAN_POINT ( 'NONE',  ( 14.23945615837883949, -31.58416516429907972, 3.000000000000000000 ) ) ;
#39640 = CARTESIAN_POINT ( 'NONE',  ( 0.000000000000000000, 22.50000000000000355, 11.00000000000000178 ) ) ;
#39641 = EDGE_CURVE ( 'NONE', #23735, #6691, #37139, .T. ) ;
#39642 = CARTESIAN_POINT ( 'NONE',  ( 7.734772747480874067, 34.12887688845987810, -10.23333199772818070 ) ) ;
#39643 = CIRCLE ( 'NONE', #26009, 1.000000000000000000 ) ;
#39644 = CARTESIAN_POINT ( 'NONE',  ( -9.754330675317843813, 26.45797082815842316, 10.74999999999999645 ) ) ;
#39645 = ADVANCED_FACE ( 'NONE', ( #29773 ), #8638, .T. ) ;
#39646 = CARTESIAN_POINT ( 'NONE',  ( 6.367390439425446580, 24.26983560722391786, 20.94377226548378346 ) ) ;
#39647 = AXIS2_PLACEMENT_3D ( 'NONE', #4514, #29497, #10814 ) ;
#39648 = CARTESIAN_POINT ( 'NONE',  ( 12.38700900889000422, -16.57502586561705016, -27.91489560070839460 ) ) ;
#39649 = LINE ( 'NONE', #3476, #6748 ) ;
#39650 = LINE ( 'NONE', #15469, #30028 ) ;
#39651 = DIRECTION ( 'NONE',  ( 0.000000000000000000, 0.000000000000000000, 1.000000000000000000 ) ) ;
#39652 = ORIENTED_EDGE ( 'NONE', *, *, #37086, .F. ) ;
#39653 = CARTESIAN_POINT ( 'NONE',  ( 10.95197819135580630, 17.38279901324217036, -28.70470247791863727 ) ) ;
#39654 = ORIENTED_EDGE ( 'NONE', *, *, #1425, .T. ) ;
#39655 = CARTESIAN_POINT ( 'NONE',  ( -15.04084753456836410, 25.47187635758209368, -9.713999766003432512 ) ) ;
#39656 = ADVANCED_FACE ( 'NONE', ( #1749 ), #24275, .T. ) ;
#39657 = CARTESIAN_POINT ( 'NONE',  ( -20.47921202893386194, -24.94416275241482950, 18.42518152272108978 ) ) ;
#39658 = CARTESIAN_POINT ( 'NONE',  ( 11.49405981918322439, -20.98321110018536828, -19.50239126088900221 ) ) ;
#39659 = CARTESIAN_POINT ( 'NONE',  ( 2.494936919103933448, 34.23777120880591696, 13.00000000000000178 ) ) ;
#39660 = CARTESIAN_POINT ( 'NONE',  ( 15.41013925098940440, 26.53795535406381489, -6.417150894498828251 ) ) ;
#39661 = ORIENTED_EDGE ( 'NONE', *, *, #36084, .T. ) ;
#39662 = CARTESIAN_POINT ( 'NONE',  ( 19.29646234545531769, -12.21333632372317091, -22.98710221298432543 ) ) ;
#39663 = EDGE_LOOP ( 'NONE', ( #37475, #8654, #36782, #3393 ) ) ;
#39665 = CARTESIAN_POINT ( 'NONE',  ( 13.67979938750375979, 27.47056737363388734, 10.99999999999999289 ) ) ;
#39664 = CARTESIAN_POINT ( 'NONE',  ( -15.11591168330041235, 27.33994589239279804, -6.872610621541277887 ) ) ;
#39666 = CARTESIAN_POINT ( 'NONE',  ( -14.88990478036455833, -23.71550094554306654, -14.34039717371376810 ) ) ;
#39667 = DIRECTION ( 'NONE',  ( 0.000000000000000000, 0.000000000000000000, 1.000000000000000000 ) ) ;
#39668 = ORIENTED_EDGE ( 'NONE', *, *, #31238, .T. ) ;
#39669 = CARTESIAN_POINT ( 'NONE',  ( -35.34736855013350976, -11.03791369283689328, -6.297914269266797760 ) ) ;
#39670 = CARTESIAN_POINT ( 'NONE',  ( -9.320207966883044648, -18.25898334416423197, -29.35196178604148542 ) ) ;
#39671 = DIRECTION ( 'NONE',  ( 1.000000000000000000, 0.000000000000000000, 0.000000000000000000 ) ) ;
#39672 = VERTEX_POINT ( 'NONE', #30175 ) ;
#39673 = CARTESIAN_POINT ( 'NONE',  ( 29.29107452043095350, 1.132527418749026182, -8.309007812652541958 ) ) ;
#39674 = FACE_OUTER_BOUND ( 'NONE', #39711, .T. ) ;
#39675 = PLANE ( 'NONE',  #8928 ) ;
#39676 = ADVANCED_FACE ( 'NONE', ( #20640 ), #28166, .T. ) ;
#39677 = ORIENTED_EDGE ( 'NONE', *, *, #4066, .T. ) ;
#39678 = EDGE_CURVE ( 'NONE', #19098, #855, #35191, .T. ) ;
#39679 = CARTESIAN_POINT ( 'NONE',  ( -23.34145163311095672, 0.4855504374881212115, -20.53287417781590918 ) ) ;
#39681 = ADVANCED_FACE ( 'NONE', ( #23475 ), #8839, .F. ) ;
#39680 = ORIENTED_EDGE ( 'NONE', *, *, #32494, .F. ) ;
#39682 = CARTESIAN_POINT ( 'NONE',  ( 30.92579311035478895, -1.297794089189396871, -9.623581977891010553 ) ) ;
#39683 = AXIS2_PLACEMENT_3D ( 'NONE', #30058, #29851, #24560 ) ;
#39684 = CARTESIAN_POINT ( 'NONE',  ( 20.47921202893403247, -24.94416275241516701, 18.42518152272108622 ) ) ;
#39685 = AXIS2_PLACEMENT_3D ( 'NONE', #34100, #6454, #16008 ) ;
#39686 = VERTEX_POINT ( 'NONE', #3134 ) ;
#39687 = CARTESIAN_POINT ( 'NONE',  ( -24.50095130057663084, 3.514676660001284425, -15.68173609412164282 ) ) ;
#39688 = CARTESIAN_POINT ( 'NONE',  ( -10.33756681542519118, 33.36973668161310513, 7.202682876670055911 ) ) ;
#39689 = DIRECTION ( 'NONE',  ( -1.000000000000000000, 0.000000000000000000, 0.000000000000000000 ) ) ;
#39690 = CARTESIAN_POINT ( 'NONE',  ( -15.60391421430763614, -26.29546805949255628, 16.87380292611442201 ) ) ;
#39691 = LINE ( 'NONE', #37045, #32503 ) ;
#39692 = EDGE_CURVE ( 'NONE', #39920, #6629, #2806, .T. ) ;
#39693 = CARTESIAN_POINT ( 'NONE',  ( 8.118377661053324701, 10.47536095541698486, 9.500000000000000000 ) ) ;
#39694 = ADVANCED_FACE ( 'NONE', ( #12871 ), #18188, .F. ) ;
#39695 = DIRECTION ( 'NONE',  ( -0.5877852522924797984, -0.8090169943749425663, 0.000000000000000000 ) ) ;
#39696 = VERTEX_POINT ( 'NONE', #27712 ) ;
#39697 = CARTESIAN_POINT ( 'NONE',  ( -21.25477442056000399, 6.622378896756878852, -20.01598680303737154 ) ) ;
#39698 = DIRECTION ( 'NONE',  ( 0.1045284632676559550, 0.9945218953682730678, 0.000000000000000000 ) ) ;
#39699 = CARTESIAN_POINT ( 'NONE',  ( -18.74997338764006471, -3.362744936731947298, 20.99999999999999645 ) ) ;
#39700 = CARTESIAN_POINT ( 'NONE',  ( 21.59233126178605033, -21.18517331184714081, -14.86128476917193630 ) ) ;
#39701 = DIRECTION ( 'NONE',  ( -0.000000000000000000, -0.000000000000000000, -1.000000000000000000 ) ) ;
#39702 = CARTESIAN_POINT ( 'NONE',  ( 11.01155832696060166, 17.88005758764968789, -26.20616980121537409 ) ) ;
#39703 = CARTESIAN_POINT ( 'NONE',  ( 4.250072516143177381E-14, -26.77689918168226058, 11.00000000000000000 ) ) ;
#39704 = ORIENTED_EDGE ( 'NONE', *, *, #8912, .T. ) ;
#39705 = CARTESIAN_POINT ( 'NONE',  ( -13.53617536424694379, 15.84659297203116424, -26.44149828717701567 ) ) ;
#39706 = CARTESIAN_POINT ( 'NONE',  ( -25.00594398452541967, -16.29738563782265004, 20.82122704794080192 ) ) ;
#39707 = CYLINDRICAL_SURFACE ( 'NONE', #1649, 1.000000000000000000 ) ;
#39708 = CARTESIAN_POINT ( 'NONE',  ( 15.35276837714096487, 26.56664761675495967, -6.888009055590721630 ) ) ;
#39709 = ORIENTED_EDGE ( 'NONE', *, *, #352, .T. ) ;
#39710 = CARTESIAN_POINT ( 'NONE',  ( 12.13489577391687746, 19.91918273965261932, -20.54176214682888357 ) ) ;
#39711 = EDGE_LOOP ( 'NONE', ( #13739, #16408, #12599, #35280 ) ) ;
#39713 = DIRECTION ( 'NONE',  ( -0.000000000000000000, -0.000000000000000000, -1.000000000000000000 ) ) ;
#39712 = CARTESIAN_POINT ( 'NONE',  ( -12.06785836680760937, 19.99931457666742318, -20.52815288208361011 ) ) ;
#39714 = B_SPLINE_CURVE_WITH_KNOTS ( 'NONE', 3,
 ( #2297, #38864, #36227, #4734 ),
 .UNSPECIFIED., .F., .F.,
 ( 4, 4 ),
 ( 0.000000000000000000, 1.000000000000000000 ),
 .UNSPECIFIED. ) ;
#39715 = CARTESIAN_POINT ( 'NONE',  ( -10.54623483126699668, -19.57291301703272879, -22.73368254332207883 ) ) ;
#39716 = CARTESIAN_POINT ( 'NONE',  ( 3.494936919103933448, 34.23777120880591696, 6.000000000000000000 ) ) ;
#39717 = CARTESIAN_POINT ( 'NONE',  ( -28.72041673430533137, -15.03451237313814204, -13.80826013931377005 ) ) ;
#39718 = CARTESIAN_POINT ( 'NONE',  ( -11.41304656535760209, -25.54597899413777640, -7.851881303444170790 ) ) ;
#39719 = DIRECTION ( 'NONE',  ( 0.3090169943749465631, -0.9510565162951538642, 0.000000000000000000 ) ) ;
#39720 = CARTESIAN_POINT ( 'NONE',  ( 15.83034964957195179, 23.90031239945711761, -8.791623678892117155 ) ) ;
#39721 = ORIENTED_EDGE ( 'NONE', *, *, #33018, .F. ) ;
#39722 = CARTESIAN_POINT ( 'NONE',  ( 20.06920181270377412, 5.944727635545681288, -25.41012073482777822 ) ) ;
#39723 = CARTESIAN_POINT ( 'NONE',  ( 5.953805871968278929, 30.22298757065274444, 6.000000000000000000 ) ) ;
#39724 = TOROIDAL_SURFACE ( 'NONE', #15703, 1.000000000000000000, 0.5000000000000000000 ) ;
#39725 = CYLINDRICAL_SURFACE ( 'NONE', #12113, 0.5000000000000005551 ) ;
#39726 = FACE_OUTER_BOUND ( 'NONE', #26111, .T. ) ;
#39727 = ORIENTED_EDGE ( 'NONE', *, *, #26182, .F. ) ;
#39728 = CARTESIAN_POINT ( 'NONE',  ( -25.76299961875513844, -0.6882523748748244907, -17.30342747421279270 ) ) ;
#39729 = CARTESIAN_POINT ( 'NONE',  ( 20.52955548149205001, 0.8017222527024847611, -28.70499869001353588 ) ) ;
#39730 = AXIS2_PLACEMENT_3D ( 'NONE', #37768, #399, #16435 ) ;
#39731 = DIRECTION ( 'NONE',  ( 0.9781476007338069101, 0.2079116908177532363, 0.000000000000000000 ) ) ;
#39732 = CARTESIAN_POINT ( 'NONE',  ( 28.10500611839371743, -8.168659512009874391, 20.50957957746006599 ) ) ;
#39733 = CARTESIAN_POINT ( 'NONE',  ( 35.48557158514988430, -11.24999999999998046, 6.000000000000000000 ) ) ;
#39734 = FACE_OUTER_BOUND ( 'NONE', #9126, .T. ) ;
#39735 = CIRCLE ( 'NONE', #5347, 1.000000000000000000 ) ;
#39736 = ORIENTED_EDGE ( 'NONE', *, *, #16325, .T. ) ;
#39737 = CARTESIAN_POINT ( 'NONE',  ( 10.10646936306337729, 32.94553861768082470, 7.499999999999997335 ) ) ;
#39738 = DIRECTION ( 'NONE',  ( 0.4067366430757995976, 0.9135454576426010886, 0.000000000000000000 ) ) ;
#39739 = CARTESIAN_POINT ( 'NONE',  ( 35.84808252048253507, -3.038699442442335030, -4.999999999999999112 ) ) ;
#39740 = CARTESIAN_POINT ( 'NONE',  ( 1.474331469296633612, 20.86371088087402370, -26.97373403608622766 ) ) ;
#39741 = CARTESIAN_POINT ( 'NONE',  ( 8.541469607472738090, 17.40487552589537401, 12.00000000000000000 ) ) ;
#39742 = CARTESIAN_POINT ( 'NONE',  ( 11.11100267139550013, 25.58833710557466290, 19.66345542862528717 ) ) ;
#39743 = AXIS2_PLACEMENT_3D ( 'NONE', #30498, #34343, #36784 ) ;
#39744 = LINE ( 'NONE', #11922, #10989 ) ;
#39745 = DIRECTION ( 'NONE',  ( 1.000000000000000000, 0.000000000000000000, 0.000000000000000000 ) ) ;
#39746 = DIRECTION ( 'NONE',  ( 0.000000000000000000, 0.000000000000000000, 1.000000000000000000 ) ) ;
#39747 = CARTESIAN_POINT ( 'NONE',  ( 0.000000000000000000, 22.50000000000000355, 12.00000000000000000 ) ) ;
#39748 = CARTESIAN_POINT ( 'NONE',  ( 12.66415514388964247, 24.32263371310837030, -15.28493877312508964 ) ) ;
#39749 = CARTESIAN_POINT ( 'NONE',  ( -13.37378135583788286, 20.59160479820268108, 10.50000000000000000 ) ) ;
#39750 = ORIENTED_EDGE ( 'NONE', *, *, #39173, .F. ) ;
#39751 = AXIS2_PLACEMENT_3D ( 'NONE', #25228, #3493, #34774 ) ;
#39753 = CARTESIAN_POINT ( 'NONE',  ( -15.41558956984162521, 26.78481017248023832, 0.000000000000000000 ) ) ;
#39752 = CARTESIAN_POINT ( 'NONE',  ( -18.28296541247297924, 14.26023631948706694, -15.91594685420020738 ) ) ;
#39754 = LINE ( 'NONE', #36720, #22428 ) ;
#39755 = CARTESIAN_POINT ( 'NONE',  ( 13.71882174050663927, -24.11825156489150856, -13.51284417636739654 ) ) ;
#39756 = CARTESIAN_POINT ( 'NONE',  ( -12.15296441974668262, -16.58779298946083358, -28.59925402789991367 ) ) ;
#39757 = CARTESIAN_POINT ( 'NONE',  ( 12.65336495216307533, 21.05333586549357960, -18.45227026116427993 ) ) ;
#39758 = CARTESIAN_POINT ( 'NONE',  ( 15.16184759445628139, 26.32446738171400824, -8.296192284030361463 ) ) ;
#39759 = ORIENTED_EDGE ( 'NONE', *, *, #10366, .T. ) ;
#39760 = CARTESIAN_POINT ( 'NONE',  ( -9.165211421344535481, 24.66068167190384841, 6.000000000000000000 ) ) ;
#39761 = CARTESIAN_POINT ( 'NONE',  ( 38.42882786495224678, -4.479089870562107834, 10.99999999999999822 ) ) ;
#39762 = CARTESIAN_POINT ( 'NONE',  ( -16.46096347412068539, -13.67449536700828716, -25.64341775554081337 ) ) ;
#39763 = VECTOR ( 'NONE', #2681, 1000.000000000000000 ) ;
#39764 = CARTESIAN_POINT ( 'NONE',  ( -0.2650373451695002269, -20.49916026595607121, -29.42941051173712097 ) ) ;
#39765 = CARTESIAN_POINT ( 'NONE',  ( 15.40551039434233083, 25.82709679606264430, -7.831030787721910968 ) ) ;
#39766 = CARTESIAN_POINT ( 'NONE',  ( 20.06132735707487669, 11.19275764913479065, -15.94899771753667572 ) ) ;
#39767 = DIRECTION ( 'NONE',  ( -0.9135454576426005335, 0.4067366430758010964, 0.000000000000000000 ) ) ;
#39768 = CARTESIAN_POINT ( 'NONE',  ( -2.848530395113699321, 20.31062432315956201, -29.99999999999998224 ) ) ;
#39769 = ORIENTED_EDGE ( 'NONE', *, *, #40153, .F. ) ;
#39770 = CARTESIAN_POINT ( 'NONE',  ( -34.83329005959444657, -6.589775719143758259, -5.000000000000002665 ) ) ;
#39771 = AXIS2_PLACEMENT_3D ( 'NONE', #33529, #23764, #8730 ) ;
#39772 = CARTESIAN_POINT ( 'NONE',  ( -23.18947492591177095, 13.38844959084094555, 11.55979286843934872 ) ) ;
#39773 = EDGE_LOOP ( 'NONE', ( #23228, #25584, #21587, #12584 ) ) ;
#39774 = CARTESIAN_POINT ( 'NONE',  ( 10.16520467992603294, 20.33931832809677331, 6.000000000000000000 ) ) ;
#39775 = EDGE_CURVE ( 'NONE', #4988, #21746, #5382, .T. ) ;
#39776 = CONICAL_SURFACE ( 'NONE', #24202, 0.5000000000000046629, 0.7853981633974492782 ) ;
#39777 = DIRECTION ( 'NONE',  ( 1.000000000000000000, 0.000000000000000000, 0.000000000000000000 ) ) ;
#39778 = CARTESIAN_POINT ( 'NONE',  ( -29.78284714116363574, 0.4461029049765271592, -8.773278634192886116 ) ) ;
#39779 = CARTESIAN_POINT ( 'NONE',  ( 24.92085914673013036, -9.179035951187309195, -18.69283157082075775 ) ) ;
#39780 = VECTOR ( 'NONE', #7905, 1000.000000000000000 ) ;
#39781 = ADVANCED_FACE ( 'NONE', ( #6372 ), #27914, .F. ) ;
#39782 = EDGE_LOOP ( 'NONE', ( #8987, #22733, #6814, #7625 ) ) ;
#39783 = CARTESIAN_POINT ( 'NONE',  ( -35.48557158514985588, -11.25000000000002309, 6.000000000000000000 ) ) ;
#39784 = ORIENTED_EDGE ( 'NONE', *, *, #9937, .T. ) ;
#39785 = ADVANCED_FACE ( 'NONE', ( #15325 ), #33829, .T. ) ;
#39786 = DIRECTION ( 'NONE',  ( 1.000000000000000000, 0.000000000000000000, -0.000000000000000000 ) ) ;
#39787 = DIRECTION ( 'NONE',  ( -0.000000000000000000, -0.000000000000000000, -1.000000000000000000 ) ) ;
#39788 = CARTESIAN_POINT ( 'NONE',  ( -3.820972158149174458, 8.017991022712379845, 10.49999999999999822 ) ) ;
#39789 = VERTEX_POINT ( 'NONE', #15531 ) ;
#39790 = FILL_AREA_STYLE_COLOUR ( '', #18410 ) ;
#39791 = CYLINDRICAL_SURFACE ( 'NONE', #24992, 0.5000000000000004441 ) ;
#39792 = CARTESIAN_POINT ( 'NONE',  ( -16.00000000000000000, 22.50000000000000355, 0.000000000000000000 ) ) ;
#39793 = DIRECTION ( 'NONE',  ( -0.1045284632676569680, -0.9945218953682730678, 0.000000000000000000 ) ) ;
#39794 = CARTESIAN_POINT ( 'NONE',  ( 23.74751641108253253, -18.28319883384900990, -15.71451449610176887 ) ) ;
#39795 = CARTESIAN_POINT ( 'NONE',  ( 16.64565377271186009, 14.14783685497081933, -21.10538628858365229 ) ) ;
#39796 = CARTESIAN_POINT ( 'NONE',  ( 12.20628291170280733, 31.91935747496564701, -8.112038654058029152 ) ) ;
#39797 = VERTEX_POINT ( 'NONE', #3332 ) ;
#39798 = CARTESIAN_POINT ( 'NONE',  ( -22.03145203603800084, 10.67872040110599485, -9.392672953967160510 ) ) ;
#39799 = FACE_OUTER_BOUND ( 'NONE', #9610, .T. ) ;
#39800 = EDGE_CURVE ( 'NONE', #30063, #6257, #7992, .T. ) ;
#39801 = STYLED_ITEM ( 'NONE', ( #36354 ), #3225 ) ;
#39802 = EDGE_CURVE ( 'NONE', #1089, #30187, #25263, .T. ) ;
#39803 = CARTESIAN_POINT ( 'NONE',  ( 13.49272883091155606, -23.63509699019526167, -14.46508437397573843 ) ) ;
#39804 = DIRECTION ( 'NONE',  ( 1.000000000000000000, 0.000000000000000000, 0.000000000000000000 ) ) ;
#39805 = CARTESIAN_POINT ( 'NONE',  ( -13.48130249190472796, 27.93180293473203335, 9.500000000000000000 ) ) ;
#39806 = CARTESIAN_POINT ( 'NONE',  ( -15.21760210513949829, 26.45671326379792987, -7.826101484237490524 ) ) ;
#39807 = CARTESIAN_POINT ( 'NONE',  ( -17.15649068250308673, -19.26226397553716652, -18.90765395908277569 ) ) ;
#39808 = CARTESIAN_POINT ( 'NONE',  ( 8.501931199692817742, -21.76549204576950203, -18.75867965171295282 ) ) ;
#39809 = CARTESIAN_POINT ( 'NONE',  ( 11.61617248865833396, 31.85261603038683376, 10.49999999999999822 ) ) ;
#39810 = VERTEX_POINT ( 'NONE', #6179 ) ;
#39811 = ORIENTED_EDGE ( 'NONE', *, *, #14157, .T. ) ;
#39812 = CARTESIAN_POINT ( 'NONE',  ( -6.868207022587211164, 20.65556158837918588, -24.50483338991505633 ) ) ;
#39813 = CARTESIAN_POINT ( 'NONE',  ( 0.8223886111234900431, 37.39061994947682877, 10.49999999999999822 ) ) ;
#39814 = FACE_OUTER_BOUND ( 'NONE', #19166, .T. ) ;
#39815 = CIRCLE ( 'NONE', #9977, 1.000000000000000000 ) ;
#39816 = DIRECTION ( 'NONE',  ( 0.000000000000000000, 0.000000000000000000, 1.000000000000000000 ) ) ;
#39817 = ORIENTED_EDGE ( 'NONE', *, *, #24791, .F. ) ;
#39818 = CARTESIAN_POINT ( 'NONE',  ( 25.20856571035977467, 0.3839094494008684078, -17.43916632868277716 ) ) ;
#39819 = DIRECTION ( 'NONE',  ( -0.000000000000000000, -0.000000000000000000, 1.000000000000000000 ) ) ;
#39820 = CARTESIAN_POINT ( 'NONE',  ( -13.01838097023000707, 23.73363068877903359, 12.00000000000000000 ) ) ;
#39821 = ORIENTED_EDGE ( 'NONE', *, *, #3553, .T. ) ;
#39822 = CARTESIAN_POINT ( 'NONE',  ( -29.33832633994033046, 0.09267334156268687562, -10.65398983853952508 ) ) ;
#39823 = EDGE_CURVE ( 'NONE', #19575, #15240, #22886, .T. ) ;
#39824 = CARTESIAN_POINT ( 'NONE',  ( -13.47830981910552772, 21.58612669357095015, 10.00000000000000000 ) ) ;
#39825 = ORIENTED_EDGE ( 'NONE', *, *, #26410, .F. ) ;
#39826 = CARTESIAN_POINT ( 'NONE',  ( 22.06145134990718404, -2.477892607279924775, -23.48296052362532294 ) ) ;
#39827 = VECTOR ( 'NONE', #23319, 1000.000000000000000 ) ;
#39828 = ORIENTED_EDGE ( 'NONE', *, *, #29697, .F. ) ;
#39829 = CARTESIAN_POINT ( 'NONE',  ( 12.39897218486625796, 35.60749793648125205, 12.14047268033093196 ) ) ;
#39830 = CARTESIAN_POINT ( 'NONE',  ( 5.869341256201768608, -17.04122685614420263, 20.69868183039781684 ) ) ;
#39831 = CARTESIAN_POINT ( 'NONE',  ( -35.36940577612494963, -20.42053594592269761, -4.999999999999992895 ) ) ;
#39832 = CARTESIAN_POINT ( 'NONE',  ( -6.495117285923170947, 31.04668714394608031, 19.99202127657103389 ) ) ;
#39833 = VECTOR ( 'NONE', #17629, 1000.000000000000000 ) ;
#39834 = LINE ( 'NONE', #17726, #29790 ) ;
#39835 = ORIENTED_EDGE ( 'NONE', *, *, #9616, .F. ) ;
#39836 = CARTESIAN_POINT ( 'NONE',  ( 19.48557158514982746, -11.25000000000009415, 3.000000000000000000 ) ) ;
#39837 = CARTESIAN_POINT ( 'NONE',  ( -1.587667106213708879, 35.31811204475769728, 13.00000000000000178 ) ) ;
#39838 = CARTESIAN_POINT ( 'NONE',  ( 3.888268390277564102, 20.12764833916413210, -29.23063393235646501 ) ) ;
#39839 = CARTESIAN_POINT ( 'NONE',  ( -17.34253826607186966, 27.32041144404028188, 11.00000000000000000 ) ) ;
#39840 = VECTOR ( 'NONE', #8169, 1000.000000000000000 ) ;
#39841 = CARTESIAN_POINT ( 'NONE',  ( 9.555312204549732513, 25.15592819203938291, 20.25080042701566541 ) ) ;
#39842 = EDGE_CURVE ( 'NONE', #30884, #39356, #18384, .T. ) ;
#39843 = EDGE_CURVE ( 'NONE', #33201, #6388, #9436, .T. ) ;
#39844 = CARTESIAN_POINT ( 'NONE',  ( 17.57430537192386666, -27.14116438782096097, -5.925949327191978533 ) ) ;
#39845 = FILL_AREA_STYLE ('',( #5721 ) ) ;
#39846 = FACE_OUTER_BOUND ( 'NONE', #25368, .T. ) ;
#39847 = DIRECTION ( 'NONE',  ( 1.000000000000000000, 0.000000000000000000, 0.000000000000000000 ) ) ;
#39848 = VERTEX_POINT ( 'NONE', #27519 ) ;
#39849 = CIRCLE ( 'NONE', #26865, 1.000000000000000000 ) ;
#39850 = ORIENTED_EDGE ( 'NONE', *, *, #11486, .F. ) ;
#39851 = CARTESIAN_POINT ( 'NONE',  ( -15.30597197327310433, 26.47602732279704441, -7.358011888683543944 ) ) ;
#39852 = CARTESIAN_POINT ( 'NONE',  ( -28.78471548569087091, -2.122417091764221109, 18.87996532025785257 ) ) ;
#39853 = CARTESIAN_POINT ( 'NONE',  ( 15.35461928258050612, -26.68267657520923919, -5.946095485900740663 ) ) ;
#39854 = DIRECTION ( 'NONE',  ( 0.000000000000000000, 0.000000000000000000, 1.000000000000000000 ) ) ;
#39855 = EDGE_LOOP ( 'NONE', ( #17680, #34193, #15542, #5937 ) ) ;
#39856 = ORIENTED_EDGE ( 'NONE', *, *, #23154, .F. ) ;
#39858 = CARTESIAN_POINT ( 'NONE',  ( 13.84312823610354748, 27.91543399189757579, 10.49999999999999822 ) ) ;
#39857 = CARTESIAN_POINT ( 'NONE',  ( -10.03540317069667509, 17.94769342537721712, -28.66663826095419054 ) ) ;
#39859 = CARTESIAN_POINT ( 'NONE',  ( -12.32505676087189350, -18.97741914115109907, -22.50295322248722130 ) ) ;
#39860 = CARTESIAN_POINT ( 'NONE',  ( 14.78469161520106034, 20.18088120075953640, 10.49999999999999822 ) ) ;
#39861 = AXIS2_PLACEMENT_3D ( 'NONE', #2673, #20960, #3269 ) ;
#39862 = ORIENTED_EDGE ( 'NONE', *, *, #19596, .F. ) ;
#39863 = CARTESIAN_POINT ( 'NONE',  ( -27.91051972509944434, -10.53651564714228783, -15.73446641547097968 ) ) ;
#39864 = CARTESIAN_POINT ( 'NONE',  ( -15.11465166066981247, -26.62188994178503876, -5.946145182990577815 ) ) ;
#39865 = DIRECTION ( 'NONE',  ( 1.000000000000000000, 0.000000000000000000, 0.000000000000000000 ) ) ;
#39866 = ORIENTED_EDGE ( 'NONE', *, *, #33431, .F. ) ;
#39867 = CARTESIAN_POINT ( 'NONE',  ( 26.36218513174588551, 2.083777371321898109, -13.61866023419330674 ) ) ;
#39868 = FACE_OUTER_BOUND ( 'NONE', #18582, .T. ) ;
#39869 = CARTESIAN_POINT ( 'NONE',  ( 33.75875814100317029, 2.759858869446390361, 11.00000000000000000 ) ) ;
#39870 = ORIENTED_EDGE ( 'NONE', *, *, #2420, .T. ) ;
#39871 = CARTESIAN_POINT ( 'NONE',  ( -20.97825103701413951, 0.7222979316363659086, -26.21732548705084298 ) ) ;
#39872 = ADVANCED_FACE ( 'NONE', ( #9828 ), #39776, .T. ) ;
#39873 = EDGE_LOOP ( 'NONE', ( #13315, #13080, #16376, #23426 ) ) ;
#39874 = CARTESIAN_POINT ( 'NONE',  ( 24.94893617927477436, -0.4134396669885003206, -18.34106591124777452 ) ) ;
#39875 = CARTESIAN_POINT ( 'NONE',  ( 29.28423149095714351, -1.632116715644855054, 18.42518152272108978 ) ) ;
#39876 = ORIENTED_EDGE ( 'NONE', *, *, #17259, .T. ) ;
#39877 = CARTESIAN_POINT ( 'NONE',  ( -21.25151043518313898, 2.851751769872009401, -24.07782968374341337 ) ) ;
#39878 = CARTESIAN_POINT ( 'NONE',  ( -10.67421745135738043, 33.03884568954855183, 7.485699520496981840 ) ) ;
#39879 = AXIS2_PLACEMENT_3D ( 'NONE', #3233, #21517, #24368 ) ;
#39880 = DIRECTION ( 'NONE',  ( 0.4999999999999920064, -0.8660254037844432595, 0.000000000000000000 ) ) ;
#39881 = DIRECTION ( 'NONE',  ( 1.000000000000000000, 0.000000000000000000, 0.000000000000000000 ) ) ;
#39882 = CARTESIAN_POINT ( 'NONE',  ( -1.204925152852743375, 12.02153850147729308, 10.50000000000000355 ) ) ;
#39883 = AXIS2_PLACEMENT_3D ( 'NONE', #17840, #9276, #34063 ) ;
#39884 = CIRCLE ( 'NONE', #20457, 1.000000000000002665 ) ;
#39885 = FACE_BOUND ( 'NONE', #7418, .T. ) ;
#39886 = LINE ( 'NONE', #17783, #37983 ) ;
#39887 = EDGE_LOOP ( 'NONE', ( #33513, #5752 ) ) ;
#39888 = CARTESIAN_POINT ( 'NONE',  ( -24.07025619749217427, 8.010103448123961911, -7.414577760795920902 ) ) ;
#39889 = CARTESIAN_POINT ( 'NONE',  ( 1.400691654708310141, 37.43445890845833901, 7.000000000000000000 ) ) ;
#39890 = CARTESIAN_POINT ( 'NONE',  ( 5.082600654608392610, 21.41965916404854298, 12.00000000000000000 ) ) ;
#39891 = CARTESIAN_POINT ( 'NONE',  ( 17.28033604266353507, -15.93370173550165347, -21.98823515398838779 ) ) ;
#39892 = EDGE_CURVE ( 'NONE', #32345, #14313, #18973, .T. ) ;
#39893 = LINE ( 'NONE', #14924, #9897 ) ;
#39894 = ADVANCED_FACE ( 'NONE', ( #25067 ), #3529, .F. ) ;
#39895 = CARTESIAN_POINT ( 'NONE',  ( 10.77342450413916630, 17.44087877699069367, -29.34380338842519009 ) ) ;
#39896 = CARTESIAN_POINT ( 'NONE',  ( -15.00437666250803836, -28.61930095463306500, 12.14047268033097460 ) ) ;
#39897 = ORIENTED_EDGE ( 'NONE', *, *, #24010, .T. ) ;
#39898 = CARTESIAN_POINT ( 'NONE',  ( -13.30210127107427986, 18.52526325335603730, -20.73340722121258750 ) ) ;
#39899 = CARTESIAN_POINT ( 'NONE',  ( -25.12106050720013073, -7.724475404461035311, 20.94377226548368753 ) ) ;
#39900 = CARTESIAN_POINT ( 'NONE',  ( 2.525645716490518833, 8.212903943950921715, 7.000000000000000000 ) ) ;
#39901 = CARTESIAN_POINT ( 'NONE',  ( 13.50462022322065359, 22.78994049946557965, -15.45234425914835796 ) ) ;
#39902 = EDGE_LOOP ( 'NONE', ( #19840, #21987, #2812, #26232 ) ) ;
#39903 = DIRECTION ( 'NONE',  ( -0.5877852522924797984, -0.8090169943749425663, 0.000000000000000000 ) ) ;
#39904 = ORIENTED_EDGE ( 'NONE', *, *, #23908, .T. ) ;
#39906 = DIRECTION ( 'NONE',  ( 1.000000000000000000, 0.000000000000000000, 0.000000000000000000 ) ) ;
#39905 = CARTESIAN_POINT ( 'NONE',  ( -11.04193823641116801, 17.67045093990668292, -26.82258941759701543 ) ) ;
#39907 = CARTESIAN_POINT ( 'NONE',  ( -10.06113038743805532, -18.77530449096024512, -25.00346255012576435 ) ) ;
#39908 = FACE_OUTER_BOUND ( 'NONE', #32964, .T. ) ;
#39909 = AXIS2_PLACEMENT_3D ( 'NONE', #23724, #10732, #11340 ) ;
#39910 = CARTESIAN_POINT ( 'NONE',  ( -33.58157224492879322, -18.91014262129728962, -4.999999999999998224 ) ) ;
#39911 = CARTESIAN_POINT ( 'NONE',  ( -13.80334467884919647, -26.14942442241866516, -7.363983261614664322 ) ) ;
#39912 = CARTESIAN_POINT ( 'NONE',  ( -11.85099884957084626, 31.69690594862152722, 7.259166423030696258 ) ) ;
#39913 = CARTESIAN_POINT ( 'NONE',  ( 16.08594598475725590, 23.47361198360156820, -8.321775003293000239 ) ) ;
#39914 = VERTEX_POINT ( 'NONE', #37659 ) ;
#39915 = CARTESIAN_POINT ( 'NONE',  ( 21.78838290119088583, 6.945878216539049355, -17.92683057917631118 ) ) ;
#39916 = DIRECTION ( 'NONE',  ( 0.000000000000000000, 0.000000000000000000, 1.000000000000000000 ) ) ;
#39917 = CARTESIAN_POINT ( 'NONE',  ( -12.80736835487442349, 15.68301270189233954, 7.499999999999993783 ) ) ;
#39918 = DIRECTION ( 'NONE',  ( 0.000000000000000000, 0.000000000000000000, 1.000000000000000000 ) ) ;
#39919 = VECTOR ( 'NONE', #30773, 1000.000000000000000 ) ;
#39920 = VERTEX_POINT ( 'NONE', #22207 ) ;
#39921 = CARTESIAN_POINT ( 'NONE',  ( -31.63647013363080873, -0.8270238094956995356, -4.999999999999999112 ) ) ;
#39922 = EDGE_CURVE ( 'NONE', #37976, #39686, #26785, .T. ) ;
#39923 = CARTESIAN_POINT ( 'NONE',  ( 22.25509359485367256, 0.5259994801797849284, -22.71717593399117874 ) ) ;
#39924 = AXIS2_PLACEMENT_3D ( 'NONE', #39495, #11274, #5171 ) ;
#39925 = VECTOR ( 'NONE', #39267, 1000.000000000000000 ) ;
#39926 = CARTESIAN_POINT ( 'NONE',  ( 0.000000000000000000, 22.50000000000000355, 7.000000000000000000 ) ) ;
#39927 = ADVANCED_FACE ( 'NONE', ( #2739 ), #12079, .F. ) ;
#39928 = CARTESIAN_POINT ( 'NONE',  ( 24.94906875546882219, -17.45075080782927301, 20.69868183039781329 ) ) ;
#39929 = CARTESIAN_POINT ( 'NONE',  ( 21.88444403592372112, 6.126538576424477966, -21.50719306941230613 ) ) ;
#39930 = DIRECTION ( 'NONE',  ( 0.000000000000000000, 0.000000000000000000, 1.000000000000000000 ) ) ;
#39931 = ADVANCED_FACE ( 'NONE', ( #26061 ), #682, .F. ) ;
#39932 = ORIENTED_EDGE ( 'NONE', *, *, #5943, .T. ) ;
#39933 = PLANE ( 'NONE',  #2237 ) ;
#39934 = CARTESIAN_POINT ( 'NONE',  ( -18.74997338763903798, -3.362744936732933176, 23.00000000000000000 ) ) ;
#39935 = LINE ( 'NONE', #33667, #35238 ) ;
#39936 = CARTESIAN_POINT ( 'NONE',  ( 0.8308715916267807033, 20.49243450554475743, -30.00000000000001066 ) ) ;
#39937 = CARTESIAN_POINT ( 'NONE',  ( -5.037377569032697622, 36.27272859966233653, 10.49999999999999822 ) ) ;
#39938 = DIRECTION ( 'NONE',  ( -0.4156269377774379215, 0.5720614028176924659, -0.7071067811865500152 ) ) ;
#39939 = DIRECTION ( 'NONE',  ( 0.000000000000000000, 0.000000000000000000, 1.000000000000000000 ) ) ;
#39940 = AXIS2_PLACEMENT_3D ( 'NONE', #34215, #6369, #28109 ) ;
#39941 = EDGE_CURVE ( 'NONE', #39797, #20959, #18380, .T. ) ;
#39942 = CARTESIAN_POINT ( 'NONE',  ( -11.14717575287011542, 32.53695909538323860, 12.00000000000000000 ) ) ;
#39943 = DIRECTION ( 'NONE',  ( 1.000000000000000000, 0.000000000000000000, 0.000000000000000000 ) ) ;
#39944 = CARTESIAN_POINT ( 'NONE',  ( -4.881458130668121953, -28.77689918168226058, 11.00000000000000000 ) ) ;
#39945 = EDGE_CURVE ( 'NONE', #17659, #27275, #17729, .T. ) ;
#39946 = CARTESIAN_POINT ( 'NONE',  ( 14.87731805253066142, 27.78693658398923461, -7.324495699756750078 ) ) ;
#39947 = CARTESIAN_POINT ( 'NONE',  ( -14.09933648065464062, 26.02968990214173317, 7.000000000000000000 ) ) ;
#39948 = ORIENTED_EDGE ( 'NONE', *, *, #31146, .F. ) ;
#39951 = AXIS2_PLACEMENT_3D ( 'NONE', #36168, #11387, #2638 ) ;
#39950 = CARTESIAN_POINT ( 'NONE',  ( 3.476901250629512941, 26.36149378532653031, 12.00000000000000000 ) ) ;
#39949 = CARTESIAN_POINT ( 'NONE',  ( -16.47736608385881141, 12.45964520604596082, -27.15966153433127062 ) ) ;
#39952 = CARTESIAN_POINT ( 'NONE',  ( -6.282361020112263716, 14.70372268239681190, 10.50000000000000533 ) ) ;
#39953 = VECTOR ( 'NONE', #336, 1000.000000000000000 ) ;
#39954 = CARTESIAN_POINT ( 'NONE',  ( 10.23053142960224804, -19.16244173123859440, -23.85327837102780180 ) ) ;
#39955 = CARTESIAN_POINT ( 'NONE',  ( -12.67448603152304187, -16.20977607892205086, -28.57815234595146237 ) ) ;
#39956 = DIRECTION ( 'NONE',  ( 0.000000000000000000, 0.000000000000000000, 1.000000000000000000 ) ) ;
#39957 = CARTESIAN_POINT ( 'NONE',  ( 13.19408550500376265, 22.26414250881884982, -16.44051050966041316 ) ) ;
#39958 = VERTEX_POINT ( 'NONE', #13266 ) ;
#39959 = CARTESIAN_POINT ( 'NONE',  ( -4.003810537522578983, 8.420815593655365916, 10.49999999999999822 ) ) ;
#39960 = DIRECTION ( 'NONE',  ( -0.8660254037844364872, 0.5000000000000038858, 0.000000000000000000 ) ) ;
#39961 = CARTESIAN_POINT ( 'NONE',  ( -35.26975574857812745, -18.21959598282740345, 14.53008259254033696 ) ) ;
#39962 = CARTESIAN_POINT ( 'NONE',  ( -24.51042783259964963, -20.45774332969374854, -13.85571432261770042 ) ) ;
#39963 = CARTESIAN_POINT ( 'NONE',  ( 1.432041688667228030, -21.91824802019722895, -20.12581347459805414 ) ) ;
#39964 = CARTESIAN_POINT ( 'NONE',  ( 14.03171047072867239, 22.83987516452802780, -14.50959830643082604 ) ) ;
#39965 = CARTESIAN_POINT ( 'NONE',  ( 17.68185794339073169, 10.78269052861306321, -26.62269099698529473 ) ) ;
#39966 = CARTESIAN_POINT ( 'NONE',  ( 13.05736835487433289, 16.11602540378438420, 10.50000000000000178 ) ) ;
#39967 = CARTESIAN_POINT ( 'NONE',  ( -5.264215711173335421, 37.05024581972982389, -7.560166499036732546 ) ) ;
#39968 = VERTEX_POINT ( 'NONE', #22814 ) ;
#39969 = CARTESIAN_POINT ( 'NONE',  ( -22.02142196946409669, -4.043980901898116542, -23.33374139521805901 ) ) ;
#39970 = ADVANCED_FACE ( 'NONE', ( #25859 ), #22406, .T. ) ;
#39971 = CARTESIAN_POINT ( 'NONE',  ( -32.28722999652026715, 1.315479119632480876, 12.14047268033097282 ) ) ;
#39972 = ORIENTED_EDGE ( 'NONE', *, *, #19850, .F. ) ;
#39973 = EDGE_CURVE ( 'NONE', #8857, #12667, #37829, .T. ) ;
#39974 = CARTESIAN_POINT ( 'NONE',  ( -14.97009266215794021, 21.42933399866948463, 7.000000000000000000 ) ) ;
#39975 = CARTESIAN_POINT ( 'NONE',  ( -10.18324708981896087, 16.78440424842446532, 13.00000000000000178 ) ) ;
#39976 = AXIS2_PLACEMENT_3D ( 'NONE', #29867, #11392, #38611 ) ;
#39977 = CARTESIAN_POINT ( 'NONE',  ( -20.45512865215935960, 1.365572444264179897, -30.00000000000000000 ) ) ;
#39978 = CARTESIAN_POINT ( 'NONE',  ( 19.79492923429188522, -6.644088801164120817, -27.03743231145483961 ) ) ;
#39979 = AXIS2_PLACEMENT_3D ( 'NONE', #17804, #23678, #29776 ) ;
#39980 = VERTEX_POINT ( 'NONE', #13469 ) ;
#39981 = LINE ( 'NONE', #9313, #40094 ) ;
#39982 = ORIENTED_EDGE ( 'NONE', *, *, #27318, .T. ) ;
#39983 = DIRECTION ( 'NONE',  ( 0.000000000000000000, 0.000000000000000000, 1.000000000000000000 ) ) ;
#39984 = FACE_OUTER_BOUND ( 'NONE', #17547, .T. ) ;
#39985 = DIRECTION ( 'NONE',  ( 0.000000000000000000, 0.000000000000000000, -1.000000000000000000 ) ) ;
#39986 = ORIENTED_EDGE ( 'NONE', *, *, #23558, .T. ) ;
#39987 = CARTESIAN_POINT ( 'NONE',  ( -4.146361853739318093, 37.19997570623368688, -7.982000101131666803 ) ) ;
#39988 = DIRECTION ( 'NONE',  ( 0.000000000000000000, 0.000000000000000000, -1.000000000000000000 ) ) ;
#39989 = CARTESIAN_POINT ( 'NONE',  ( 6.576253646258389374, 14.29921418520925869, 10.00000000000000000 ) ) ;
#39990 = DIRECTION ( 'NONE',  ( 0.8660254037844364872, -0.5000000000000038858, 0.000000000000000000 ) ) ;
#39991 = CARTESIAN_POINT ( 'NONE',  ( 24.71324896981895591, -20.25039165369232208, -13.85207717093263646 ) ) ;
#39992 = CARTESIAN_POINT ( 'NONE',  ( 16.38953877806516246, 12.68919556586870456, -26.59742149645854781 ) ) ;
#39993 = CARTESIAN_POINT ( 'NONE',  ( 12.83069131337032509, 30.87910589201018041, -8.585112319502103517 ) ) ;
#39994 = ORIENTED_EDGE ( 'NONE', *, *, #4531, .T. ) ;
#39995 = CARTESIAN_POINT ( 'NONE',  ( -20.34773337042144092, 9.024600177409785928, -19.04359522162117102 ) ) ;
#39996 = CARTESIAN_POINT ( 'NONE',  ( -0.3762682982559537037, 25.43444280220171194, 13.00000000000000178 ) ) ;
#39997 = CARTESIAN_POINT ( 'NONE',  ( 15.37979159366119397, -26.42576798054937370, -7.823598831600837578 ) ) ;
#39998 = CARTESIAN_POINT ( 'NONE',  ( 0.000000000000000000, 22.50000000000000355, 12.00000000000000000 ) ) ;
#39999 = EDGE_CURVE ( 'NONE', #8131, #10797, #13062, .T. ) ;
#40000 = CARTESIAN_POINT ( 'NONE',  ( 22.40982762235196901, 2.618079236896951656, -21.24786896499729139 ) ) ;
#40001 = AXIS2_PLACEMENT_3D ( 'NONE', #36977, #24978, #39615 ) ;
#40002 = CARTESIAN_POINT ( 'NONE',  ( -11.28807574537728442, 18.05517005563689281, -25.01156050316573243 ) ) ;
#40003 = AXIS2_PLACEMENT_3D ( 'NONE', #20392, #17947, #32786 ) ;
#40004 = CARTESIAN_POINT ( 'NONE',  ( -13.59989706787225572, -15.33919494678365680, -29.26247283103435493 ) ) ;
#40005 = CARTESIAN_POINT ( 'NONE',  ( 10.21648603655621379, -24.71841561882959581, -10.75073561233235253 ) ) ;
#40006 = CARTESIAN_POINT ( 'NONE',  ( 19.15807744002891155, 8.842452143891316396, 7.000000000000000000 ) ) ;
#40007 = ORIENTED_EDGE ( 'NONE', *, *, #19053, .T. ) ;
#40008 = ORIENTED_EDGE ( 'NONE', *, *, #34226, .F. ) ;
#40009 = CARTESIAN_POINT ( 'NONE',  ( -6.548765011332742247, 19.65220123129988039, -27.84161395793670124 ) ) ;
#40010 = CARTESIAN_POINT ( 'NONE',  ( 0.6308996938995748982, 37.50000000000000711, 10.49999999999999645 ) ) ;
#40011 = CARTESIAN_POINT ( 'NONE',  ( 8.917734535019441466, 14.47043272369397116, 13.00000000000000178 ) ) ;
#40012 = CARTESIAN_POINT ( 'NONE',  ( -9.067459072332603398, 10.87036407658132120, 10.94387467463491070 ) ) ;
#40013 = ORIENTED_EDGE ( 'NONE', *, *, #22230, .T. ) ;
#40014 = CARTESIAN_POINT ( 'NONE',  ( 20.81540970976022109, 0.8324466887874750753, -26.83074899403284164 ) ) ;
#40015 = CARTESIAN_POINT ( 'NONE',  ( 8.301277145684258230, 36.28737808747508353, -5.000000000000000888 ) ) ;
#40016 = CARTESIAN_POINT ( 'NONE',  ( 0.000000000000000000, 0.000000000000000000, -30.00000000000000000 ) ) ;
#40017 = EDGE_LOOP ( 'NONE', ( #6830, #14618, #29528, #28589 ) ) ;
#40018 = CARTESIAN_POINT ( 'NONE',  ( -20.48057623381365033, 0.8922431241703845384, -30.00000000000000000 ) ) ;
#40019 = DIRECTION ( 'NONE',  ( -0.000000000000000000, -0.000000000000000000, -1.000000000000000000 ) ) ;
#40020 = ORIENTED_EDGE ( 'NONE', *, *, #12360, .T. ) ;
#40021 = CARTESIAN_POINT ( 'NONE',  ( 28.07197903033539532, -5.801645677830485681, -15.91382734764840201 ) ) ;
#40022 = ORIENTED_EDGE ( 'NONE', *, *, #25689, .F. ) ;
#40023 = CARTESIAN_POINT ( 'NONE',  ( -1.464931600276310347E-13, 40.43805239114132632, 12.14047268033097637 ) ) ;
#40024 = EDGE_CURVE ( 'NONE', #27921, #26306, #30041, .T. ) ;
#40025 = CARTESIAN_POINT ( 'NONE',  ( 17.83459896181356541, -17.64923967996807264, 20.94377226548378346 ) ) ;
#40026 = CARTESIAN_POINT ( 'NONE',  ( -33.62187204924172335, 0.04418559750806146796, -5.000000000000002665 ) ) ;
#40027 = CARTESIAN_POINT ( 'NONE',  ( 5.145977874758831838, 31.04572515098157481, 20.25080042701566896 ) ) ;
#40028 = AXIS2_PLACEMENT_3D ( 'NONE', #3297, #37028, #3497 ) ;
#40029 = AXIS2_PLACEMENT_3D ( 'NONE', #354, #34082, #37724 ) ;
#40030 = FACE_BOUND ( 'NONE', #5925, .T. ) ;
#40031 = VERTEX_POINT ( 'NONE', #16324 ) ;
#40032 =( NAMED_UNIT ( * ) PLANE_ANGLE_UNIT ( ) SI_UNIT ( $, .RADIAN. ) );
#40033 = LINE ( 'NONE', #8768, #21711 ) ;
#40034 = DIRECTION ( 'NONE',  ( 0.000000000000000000, 0.000000000000000000, 1.000000000000000000 ) ) ;
#40035 = AXIS2_PLACEMENT_3D ( 'NONE', #35491, #16197, #22880 ) ;
#40036 = CARTESIAN_POINT ( 'NONE',  ( 7.953805871968279817, 30.22298757065274444, 13.00000000000000178 ) ) ;
#40037 = VECTOR ( 'NONE', #39145, 1000.000000000000000 ) ;
#40038 = CARTESIAN_POINT ( 'NONE',  ( 7.873866743966726922, 34.78796317335525856, -9.337550848925753044 ) ) ;
#40039 = CARTESIAN_POINT ( 'NONE',  ( 2.063787492809801893, 7.980908877017387937, 10.49999999999999467 ) ) ;
#40040 = EDGE_CURVE ( 'NONE', #29140, #634, #196, .T. ) ;
#40041 = B_SPLINE_CURVE_WITH_KNOTS ( 'NONE', 3,
 ( #2129, #17974, #9021, #2332, #33813, #1934, #3120, #13049 ),
 .UNSPECIFIED., .F., .F.,
 ( 4, 2, 2, 4 ),
 ( 0.000000000000000000, 0.0002364868538934332008, 0.0004729737077868664016, 0.0009459474155737283580 ),
 .UNSPECIFIED. ) ;
#40042 = CARTESIAN_POINT ( 'NONE',  ( 17.00416740508952174, -26.36028068555279447, -9.146751134521531768 ) ) ;
#40043 = CARTESIAN_POINT ( 'NONE',  ( -2.568190708544555001, 12.82247983807085134, 10.50000000000000533 ) ) ;
#40044 = DIRECTION ( 'NONE',  ( 0.000000000000000000, 0.000000000000000000, 1.000000000000000000 ) ) ;
#40045 = CYLINDRICAL_SURFACE ( 'NONE', #32398, 1.000000000000000888 ) ;
#40046 = VERTEX_POINT ( 'NONE', #29118 ) ;
#40047 = CARTESIAN_POINT ( 'NONE',  ( -11.71011565210685035, 18.88845938667280677, -22.73910212722063662 ) ) ;
#40048 = CARTESIAN_POINT ( 'NONE',  ( -33.27313359468927700, -17.33775975077042375, 17.42190598798430301 ) ) ;
#40049 = CARTESIAN_POINT ( 'NONE',  ( 10.65270019876893137, -20.03412338725443220, -21.63978030402215680 ) ) ;
#40050 = ADVANCED_FACE ( 'NONE', ( #10634 ), #34808, .F. ) ;
#40051 = LINE ( 'NONE', #5930, #12689 ) ;
#40052 = ADVANCED_FACE ( 'NONE', ( #19775 ), #32169, .F. ) ;
#40053 = VERTEX_POINT ( 'NONE', #23016 ) ;
#40054 = ORIENTED_EDGE ( 'NONE', *, *, #21441, .T. ) ;
#40055 = CARTESIAN_POINT ( 'NONE',  ( -9.673362312327872914, 18.76285134508493968, -26.06461302575264583 ) ) ;
#40056 = CARTESIAN_POINT ( 'NONE',  ( -20.54949627891300779, -27.17849093361366641, -5.904791858424460749 ) ) ;
#40057 = CARTESIAN_POINT ( 'NONE',  ( -6.354454053420243831, 35.54304081427989814, 7.500000000000000888 ) ) ;
#40058 = AXIS2_PLACEMENT_3D ( 'NONE', #21536, #18498, #15442 ) ;
#40059 = CIRCLE ( 'NONE', #12172, 1.000000000000000000 ) ;
#40060 = ORIENTED_EDGE ( 'NONE', *, *, #34928, .F. ) ;
#40061 = CARTESIAN_POINT ( 'NONE',  ( -35.33576435770064705, -9.891194556348709810, -6.303855711779147164 ) ) ;
#40062 = CARTESIAN_POINT ( 'NONE',  ( -12.86026711733400774, -23.08413008810780198, -15.46047026364893995 ) ) ;
#40063 = CARTESIAN_POINT ( 'NONE',  ( 39.51968005975079734, -13.07391886567386763, 11.00000000000000000 ) ) ;
#40064 = EDGE_LOOP ( 'NONE', ( #34016, #22826, #10510, #2691 ) ) ;
#40065 = CARTESIAN_POINT ( 'NONE',  ( 20.87261353721463664, 1.691488166188070075, -26.30017656618466404 ) ) ;
#40066 = DIRECTION ( 'NONE',  ( 0.000000000000000000, 0.000000000000000000, 1.000000000000000000 ) ) ;
#40067 = DIRECTION ( 'NONE',  ( -1.000000000000000000, 0.000000000000000000, 0.000000000000000000 ) ) ;
#40068 = VECTOR ( 'NONE', #6206, 999.9999999999998863 ) ;
#40069 = ORIENTED_EDGE ( 'NONE', *, *, #15466, .T. ) ;
#40070 = CARTESIAN_POINT ( 'NONE',  ( -29.42332256357913067, -0.003158690108220226205, -10.64750720974525500 ) ) ;
#40071 = ORIENTED_EDGE ( 'NONE', *, *, #665, .F. ) ;
#40072 = CARTESIAN_POINT ( 'NONE',  ( 28.21183386950785632, -1.421389276423470127, -14.30337687367899235 ) ) ;
#40073 = AXIS2_PLACEMENT_3D ( 'NONE', #3152, #15740, #27932 ) ;
#40074 = DIRECTION ( 'NONE',  ( -0.000000000000000000, -0.000000000000000000, -1.000000000000000000 ) ) ;
#40075 = CARTESIAN_POINT ( 'NONE',  ( 30.63324413334751029, -19.40199358733793744, 18.42518152272108622 ) ) ;
#40076 = ADVANCED_FACE ( 'NONE', ( #19165 ), #35210, .T. ) ;
#40077 = VERTEX_POINT ( 'NONE', #3723 ) ;
#40078 = CARTESIAN_POINT ( 'NONE',  ( -26.22013064122013404, 3.515541298840649809, -11.72090826476172865 ) ) ;
#40079 = ADVANCED_FACE ( 'NONE', ( #31764 ), #4125, .F. ) ;
#40080 = FACE_OUTER_BOUND ( 'NONE', #8914, .T. ) ;
#40081 = CARTESIAN_POINT ( 'NONE',  ( 4.817371740575539185, 23.83900317890011422, 23.00000000000000000 ) ) ;
#40082 = CARTESIAN_POINT ( 'NONE',  ( 17.34253826607186255, 27.32041144404028543, 0.000000000000000000 ) ) ;
#40083 = LINE ( 'NONE', #9215, #26627 ) ;
#40084 = CIRCLE ( 'NONE', #22564, 0.9999999999999996669 ) ;
#40085 = AXIS2_PLACEMENT_3D ( 'NONE', #4296, #4501, #16696 ) ;
#40086 = AXIS2_PLACEMENT_3D ( 'NONE', #9001, #40066, #12438 ) ;
#40087 = CARTESIAN_POINT ( 'NONE',  ( -11.74460609746112461, 31.83082137946488643, 7.365559175140416137 ) ) ;
#40088 = CARTESIAN_POINT ( 'NONE',  ( 22.89849980942894092, 13.22045502901191405, 13.32518128616608877 ) ) ;
#40089 = ORIENTED_EDGE ( 'NONE', *, *, #27301, .F. ) ;
#40090 = CARTESIAN_POINT ( 'NONE',  ( -23.94224112514191205, 7.985727600362816148, -8.389107632434875228 ) ) ;
#40091 = DIRECTION ( 'NONE',  ( 1.000000000000000000, 0.000000000000000000, 0.000000000000000000 ) ) ;
#40092 = DIRECTION ( 'NONE',  ( -1.000000000000000000, 0.000000000000000000, 0.000000000000000000 ) ) ;
#40093 = CARTESIAN_POINT ( 'NONE',  ( 18.05169300019579026, -18.77641457309465522, -18.83767055183944095 ) ) ;
#40094 = VECTOR ( 'NONE', #368, 1000.000000000000000 ) ;
#40095 = CARTESIAN_POINT ( 'NONE',  ( 1.587660364795204782, 9.681887955242936883, 13.00000000000000178 ) ) ;
#40096 = ADVANCED_FACE ( 'NONE', ( #3663 ), #12806, .F. ) ;
#40097 = CARTESIAN_POINT ( 'NONE',  ( 15.15757690463086149, 26.65769437118299479, -7.819476649599757856 ) ) ;
#40098 = ORIENTED_EDGE ( 'NONE', *, *, #26662, .F. ) ;
#40099 = CARTESIAN_POINT ( 'NONE',  ( -14.75810761987182929, 21.35594160732316027, -14.59729096891024192 ) ) ;
#40100 = CARTESIAN_POINT ( 'NONE',  ( -18.64638308222451357, -17.01267446048745668, 20.99999999999999645 ) ) ;
#40101 = CARTESIAN_POINT ( 'NONE',  ( -5.688306800005769048, 28.52217545723006609, 6.000000000000000000 ) ) ;
#40102 = CARTESIAN_POINT ( 'NONE',  ( 15.30435262198499480, 26.48161234833224498, -7.357992236420034970 ) ) ;
#40103 = ORIENTED_EDGE ( 'NONE', *, *, #19189, .F. ) ;
#40104 = DIRECTION ( 'NONE',  ( 0.8090169943749503378, 0.5877852522924691403, 0.000000000000000000 ) ) ;
#40105 = VERTEX_POINT ( 'NONE', #22147 ) ;
#40107 = CARTESIAN_POINT ( 'NONE',  ( -13.13581098909220479, 27.45627467658446008, 9.500000000000000000 ) ) ;
#40106 = CARTESIAN_POINT ( 'NONE',  ( -15.31676148297655615, 27.12555199532522110, -5.472534537103582508 ) ) ;
#40108 = CARTESIAN_POINT ( 'NONE',  ( -15.53934119414200410, -26.55776016592740163, -7.352091074212602884 ) ) ;
#40109 = DIRECTION ( 'NONE',  ( 0.000000000000000000, 0.000000000000000000, 1.000000000000000000 ) ) ;
#40110 = CARTESIAN_POINT ( 'NONE',  ( -18.72341571292924201, -9.819713513424439100, -26.25964704346830558 ) ) ;
#40111 = CARTESIAN_POINT ( 'NONE',  ( -9.876300105305748644, -20.21249212776923443, -21.72942160044624771 ) ) ;
#40112 = CARTESIAN_POINT ( 'NONE',  ( 75.15099915297797395, 43.38844959084117647, -5.000000000000000000 ) ) ;
#40113 = CARTESIAN_POINT ( 'NONE',  ( 12.28921816709972248, 16.91395354023228492, -26.33542656321613151 ) ) ;
#40114 = ORIENTED_EDGE ( 'NONE', *, *, #17365, .F. ) ;
#40115 = CARTESIAN_POINT ( 'NONE',  ( 21.86544796520013634, 5.303751907987186875, -19.93596551504636238 ) ) ;
#40116 = DIRECTION ( 'NONE',  ( -0.000000000000000000, -0.000000000000000000, 1.000000000000000000 ) ) ;
#40117 = DIRECTION ( 'NONE',  ( 0.000000000000000000, 0.000000000000000000, 1.000000000000000000 ) ) ;
#40118 = CARTESIAN_POINT ( 'NONE',  ( -20.46001567034013391, -27.07608408263049427, -6.799282311406788182 ) ) ;
#40119 = ORIENTED_EDGE ( 'NONE', *, *, #10356, .T. ) ;
#40120 = CARTESIAN_POINT ( 'NONE',  ( -31.98245490244095635, -1.244365697959704642, -5.467109644685292480 ) ) ;
#40122 = CARTESIAN_POINT ( 'NONE',  ( 30.14155812561973846, -0.1321297161395868502, -9.228335630909516141 ) ) ;
#40121 = CIRCLE ( 'NONE', #22593, 1.000000000000000888 ) ;
#40123 = CIRCLE ( 'NONE', #25844, 1.000000000000000000 ) ;
#40124 = DIRECTION ( 'NONE',  ( 0.4067366430757984874, 0.9135454576426016438, -2.428612866367517941E-14 ) ) ;
#40125 = CARTESIAN_POINT ( 'NONE',  ( 28.21258359973596797, -14.01198379553896167, 20.50957957746030047 ) ) ;
#40126 = ORIENTED_EDGE ( 'NONE', *, *, #16587, .F. ) ;
#40127 = EDGE_CURVE ( 'NONE', #18785, #12475, #3067, .T. ) ;
#40128 = CIRCLE ( 'NONE', #31060, 0.5000000000000004441 ) ;
#40129 = CARTESIAN_POINT ( 'NONE',  ( 12.05832241004688399, 18.99596958976722760, -30.00000000000000000 ) ) ;
#40130 = ADVANCED_FACE ( 'NONE', ( #226 ), #32082, .T. ) ;
#40132 = CIRCLE ( 'NONE', #555, 1.000000000000000888 ) ;
#40131 = DIRECTION ( 'NONE',  ( 1.000000000000000000, 0.000000000000000000, 0.000000000000000000 ) ) ;
#40133 = ORIENTED_EDGE ( 'NONE', *, *, #10356, .F. ) ;
#40134 = CARTESIAN_POINT ( 'NONE',  ( 3.914034194965609892, 30.06176806842420035, 9.000000000000001776 ) ) ;
#40135 = B_SPLINE_CURVE_WITH_KNOTS ( 'NONE', 3,
 ( #28922, #19375, #31568, #32388 ),
 .UNSPECIFIED., .F., .F.,
 ( 4, 4 ),
 ( 0.000000000000000000, 1.000000000000000000 ),
 .UNSPECIFIED. ) ;
#40136 = CARTESIAN_POINT ( 'NONE',  ( -15.48853125999098701, -26.74269726803709446, -5.000000000000000000 ) ) ;
#40137 = LINE ( 'NONE', #24501, #15152 ) ;
#40138 = CARTESIAN_POINT ( 'NONE',  ( 2.821578699638708887, 27.66899254656360441, -17.62327247309158906 ) ) ;
#40139 = CARTESIAN_POINT ( 'NONE',  ( -13.63581098909220302, 27.45627467658446719, 11.00000000000000000 ) ) ;
#40140 = DIRECTION ( 'NONE',  ( -0.000000000000000000, -0.000000000000000000, -1.000000000000000000 ) ) ;
#40141 = CARTESIAN_POINT ( 'NONE',  ( -17.00000000000000000, 22.50000000000000355, 10.00000000000000000 ) ) ;
#40142 = CARTESIAN_POINT ( 'NONE',  ( -17.34253826607186966, 27.32041144404028188, 2.999999999999999112 ) ) ;
#40143 = CARTESIAN_POINT ( 'NONE',  ( 11.64304932069170029, 31.95750204166777309, 7.455539900862796721 ) ) ;
#40144 = EDGE_CURVE ( 'NONE', #2500, #7051, #28086, .T. ) ;
#40145 = CARTESIAN_POINT ( 'NONE',  ( 14.33090402811217068, 26.16159042914056698, 10.49999999999999467 ) ) ;
#40146 = CARTESIAN_POINT ( 'NONE',  ( 12.80256909985179092, 22.95103652443984998, -16.35598967180559171 ) ) ;
#40147 = CARTESIAN_POINT ( 'NONE',  ( -2.853172919594720192, 21.57294901687549427, 12.00000000000000000 ) ) ;
#40148 = CIRCLE ( 'NONE', #27830, 17.00000000000000000 ) ;
#40149 = EDGE_LOOP ( 'NONE', ( #98, #17616, #22380, #5539 ) ) ;
#40151 = CARTESIAN_POINT ( 'NONE',  ( -6.282361020112263716, 14.70372268239681190, 10.50000000000000533 ) ) ;
#40150 = CARTESIAN_POINT ( 'NONE',  ( -15.80284921427163880, 13.98913085816324298, -24.33118825873222590 ) ) ;
#40152 = LINE ( 'NONE', #3185, #2364 ) ;
#40153 = EDGE_CURVE ( 'NONE', #10907, #33136, #18514, .T. ) ;
#40154 = CARTESIAN_POINT ( 'NONE',  ( 15.48852768438595362, -26.74270545139661337, -5.474205978023907626 ) ) ;
#40155 = CARTESIAN_POINT ( 'NONE',  ( -12.11431921870781281, -16.53859995802357474, -30.00000000000001066 ) ) ;
#40156 = DIRECTION ( 'NONE',  ( 1.000000000000000000, 0.000000000000000000, 0.000000000000000000 ) ) ;
#40157 = CARTESIAN_POINT ( 'NONE',  ( 13.20319059294109820, 22.24725340734820023, -16.44263110745769296 ) ) ;
#40158 = AXIS2_PLACEMENT_3D ( 'NONE', #12852, #6157, #37441 ) ;
#40159 = ORIENTED_EDGE ( 'NONE', *, *, #29866, .T. ) ;
#40160 = CARTESIAN_POINT ( 'NONE',  ( 7.126083911573380725, 10.99048532364570008, 10.50000000000000000 ) ) ;
#40161 = CARTESIAN_POINT ( 'NONE',  ( -15.05265445420552517, -26.25383179241455878, -8.298612710543265436 ) ) ;
#40162 = CARTESIAN_POINT ( 'NONE',  ( -24.41232237690015339, -27.78610790073776471, 14.53008259254036716 ) ) ;
#40163 = EDGE_CURVE ( 'NONE', #24240, #26220, #12513, .T. ) ;
#40164 = CARTESIAN_POINT ( 'NONE',  ( -25.25503446062520396, -21.08292511653661805, -12.93509045432853455 ) ) ;
#40165 = CARTESIAN_POINT ( 'NONE',  ( 1.643370889305333371, -23.47708040232879867, -13.90816583911588467 ) ) ;
#40166 = CARTESIAN_POINT ( 'NONE',  ( 15.32296600055157398, 25.42927303866269284, -8.774763805950231088 ) ) ;
#40167 = CARTESIAN_POINT ( 'NONE',  ( 22.72267378955431028, 10.13466626278336769, -6.937383578344491930 ) ) ;
#40168 = DIRECTION ( 'NONE',  ( -1.000000000000000000, 0.000000000000000000, 0.000000000000000000 ) ) ;
#40169 = CARTESIAN_POINT ( 'NONE',  ( -5.311406340589158503, 37.48456040921701771, -6.284425160920512177 ) ) ;
#40170 = ORIENTED_EDGE ( 'NONE', *, *, #38050, .T. ) ;
#40171 = CARTESIAN_POINT ( 'NONE',  ( -20.37366957899092057, -3.711739399828728470, -27.85939855946655186 ) ) ;
#40172 = CARTESIAN_POINT ( 'NONE',  ( -16.52773037516168486, 27.09393310378289854, 14.53008259254011136 ) ) ;
#40173 = EDGE_LOOP ( 'NONE', ( #32699, #29400 ) ) ;
#40174 = DIRECTION ( 'NONE',  ( 1.000000000000000000, 0.000000000000000000, -0.000000000000000000 ) ) ;
#40175 = CARTESIAN_POINT ( 'NONE',  ( 22.38136799084939810, -15.36239294196588290, 23.00000000000000355 ) ) ;
#40176 = EDGE_CURVE ( 'NONE', #18778, #163, #34353, .T. ) ;
#40177 = CARTESIAN_POINT ( 'NONE',  ( -23.78118149983960095, 0.8666473556403437861, -19.53966836938907292 ) ) ;
#40178 = EDGE_CURVE ( 'NONE', #31871, #2935, #17083, .T. ) ;
#40179 = CARTESIAN_POINT ( 'NONE',  ( 34.88728563833267060, -12.83225574243902223, -7.568163508673742434 ) ) ;
#40180 = EDGE_CURVE ( 'NONE', #9757, #32909, #28249, .T. ) ;
#40181 = ORIENTED_EDGE ( 'NONE', *, *, #33465, .T. ) ;
#40182 = LINE ( 'NONE', #39783, #17422 ) ;
#40183 = ORIENTED_EDGE ( 'NONE', *, *, #29005, .T. ) ;
#40184 = AXIS2_PLACEMENT_3D ( 'NONE', #4262, #19705, #16663 ) ;
#40185 = FACE_OUTER_BOUND ( 'NONE', #39440, .T. ) ;
#40186 = CARTESIAN_POINT ( 'NONE',  ( -11.11016527260153630, 31.83082137946488643, 7.500000000000004441 ) ) ;
#40187 = CARTESIAN_POINT ( 'NONE',  ( 19.48557158514975285, -11.24999999999995737, 10.00000000000000000 ) ) ;
#40188 = VERTEX_POINT ( 'NONE', #18907 ) ;
#40189 = CARTESIAN_POINT ( 'NONE',  ( -3.201270893313360233, 28.76478025971673702, -16.65328222338712294 ) ) ;
#40190 = CARTESIAN_POINT ( 'NONE',  ( 0.3582258883630317636, 11.68927977431952137, 12.00000000000000000 ) ) ;
#40191 = LINE ( 'NONE', #12364, #21520 ) ;
#40192 = CARTESIAN_POINT ( 'NONE',  ( -11.16521142134453726, 24.66068167190384841, 6.000000000000000000 ) ) ;
#40193 = CARTESIAN_POINT ( 'NONE',  ( 21.15267166395459597, -16.25933725513243289, -18.65893975419588813 ) ) ;
#40194 = EDGE_CURVE ( 'NONE', #31812, #34769, #24605, .T. ) ;
#40195 = CARTESIAN_POINT ( 'NONE',  ( 19.41339421492355299, 15.80365212772844430, -7.907966775341815691 ) ) ;
#40196 = CARTESIAN_POINT ( 'NONE',  ( 9.218513230433782013, 21.74694333236849175, -21.18942908098420830 ) ) ;
#40197 = VERTEX_POINT ( 'NONE', #27648 ) ;
#40198 = CARTESIAN_POINT ( 'NONE',  ( -17.70440478334998247, 10.53096322850521460, -27.73763193811898375 ) ) ;
#40199 = CARTESIAN_POINT ( 'NONE',  ( 12.19805850000708780, -24.73057336344299628, -11.66080542555461008 ) ) ;
#40200 = NEXT_ASSEMBLY_USAGE_OCCURRENCE ( 'NAUO1', ' ', ' ', #32870, #27397, $ ) ;
#40201 = NEXT_ASSEMBLY_USAGE_OCCURRENCE ( 'NAUO2', ' ', ' ', #32870, #1580, $ ) ;
#40202 = NEXT_ASSEMBLY_USAGE_OCCURRENCE ( 'NAUO3', ' ', ' ', #32870, #3314, $ ) ;
#40203 = NEXT_ASSEMBLY_USAGE_OCCURRENCE ( 'NAUO4', ' ', ' ', #32870, #17230, $ ) ;
#40204 = NEXT_ASSEMBLY_USAGE_OCCURRENCE ( 'NAUO5', ' ', ' ', #32870, #1580, $ ) ;
#40205 = NEXT_ASSEMBLY_USAGE_OCCURRENCE ( 'NAUO6', ' ', ' ', #32870, #1580, $ ) ;
#40206 = NEXT_ASSEMBLY_USAGE_OCCURRENCE ( 'NAUO7', ' ', ' ', #32870, #17230, $ ) ;
#40207 = NEXT_ASSEMBLY_USAGE_OCCURRENCE ( 'NAUO8', ' ', ' ', #32870, #17230, $ ) ;
ENDSEC;
END-ISO-10303-21;
